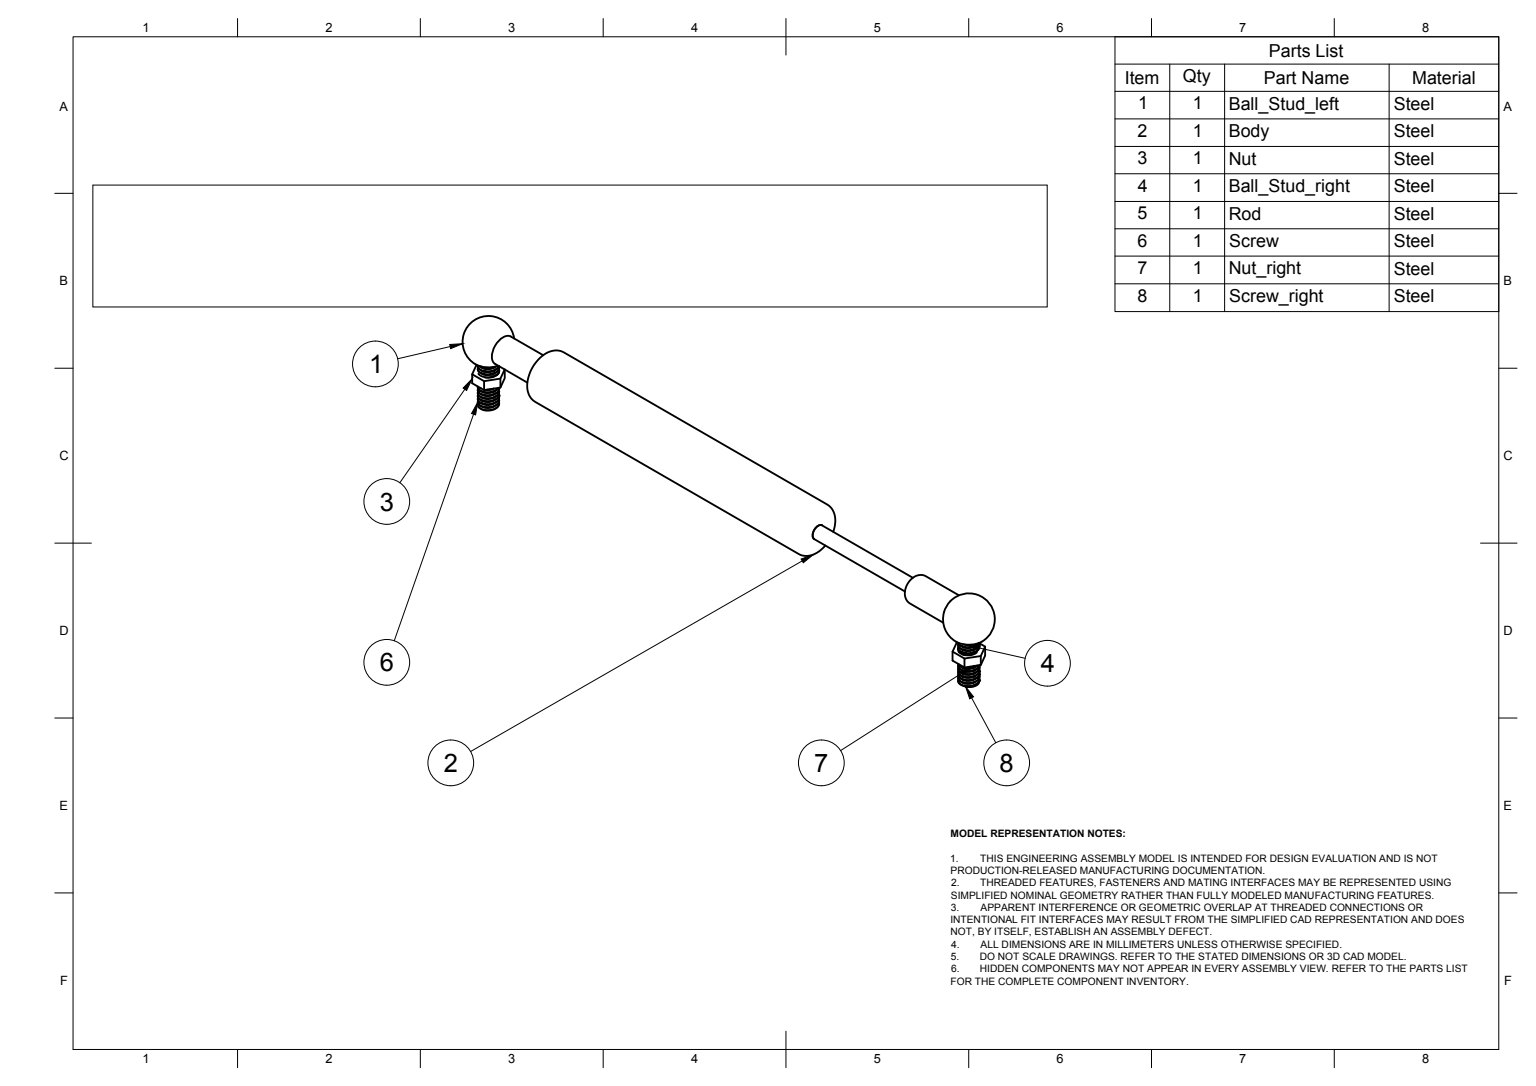
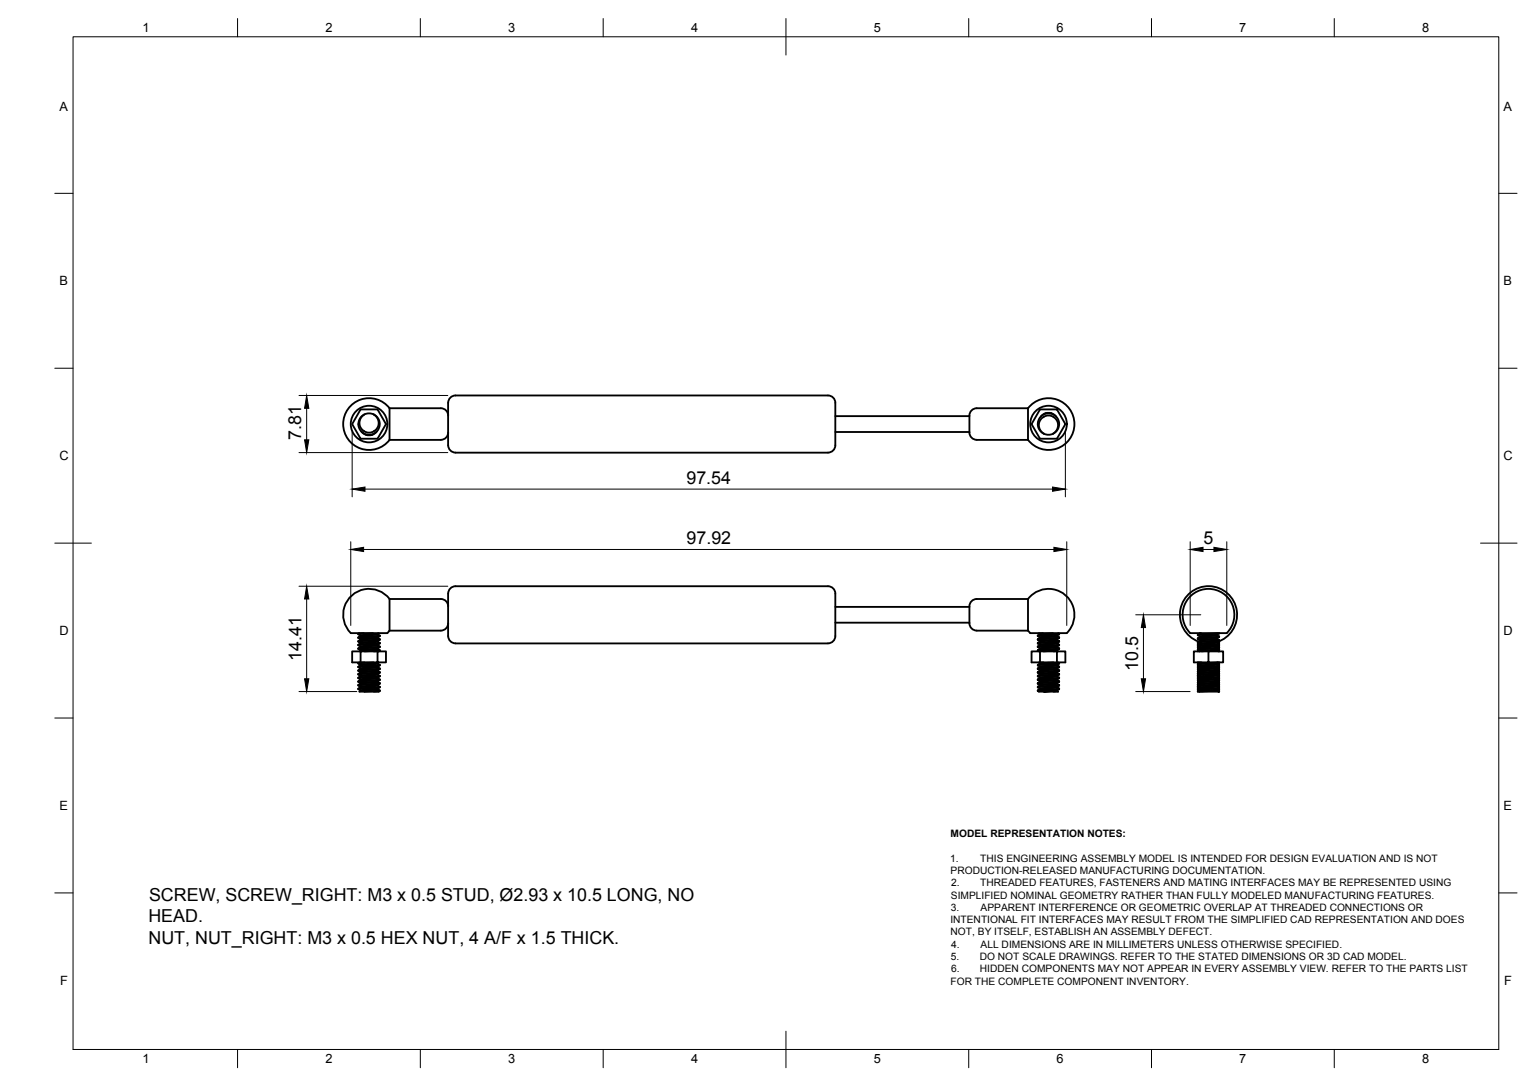
ISO-10303-21;
HEADER;
/* Generated by software containing ST-Developer
 * from STEP Tools, Inc. (www.steptools.com) 
 */

FILE_DESCRIPTION(
/* description */ (''),
/* implementation_level */ '2;1');

FILE_NAME(
/* name */ 'BR-109',
/* time_stamp */ '2026-10-04T22:13:49-07:00',
/* author */ (''),
/* organization */ (''),
/* preprocessor_version */ 'ST-DEVELOPER v20.2',
/* originating_system */ 'Autodesk Translation Framework v15.15.0.0',
/* authorisation */ '');

FILE_SCHEMA (('AUTOMOTIVE_DESIGN { 1 0 10303 214 3 1 1 }'));
ENDSEC;

DATA;
#10=MECHANICAL_DESIGN_GEOMETRIC_PRESENTATION_REPRESENTATION('',(#361,#362,
#363,#364,#365,#366,#367,#368,#369),#40734);
#11=ITEM_DEFINED_TRANSFORMATION($,$,#3265,#3474);
#12=ITEM_DEFINED_TRANSFORMATION($,$,#3284,#3475);
#13=ITEM_DEFINED_TRANSFORMATION($,$,#3299,#3476);
#14=ITEM_DEFINED_TRANSFORMATION($,$,#3320,#3477);
#15=ITEM_DEFINED_TRANSFORMATION($,$,#3340,#3478);
#16=ITEM_DEFINED_TRANSFORMATION($,$,#3351,#3479);
#17=ITEM_DEFINED_TRANSFORMATION($,$,#3402,#3480);
#18=ITEM_DEFINED_TRANSFORMATION($,$,#3423,#3481);
#19=(
REPRESENTATION_RELATIONSHIP($,$,#40766,#40765)
REPRESENTATION_RELATIONSHIP_WITH_TRANSFORMATION(#11)
SHAPE_REPRESENTATION_RELATIONSHIP()
);
#20=(
REPRESENTATION_RELATIONSHIP($,$,#40767,#40765)
REPRESENTATION_RELATIONSHIP_WITH_TRANSFORMATION(#12)
SHAPE_REPRESENTATION_RELATIONSHIP()
);
#21=(
REPRESENTATION_RELATIONSHIP($,$,#40768,#40765)
REPRESENTATION_RELATIONSHIP_WITH_TRANSFORMATION(#13)
SHAPE_REPRESENTATION_RELATIONSHIP()
);
#22=(
REPRESENTATION_RELATIONSHIP($,$,#40769,#40765)
REPRESENTATION_RELATIONSHIP_WITH_TRANSFORMATION(#14)
SHAPE_REPRESENTATION_RELATIONSHIP()
);
#23=(
REPRESENTATION_RELATIONSHIP($,$,#40770,#40765)
REPRESENTATION_RELATIONSHIP_WITH_TRANSFORMATION(#15)
SHAPE_REPRESENTATION_RELATIONSHIP()
);
#24=(
REPRESENTATION_RELATIONSHIP($,$,#40771,#40765)
REPRESENTATION_RELATIONSHIP_WITH_TRANSFORMATION(#16)
SHAPE_REPRESENTATION_RELATIONSHIP()
);
#25=(
REPRESENTATION_RELATIONSHIP($,$,#40772,#40765)
REPRESENTATION_RELATIONSHIP_WITH_TRANSFORMATION(#17)
SHAPE_REPRESENTATION_RELATIONSHIP()
);
#26=(
REPRESENTATION_RELATIONSHIP($,$,#40773,#40765)
REPRESENTATION_RELATIONSHIP_WITH_TRANSFORMATION(#18)
SHAPE_REPRESENTATION_RELATIONSHIP()
);
#27=CONTEXT_DEPENDENT_SHAPE_REPRESENTATION(#19,#40757);
#28=CONTEXT_DEPENDENT_SHAPE_REPRESENTATION(#20,#40758);
#29=CONTEXT_DEPENDENT_SHAPE_REPRESENTATION(#21,#40759);
#30=CONTEXT_DEPENDENT_SHAPE_REPRESENTATION(#22,#40760);
#31=CONTEXT_DEPENDENT_SHAPE_REPRESENTATION(#23,#40761);
#32=CONTEXT_DEPENDENT_SHAPE_REPRESENTATION(#24,#40762);
#33=CONTEXT_DEPENDENT_SHAPE_REPRESENTATION(#25,#40763);
#34=CONTEXT_DEPENDENT_SHAPE_REPRESENTATION(#26,#40764);
#35=NEXT_ASSEMBLY_USAGE_OCCURRENCE('Ball_Stud_left:1',
'Ball_Stud_left:1','Ball_Stud_left:1',#40775,#40776,'Ball_Stud_left:1');
#36=NEXT_ASSEMBLY_USAGE_OCCURRENCE('Body:1','Body:1','Body:1',#40775,#40777,
'Body:1');
#37=NEXT_ASSEMBLY_USAGE_OCCURRENCE('Nut:1','Nut:1','Nut:1',#40775,#40778,
'Nut:1');
#38=NEXT_ASSEMBLY_USAGE_OCCURRENCE('Ball_Stud_right:1',
'Ball_Stud_right:1','Ball_Stud_right:1',#40775,#40779,
'Ball_Stud_right:1');
#39=NEXT_ASSEMBLY_USAGE_OCCURRENCE('Rod:1','Rod:1','Rod:1',#40775,#40780,
'Rod:1');
#40=NEXT_ASSEMBLY_USAGE_OCCURRENCE('Screw:1','Screw:1','Screw:1',#40775,
#40781,'Screw:1');
#41=NEXT_ASSEMBLY_USAGE_OCCURRENCE('Nut_right:1','Nut_right:1',
'Nut_right:1',#40775,#40782,'Nut_right:1');
#42=NEXT_ASSEMBLY_USAGE_OCCURRENCE('Screw_right:1','Screw_right:1',
'Screw_right:1',#40775,#40783,'Screw_right:1');
#43=B_SPLINE_SURFACE_WITH_KNOTS('',3,3,((#5877,#5878,#5879,#5880,#5881,
#5882,#5883,#5884,#5885,#5886,#5887,#5888,#5889,#5890,#5891,#5892,#5893,
#5894,#5895,#5896,#5897,#5898,#5899,#5900),(#5901,#5902,#5903,#5904,#5905,
#5906,#5907,#5908,#5909,#5910,#5911,#5912,#5913,#5914,#5915,#5916,#5917,
#5918,#5919,#5920,#5921,#5922,#5923,#5924),(#5925,#5926,#5927,#5928,#5929,
#5930,#5931,#5932,#5933,#5934,#5935,#5936,#5937,#5938,#5939,#5940,#5941,
#5942,#5943,#5944,#5945,#5946,#5947,#5948),(#5949,#5950,#5951,#5952,#5953,
#5954,#5955,#5956,#5957,#5958,#5959,#5960,#5961,#5962,#5963,#5964,#5965,
#5966,#5967,#5968,#5969,#5970,#5971,#5972)),.UNSPECIFIED.,.F.,.F.,.F.,(4,
4),(4,1,1,1,1,1,1,1,1,1,1,1,1,1,1,1,1,1,1,1,1,4),(-0.000258182183401192,
0.0323763819078579),(11.855103081396,12.8491769023077,13.8429925410361,
14.8368081797645,15.8306238184928,16.8244394572212,17.8182550959496,18.8120707346779,
19.8058863734063,20.7997020121347,21.793517650863,22.7873332895914,23.7811489283198,
24.7749645670481,25.7687802057765,26.7625958445049,27.7564114832332,28.7502271219616,
29.74404276069,30.7378583994183,31.7316740381467,32.725489676875),
 .UNSPECIFIED.);
#44=B_SPLINE_SURFACE_WITH_KNOTS('',3,3,((#6139,#6140,#6141,#6142,#6143,
#6144,#6145,#6146,#6147,#6148,#6149,#6150,#6151,#6152,#6153,#6154,#6155,
#6156,#6157,#6158,#6159,#6160,#6161,#6162),(#6163,#6164,#6165,#6166,#6167,
#6168,#6169,#6170,#6171,#6172,#6173,#6174,#6175,#6176,#6177,#6178,#6179,
#6180,#6181,#6182,#6183,#6184,#6185,#6186),(#6187,#6188,#6189,#6190,#6191,
#6192,#6193,#6194,#6195,#6196,#6197,#6198,#6199,#6200,#6201,#6202,#6203,
#6204,#6205,#6206,#6207,#6208,#6209,#6210),(#6211,#6212,#6213,#6214,#6215,
#6216,#6217,#6218,#6219,#6220,#6221,#6222,#6223,#6224,#6225,#6226,#6227,
#6228,#6229,#6230,#6231,#6232,#6233,#6234)),.UNSPECIFIED.,.F.,.F.,.F.,(4,
4),(4,1,1,1,1,1,1,1,1,1,1,1,1,1,1,1,1,1,1,1,1,4),(-0.000227807970484936,
0.0323629493365531),(14.3984001269719,15.3922157657002,16.3860314044286,
17.379847043157,18.3736626818853,19.3674783206137,20.3612939593421,21.3551095980704,
22.3489252367988,23.3427408755272,24.3365565142555,25.3303721529839,26.3241877917123,
27.3180034304406,28.311819069169,29.3056347078974,30.2994503466257,31.2932659853541,
32.2870816240825,33.2808972628108,34.2747129015392,35.2685285402676),
 .UNSPECIFIED.);
#45=B_SPLINE_SURFACE_WITH_KNOTS('',3,3,((#19059,#19060,#19061,#19062,#19063,
#19064,#19065,#19066,#19067,#19068,#19069,#19070,#19071,#19072,#19073,#19074,
#19075,#19076,#19077,#19078,#19079,#19080,#19081,#19082,#19083,#19084,#19085,
#19086,#19087,#19088,#19089,#19090,#19091,#19092,#19093,#19094,#19095,#19096,
#19097,#19098,#19099,#19100,#19101,#19102,#19103,#19104,#19105,#19106,#19107,
#19108,#19109,#19110,#19111,#19112,#19113,#19114,#19115,#19116,#19117,#19118,
#19119,#19120,#19121,#19122,#19123,#19124,#19125,#19126,#19127,#19128,#19129,
#19130,#19131,#19132,#19133,#19134,#19135,#19136,#19137,#19138,#19139,#19140,
#19141,#19142,#19143,#19144,#19145,#19146,#19147,#19148,#19149,#19150,#19151,
#19152,#19153,#19154,#19155,#19156,#19157,#19158,#19159,#19160,#19161,#19162,
#19163,#19164,#19165,#19166,#19167,#19168,#19169,#19170,#19171,#19172,#19173,
#19174,#19175,#19176,#19177,#19178,#19179,#19180,#19181,#19182,#19183,#19184,
#19185,#19186,#19187,#19188,#19189,#19190,#19191,#19192,#19193,#19194,#19195,
#19196),(#19197,#19198,#19199,#19200,#19201,#19202,#19203,#19204,#19205,
#19206,#19207,#19208,#19209,#19210,#19211,#19212,#19213,#19214,#19215,#19216,
#19217,#19218,#19219,#19220,#19221,#19222,#19223,#19224,#19225,#19226,#19227,
#19228,#19229,#19230,#19231,#19232,#19233,#19234,#19235,#19236,#19237,#19238,
#19239,#19240,#19241,#19242,#19243,#19244,#19245,#19246,#19247,#19248,#19249,
#19250,#19251,#19252,#19253,#19254,#19255,#19256,#19257,#19258,#19259,#19260,
#19261,#19262,#19263,#19264,#19265,#19266,#19267,#19268,#19269,#19270,#19271,
#19272,#19273,#19274,#19275,#19276,#19277,#19278,#19279,#19280,#19281,#19282,
#19283,#19284,#19285,#19286,#19287,#19288,#19289,#19290,#19291,#19292,#19293,
#19294,#19295,#19296,#19297,#19298,#19299,#19300,#19301,#19302,#19303,#19304,
#19305,#19306,#19307,#19308,#19309,#19310,#19311,#19312,#19313,#19314,#19315,
#19316,#19317,#19318,#19319,#19320,#19321,#19322,#19323,#19324,#19325,#19326,
#19327,#19328,#19329,#19330,#19331,#19332,#19333,#19334),(#19335,#19336,
#19337,#19338,#19339,#19340,#19341,#19342,#19343,#19344,#19345,#19346,#19347,
#19348,#19349,#19350,#19351,#19352,#19353,#19354,#19355,#19356,#19357,#19358,
#19359,#19360,#19361,#19362,#19363,#19364,#19365,#19366,#19367,#19368,#19369,
#19370,#19371,#19372,#19373,#19374,#19375,#19376,#19377,#19378,#19379,#19380,
#19381,#19382,#19383,#19384,#19385,#19386,#19387,#19388,#19389,#19390,#19391,
#19392,#19393,#19394,#19395,#19396,#19397,#19398,#19399,#19400,#19401,#19402,
#19403,#19404,#19405,#19406,#19407,#19408,#19409,#19410,#19411,#19412,#19413,
#19414,#19415,#19416,#19417,#19418,#19419,#19420,#19421,#19422,#19423,#19424,
#19425,#19426,#19427,#19428,#19429,#19430,#19431,#19432,#19433,#19434,#19435,
#19436,#19437,#19438,#19439,#19440,#19441,#19442,#19443,#19444,#19445,#19446,
#19447,#19448,#19449,#19450,#19451,#19452,#19453,#19454,#19455,#19456,#19457,
#19458,#19459,#19460,#19461,#19462,#19463,#19464,#19465,#19466,#19467,#19468,
#19469,#19470,#19471,#19472),(#19473,#19474,#19475,#19476,#19477,#19478,
#19479,#19480,#19481,#19482,#19483,#19484,#19485,#19486,#19487,#19488,#19489,
#19490,#19491,#19492,#19493,#19494,#19495,#19496,#19497,#19498,#19499,#19500,
#19501,#19502,#19503,#19504,#19505,#19506,#19507,#19508,#19509,#19510,#19511,
#19512,#19513,#19514,#19515,#19516,#19517,#19518,#19519,#19520,#19521,#19522,
#19523,#19524,#19525,#19526,#19527,#19528,#19529,#19530,#19531,#19532,#19533,
#19534,#19535,#19536,#19537,#19538,#19539,#19540,#19541,#19542,#19543,#19544,
#19545,#19546,#19547,#19548,#19549,#19550,#19551,#19552,#19553,#19554,#19555,
#19556,#19557,#19558,#19559,#19560,#19561,#19562,#19563,#19564,#19565,#19566,
#19567,#19568,#19569,#19570,#19571,#19572,#19573,#19574,#19575,#19576,#19577,
#19578,#19579,#19580,#19581,#19582,#19583,#19584,#19585,#19586,#19587,#19588,
#19589,#19590,#19591,#19592,#19593,#19594,#19595,#19596,#19597,#19598,#19599,
#19600,#19601,#19602,#19603,#19604,#19605,#19606,#19607,#19608,#19609,#19610)),
 .UNSPECIFIED.,.F.,.F.,.F.,(4,4),(4,1,1,1,1,1,1,1,1,1,1,1,1,1,1,1,1,1,1,
1,1,1,1,1,1,1,1,1,1,1,1,1,1,1,1,1,1,1,1,1,1,1,1,1,1,1,1,1,1,1,1,1,1,1,1,
1,1,1,1,1,1,1,1,1,1,1,1,1,1,1,1,1,1,1,1,1,1,1,1,1,1,1,1,1,1,1,1,1,1,1,1,
1,1,1,1,1,1,1,1,1,1,1,1,1,1,1,1,1,1,1,1,1,1,1,1,1,1,1,1,1,1,1,1,1,1,1,1,
1,1,1,1,1,1,1,1,4),(-0.000231142210478152,0.0332102052225793),(8.30203615430837,
9.29477737004237,10.2875185857764,11.2802598015104,12.2730010172444,13.2657422329784,
14.2584834487124,15.2512246644464,16.2439658801804,17.2367070959144,18.2294483116484,
19.2221895273825,20.2149307431165,21.2076719588505,22.2004131745845,23.1931543903185,
24.1858956060525,25.1786368217865,26.1713780375205,27.1641192532545,28.1568604689885,
29.1496016847225,30.1423429004565,31.1350841161905,32.1278253319246,33.1205665476586,
34.1133077633926,35.1060489791266,36.0987901948606,37.0915314105946,38.0842726263286,
39.0770138420626,40.0697550577966,41.0624962735306,42.0552374892646,43.0479787049986,
44.0407199207326,45.0334611364667,46.0262023522007,47.0189435679347,48.0116847836687,
49.0044259994027,49.9971672151367,50.9899084308707,51.9826496466047,52.9753908623387,
53.9681320780727,54.9608732938067,55.9536145095407,56.9463557252747,57.9390969410088,
58.9318381567428,59.9245793724768,60.9173205882108,61.9100618039448,62.9028030196788,
63.8955442354128,64.8882854511468,65.8810266668808,66.8737678826148,67.8665090983488,
68.8592503140828,69.8519915298168,70.8447327455509,71.8374739612849,72.8302151770189,
73.8229563927529,74.8156976084869,75.8084388242209,76.8011800399549,77.7939212556889,
78.7866624714229,79.7794036871569,80.7721449028909,81.7648861186249,82.7576273343589,
83.750368550093,84.743109765827,85.735850981561,86.728592197295,87.721333413029,
88.714074628763,89.706815844497,90.699557060231,91.692298275965,92.685039491699,
93.677780707433,94.670521923167,95.663263138901,96.6560043546351,97.6487455703691,
98.6414867861031,99.6342280018371,100.626969217571,101.619710433305,102.612451649039,
103.605192864773,104.597934080507,105.590675296241,106.583416511975,107.576157727709,
108.568898943443,109.561640159177,110.554381374911,111.547122590645,112.539863806379,
113.532605022113,114.525346237847,115.518087453581,116.510828669315,117.503569885049,
118.496311100783,119.489052316517,120.481793532251,121.474534747985,122.467275963719,
123.460017179453,124.452758395187,125.445499610921,126.438240826655,127.430982042389,
128.423723258123,129.416464473857,130.409205689591,131.401946905325,132.394688121059,
133.387429336793,134.380170552527,135.372911768261,136.365652983995,137.358394199729,
138.351135415463,139.343876631197,140.336617846931,141.329359062665,142.322331420609),
 .UNSPECIFIED.);
#46=B_SPLINE_SURFACE_WITH_KNOTS('',3,3,((#19774,#19775,#19776,#19777,#19778,
#19779,#19780,#19781,#19782,#19783,#19784,#19785,#19786,#19787,#19788,#19789,
#19790,#19791,#19792,#19793,#19794,#19795,#19796,#19797,#19798,#19799,#19800,
#19801,#19802,#19803,#19804,#19805,#19806,#19807,#19808,#19809,#19810,#19811,
#19812,#19813,#19814,#19815,#19816,#19817,#19818,#19819,#19820,#19821,#19822,
#19823,#19824,#19825,#19826,#19827,#19828,#19829,#19830,#19831,#19832,#19833,
#19834,#19835,#19836,#19837,#19838,#19839,#19840,#19841,#19842,#19843,#19844,
#19845,#19846,#19847,#19848,#19849,#19850,#19851,#19852,#19853,#19854,#19855,
#19856,#19857,#19858,#19859,#19860,#19861,#19862,#19863,#19864,#19865,#19866,
#19867,#19868,#19869,#19870,#19871,#19872,#19873,#19874,#19875,#19876,#19877,
#19878,#19879,#19880,#19881,#19882,#19883,#19884,#19885,#19886,#19887,#19888,
#19889,#19890,#19891,#19892,#19893,#19894,#19895,#19896,#19897,#19898,#19899,
#19900,#19901,#19902,#19903,#19904,#19905,#19906,#19907,#19908,#19909,#19910,
#19911),(#19912,#19913,#19914,#19915,#19916,#19917,#19918,#19919,#19920,
#19921,#19922,#19923,#19924,#19925,#19926,#19927,#19928,#19929,#19930,#19931,
#19932,#19933,#19934,#19935,#19936,#19937,#19938,#19939,#19940,#19941,#19942,
#19943,#19944,#19945,#19946,#19947,#19948,#19949,#19950,#19951,#19952,#19953,
#19954,#19955,#19956,#19957,#19958,#19959,#19960,#19961,#19962,#19963,#19964,
#19965,#19966,#19967,#19968,#19969,#19970,#19971,#19972,#19973,#19974,#19975,
#19976,#19977,#19978,#19979,#19980,#19981,#19982,#19983,#19984,#19985,#19986,
#19987,#19988,#19989,#19990,#19991,#19992,#19993,#19994,#19995,#19996,#19997,
#19998,#19999,#20000,#20001,#20002,#20003,#20004,#20005,#20006,#20007,#20008,
#20009,#20010,#20011,#20012,#20013,#20014,#20015,#20016,#20017,#20018,#20019,
#20020,#20021,#20022,#20023,#20024,#20025,#20026,#20027,#20028,#20029,#20030,
#20031,#20032,#20033,#20034,#20035,#20036,#20037,#20038,#20039,#20040,#20041,
#20042,#20043,#20044,#20045,#20046,#20047,#20048,#20049),(#20050,#20051,
#20052,#20053,#20054,#20055,#20056,#20057,#20058,#20059,#20060,#20061,#20062,
#20063,#20064,#20065,#20066,#20067,#20068,#20069,#20070,#20071,#20072,#20073,
#20074,#20075,#20076,#20077,#20078,#20079,#20080,#20081,#20082,#20083,#20084,
#20085,#20086,#20087,#20088,#20089,#20090,#20091,#20092,#20093,#20094,#20095,
#20096,#20097,#20098,#20099,#20100,#20101,#20102,#20103,#20104,#20105,#20106,
#20107,#20108,#20109,#20110,#20111,#20112,#20113,#20114,#20115,#20116,#20117,
#20118,#20119,#20120,#20121,#20122,#20123,#20124,#20125,#20126,#20127,#20128,
#20129,#20130,#20131,#20132,#20133,#20134,#20135,#20136,#20137,#20138,#20139,
#20140,#20141,#20142,#20143,#20144,#20145,#20146,#20147,#20148,#20149,#20150,
#20151,#20152,#20153,#20154,#20155,#20156,#20157,#20158,#20159,#20160,#20161,
#20162,#20163,#20164,#20165,#20166,#20167,#20168,#20169,#20170,#20171,#20172,
#20173,#20174,#20175,#20176,#20177,#20178,#20179,#20180,#20181,#20182,#20183,
#20184,#20185,#20186,#20187),(#20188,#20189,#20190,#20191,#20192,#20193,
#20194,#20195,#20196,#20197,#20198,#20199,#20200,#20201,#20202,#20203,#20204,
#20205,#20206,#20207,#20208,#20209,#20210,#20211,#20212,#20213,#20214,#20215,
#20216,#20217,#20218,#20219,#20220,#20221,#20222,#20223,#20224,#20225,#20226,
#20227,#20228,#20229,#20230,#20231,#20232,#20233,#20234,#20235,#20236,#20237,
#20238,#20239,#20240,#20241,#20242,#20243,#20244,#20245,#20246,#20247,#20248,
#20249,#20250,#20251,#20252,#20253,#20254,#20255,#20256,#20257,#20258,#20259,
#20260,#20261,#20262,#20263,#20264,#20265,#20266,#20267,#20268,#20269,#20270,
#20271,#20272,#20273,#20274,#20275,#20276,#20277,#20278,#20279,#20280,#20281,
#20282,#20283,#20284,#20285,#20286,#20287,#20288,#20289,#20290,#20291,#20292,
#20293,#20294,#20295,#20296,#20297,#20298,#20299,#20300,#20301,#20302,#20303,
#20304,#20305,#20306,#20307,#20308,#20309,#20310,#20311,#20312,#20313,#20314,
#20315,#20316,#20317,#20318,#20319,#20320,#20321,#20322,#20323,#20324,#20325)),
 .UNSPECIFIED.,.F.,.F.,.F.,(4,4),(4,1,1,1,1,1,1,1,1,1,1,1,1,1,1,1,1,1,1,
1,1,1,1,1,1,1,1,1,1,1,1,1,1,1,1,1,1,1,1,1,1,1,1,1,1,1,1,1,1,1,1,1,1,1,1,
1,1,1,1,1,1,1,1,1,1,1,1,1,1,1,1,1,1,1,1,1,1,1,1,1,1,1,1,1,1,1,1,1,1,1,1,
1,1,1,1,1,1,1,1,1,1,1,1,1,1,1,1,1,1,1,1,1,1,1,1,1,1,1,1,1,1,1,1,1,1,1,1,
1,1,1,1,1,1,1,1,4),(-0.000203358763107571,0.0332327300170814),(11.6157025853675,
12.6086809632344,13.6014221789684,14.5941633947024,15.5869046104364,16.5796458261704,
17.5723870419044,18.5651282576385,19.5578694733725,20.5506106891065,21.5433519048405,
22.5360931205745,23.5288343363085,24.5215755520425,25.5143167677765,26.5070579835105,
27.4997991992445,28.4925404149785,29.4852816307125,30.4780228464465,31.4707640621806,
32.4635052779146,33.4562464936486,34.4489877093826,35.4417289251166,36.4344701408506,
37.4272113565846,38.4199525723186,39.4126937880526,40.4054350037866,41.3981762195206,
42.3909174352546,43.3836586509887,44.3763998667227,45.3691410824567,46.3618822981907,
47.3546235139247,48.3473647296587,49.3401059453927,50.3328471611267,51.3255883768607,
52.3183295925947,53.3110708083287,54.3038120240627,55.2965532397967,56.2892944555308,
57.2820356712648,58.2747768869988,59.2675181027328,60.2602593184668,61.2530005342008,
62.2457417499348,63.2384829656688,64.2312241814028,65.2239653971368,66.2167066128708,
67.2094478286048,68.2021890443388,69.1949302600729,70.1876714758069,71.1804126915409,
72.1731539072749,73.1658951230089,74.1586363387429,75.1513775544769,76.1441187702109,
77.1368599859449,78.1296012016789,79.1223424174129,80.1150836331469,81.107824848881,
82.100566064615,83.093307280349,84.086048496083,85.078789711817,86.071530927551,
87.064272143285,88.057013359019,89.049754574753,90.042495790487,91.035237006221,
92.027978221955,93.020719437689,94.0134606534231,95.0062018691571,95.9989430848911,
96.9916843006251,97.9844255163591,98.9771667320931,99.9699079478271,100.962649163561,
101.955390379295,102.948131595029,103.940872810763,104.933614026497,105.926355242231,
106.919096457965,107.911837673699,108.904578889433,109.897320105167,110.890061320901,
111.882802536635,112.875543752369,113.868284968103,114.861026183837,115.853767399571,
116.846508615305,117.839249831039,118.831991046773,119.824732262507,120.817473478241,
121.810214693975,122.802955909709,123.795697125443,124.788438341177,125.781179556911,
126.773920772645,127.766661988379,128.759403204113,129.752144419847,130.744885635581,
131.737626851315,132.730368067049,133.723109282783,134.715850498517,135.708591714251,
136.701332929985,137.694074145719,138.686815361453,139.679556577187,140.672297792921,
141.665039008655,142.657780224389,143.650521440123,144.643262655857,145.636003871591),
 .UNSPECIFIED.);
#47=B_SPLINE_SURFACE_WITH_KNOTS('',3,3,((#22334,#22335,#22336,#22337,#22338,
#22339,#22340,#22341,#22342,#22343,#22344,#22345,#22346,#22347,#22348,#22349,
#22350,#22351,#22352,#22353,#22354,#22355,#22356,#22357),(#22358,#22359,
#22360,#22361,#22362,#22363,#22364,#22365,#22366,#22367,#22368,#22369,#22370,
#22371,#22372,#22373,#22374,#22375,#22376,#22377,#22378,#22379,#22380,#22381),
(#22382,#22383,#22384,#22385,#22386,#22387,#22388,#22389,#22390,#22391,
#22392,#22393,#22394,#22395,#22396,#22397,#22398,#22399,#22400,#22401,#22402,
#22403,#22404,#22405),(#22406,#22407,#22408,#22409,#22410,#22411,#22412,
#22413,#22414,#22415,#22416,#22417,#22418,#22419,#22420,#22421,#22422,#22423,
#22424,#22425,#22426,#22427,#22428,#22429)),.UNSPECIFIED.,.F.,.F.,.F.,(4,
4),(4,1,1,1,1,1,1,1,1,1,1,1,1,1,1,1,1,1,1,1,1,4),(-0.000270002866089487,
0.0323833849707337),(11.8550912607133,12.8491769023077,13.8429925410361,
14.8368081797645,15.8306238184928,16.8244394572212,17.8182550959496,18.8120707346779,
19.8058863734063,20.7997020121347,21.793517650863,22.7873332895914,23.7811489283198,
24.7749645670481,25.7687802057765,26.7625958445049,27.7564114832332,28.7502271219616,
29.74404276069,30.7378583994183,31.7316740381467,32.725489676875),
 .UNSPECIFIED.);
#48=B_SPLINE_SURFACE_WITH_KNOTS('',3,3,((#22596,#22597,#22598,#22599,#22600,
#22601,#22602,#22603,#22604,#22605,#22606,#22607,#22608,#22609,#22610,#22611,
#22612,#22613,#22614,#22615,#22616,#22617,#22618,#22619),(#22620,#22621,
#22622,#22623,#22624,#22625,#22626,#22627,#22628,#22629,#22630,#22631,#22632,
#22633,#22634,#22635,#22636,#22637,#22638,#22639,#22640,#22641,#22642,#22643),
(#22644,#22645,#22646,#22647,#22648,#22649,#22650,#22651,#22652,#22653,
#22654,#22655,#22656,#22657,#22658,#22659,#22660,#22661,#22662,#22663,#22664,
#22665,#22666,#22667),(#22668,#22669,#22670,#22671,#22672,#22673,#22674,
#22675,#22676,#22677,#22678,#22679,#22680,#22681,#22682,#22683,#22684,#22685,
#22686,#22687,#22688,#22689,#22690,#22691)),.UNSPECIFIED.,.F.,.F.,.F.,(4,
4),(4,1,1,1,1,1,1,1,1,1,1,1,1,1,1,1,1,1,1,1,1,4),(-0.000235328167620964,
0.0323617480244609),(14.3982993132237,15.3922157657002,16.3860314044286,
17.379847043157,18.3736626818853,19.3674783206137,20.3612939593421,21.3551095980704,
22.3489252367988,23.3427408755272,24.3365565142555,25.3303721529839,26.3241877917123,
27.3180034304406,28.311819069169,29.3056347078974,30.2994503466257,31.2932659853541,
32.2870816240825,33.2808972628108,34.2747129015392,35.2685285402676),
 .UNSPECIFIED.);
#49=B_SPLINE_SURFACE_WITH_KNOTS('',3,3,((#39281,#39282,#39283,#39284,#39285,
#39286,#39287,#39288,#39289,#39290,#39291,#39292,#39293,#39294,#39295,#39296,
#39297,#39298,#39299,#39300,#39301,#39302,#39303,#39304,#39305,#39306,#39307,
#39308,#39309,#39310,#39311,#39312,#39313,#39314,#39315,#39316,#39317,#39318,
#39319,#39320,#39321,#39322,#39323,#39324,#39325,#39326,#39327,#39328,#39329,
#39330,#39331,#39332,#39333,#39334,#39335,#39336,#39337,#39338,#39339,#39340,
#39341,#39342,#39343,#39344,#39345,#39346,#39347,#39348,#39349,#39350,#39351,
#39352,#39353,#39354,#39355,#39356,#39357,#39358,#39359,#39360,#39361,#39362,
#39363,#39364,#39365,#39366,#39367,#39368,#39369,#39370,#39371,#39372,#39373,
#39374,#39375,#39376,#39377,#39378,#39379,#39380,#39381,#39382,#39383,#39384,
#39385,#39386,#39387,#39388,#39389,#39390,#39391,#39392,#39393,#39394,#39395,
#39396,#39397,#39398,#39399,#39400,#39401,#39402,#39403,#39404,#39405,#39406,
#39407,#39408,#39409,#39410,#39411,#39412,#39413,#39414,#39415,#39416,#39417,
#39418),(#39419,#39420,#39421,#39422,#39423,#39424,#39425,#39426,#39427,
#39428,#39429,#39430,#39431,#39432,#39433,#39434,#39435,#39436,#39437,#39438,
#39439,#39440,#39441,#39442,#39443,#39444,#39445,#39446,#39447,#39448,#39449,
#39450,#39451,#39452,#39453,#39454,#39455,#39456,#39457,#39458,#39459,#39460,
#39461,#39462,#39463,#39464,#39465,#39466,#39467,#39468,#39469,#39470,#39471,
#39472,#39473,#39474,#39475,#39476,#39477,#39478,#39479,#39480,#39481,#39482,
#39483,#39484,#39485,#39486,#39487,#39488,#39489,#39490,#39491,#39492,#39493,
#39494,#39495,#39496,#39497,#39498,#39499,#39500,#39501,#39502,#39503,#39504,
#39505,#39506,#39507,#39508,#39509,#39510,#39511,#39512,#39513,#39514,#39515,
#39516,#39517,#39518,#39519,#39520,#39521,#39522,#39523,#39524,#39525,#39526,
#39527,#39528,#39529,#39530,#39531,#39532,#39533,#39534,#39535,#39536,#39537,
#39538,#39539,#39540,#39541,#39542,#39543,#39544,#39545,#39546,#39547,#39548,
#39549,#39550,#39551,#39552,#39553,#39554,#39555,#39556),(#39557,#39558,
#39559,#39560,#39561,#39562,#39563,#39564,#39565,#39566,#39567,#39568,#39569,
#39570,#39571,#39572,#39573,#39574,#39575,#39576,#39577,#39578,#39579,#39580,
#39581,#39582,#39583,#39584,#39585,#39586,#39587,#39588,#39589,#39590,#39591,
#39592,#39593,#39594,#39595,#39596,#39597,#39598,#39599,#39600,#39601,#39602,
#39603,#39604,#39605,#39606,#39607,#39608,#39609,#39610,#39611,#39612,#39613,
#39614,#39615,#39616,#39617,#39618,#39619,#39620,#39621,#39622,#39623,#39624,
#39625,#39626,#39627,#39628,#39629,#39630,#39631,#39632,#39633,#39634,#39635,
#39636,#39637,#39638,#39639,#39640,#39641,#39642,#39643,#39644,#39645,#39646,
#39647,#39648,#39649,#39650,#39651,#39652,#39653,#39654,#39655,#39656,#39657,
#39658,#39659,#39660,#39661,#39662,#39663,#39664,#39665,#39666,#39667,#39668,
#39669,#39670,#39671,#39672,#39673,#39674,#39675,#39676,#39677,#39678,#39679,
#39680,#39681,#39682,#39683,#39684,#39685,#39686,#39687,#39688,#39689,#39690,
#39691,#39692,#39693,#39694),(#39695,#39696,#39697,#39698,#39699,#39700,
#39701,#39702,#39703,#39704,#39705,#39706,#39707,#39708,#39709,#39710,#39711,
#39712,#39713,#39714,#39715,#39716,#39717,#39718,#39719,#39720,#39721,#39722,
#39723,#39724,#39725,#39726,#39727,#39728,#39729,#39730,#39731,#39732,#39733,
#39734,#39735,#39736,#39737,#39738,#39739,#39740,#39741,#39742,#39743,#39744,
#39745,#39746,#39747,#39748,#39749,#39750,#39751,#39752,#39753,#39754,#39755,
#39756,#39757,#39758,#39759,#39760,#39761,#39762,#39763,#39764,#39765,#39766,
#39767,#39768,#39769,#39770,#39771,#39772,#39773,#39774,#39775,#39776,#39777,
#39778,#39779,#39780,#39781,#39782,#39783,#39784,#39785,#39786,#39787,#39788,
#39789,#39790,#39791,#39792,#39793,#39794,#39795,#39796,#39797,#39798,#39799,
#39800,#39801,#39802,#39803,#39804,#39805,#39806,#39807,#39808,#39809,#39810,
#39811,#39812,#39813,#39814,#39815,#39816,#39817,#39818,#39819,#39820,#39821,
#39822,#39823,#39824,#39825,#39826,#39827,#39828,#39829,#39830,#39831,#39832)),
 .UNSPECIFIED.,.F.,.F.,.F.,(4,4),(4,1,1,1,1,1,1,1,1,1,1,1,1,1,1,1,1,1,1,
1,1,1,1,1,1,1,1,1,1,1,1,1,1,1,1,1,1,1,1,1,1,1,1,1,1,1,1,1,1,1,1,1,1,1,1,
1,1,1,1,1,1,1,1,1,1,1,1,1,1,1,1,1,1,1,1,1,1,1,1,1,1,1,1,1,1,1,1,1,1,1,1,
1,1,1,1,1,1,1,1,1,1,1,1,1,1,1,1,1,1,1,1,1,1,1,1,1,1,1,1,1,1,1,1,1,1,1,1,
1,1,1,1,1,1,1,1,4),(-0.000234148554357844,0.0332108863658552),(8.30203615430837,
9.29477737004237,10.2875185857764,11.2802598015104,12.2730010172444,13.2657422329784,
14.2584834487124,15.2512246644464,16.2439658801804,17.2367070959144,18.2294483116484,
19.2221895273825,20.2149307431165,21.2076719588505,22.2004131745845,23.1931543903185,
24.1858956060525,25.1786368217865,26.1713780375205,27.1641192532545,28.1568604689885,
29.1496016847225,30.1423429004565,31.1350841161905,32.1278253319246,33.1205665476586,
34.1133077633926,35.1060489791266,36.0987901948606,37.0915314105946,38.0842726263286,
39.0770138420626,40.0697550577966,41.0624962735306,42.0552374892646,43.0479787049986,
44.0407199207326,45.0334611364667,46.0262023522007,47.0189435679347,48.0116847836687,
49.0044259994027,49.9971672151367,50.9899084308707,51.9826496466047,52.9753908623387,
53.9681320780727,54.9608732938067,55.9536145095407,56.9463557252747,57.9390969410088,
58.9318381567428,59.9245793724768,60.9173205882108,61.9100618039448,62.9028030196788,
63.8955442354128,64.8882854511468,65.8810266668808,66.8737678826148,67.8665090983488,
68.8592503140828,69.8519915298168,70.8447327455509,71.8374739612849,72.8302151770189,
73.8229563927529,74.8156976084869,75.8084388242209,76.8011800399549,77.7939212556889,
78.7866624714229,79.7794036871569,80.7721449028909,81.7648861186249,82.7576273343589,
83.750368550093,84.743109765827,85.735850981561,86.728592197295,87.721333413029,
88.714074628763,89.706815844497,90.699557060231,91.692298275965,92.685039491699,
93.677780707433,94.670521923167,95.663263138901,96.6560043546351,97.6487455703691,
98.6414867861031,99.6342280018371,100.626969217571,101.619710433305,102.612451649039,
103.605192864773,104.597934080507,105.590675296241,106.583416511975,107.576157727709,
108.568898943443,109.561640159177,110.554381374911,111.547122590645,112.539863806379,
113.532605022113,114.525346237847,115.518087453581,116.510828669315,117.503569885049,
118.496311100783,119.489052316517,120.481793532251,121.474534747985,122.467275963719,
123.460017179453,124.452758395187,125.445499610921,126.438240826655,127.430982042389,
128.423723258123,129.416464473857,130.409205689591,131.401946905325,132.394688121059,
133.387429336793,134.380170552527,135.372911768261,136.365652983995,137.358394199729,
138.351135415463,139.343876631197,140.336617846931,141.329359062665,142.322334426953),
 .UNSPECIFIED.);
#50=B_SPLINE_SURFACE_WITH_KNOTS('',3,3,((#39993,#39994,#39995,#39996,#39997,
#39998,#39999,#40000,#40001,#40002,#40003,#40004,#40005,#40006,#40007,#40008,
#40009,#40010,#40011,#40012,#40013,#40014,#40015,#40016,#40017,#40018,#40019,
#40020,#40021,#40022,#40023,#40024,#40025,#40026,#40027,#40028,#40029,#40030,
#40031,#40032,#40033,#40034,#40035,#40036,#40037,#40038,#40039,#40040,#40041,
#40042,#40043,#40044,#40045,#40046,#40047,#40048,#40049,#40050,#40051,#40052,
#40053,#40054,#40055,#40056,#40057,#40058,#40059,#40060,#40061,#40062,#40063,
#40064,#40065,#40066,#40067,#40068,#40069,#40070,#40071,#40072,#40073,#40074,
#40075,#40076,#40077,#40078,#40079,#40080,#40081,#40082,#40083,#40084,#40085,
#40086,#40087,#40088,#40089,#40090,#40091,#40092,#40093,#40094,#40095,#40096,
#40097,#40098,#40099,#40100,#40101,#40102,#40103,#40104,#40105,#40106,#40107,
#40108,#40109,#40110,#40111,#40112,#40113,#40114,#40115,#40116,#40117,#40118,
#40119,#40120,#40121,#40122,#40123,#40124,#40125,#40126,#40127,#40128,#40129,
#40130),(#40131,#40132,#40133,#40134,#40135,#40136,#40137,#40138,#40139,
#40140,#40141,#40142,#40143,#40144,#40145,#40146,#40147,#40148,#40149,#40150,
#40151,#40152,#40153,#40154,#40155,#40156,#40157,#40158,#40159,#40160,#40161,
#40162,#40163,#40164,#40165,#40166,#40167,#40168,#40169,#40170,#40171,#40172,
#40173,#40174,#40175,#40176,#40177,#40178,#40179,#40180,#40181,#40182,#40183,
#40184,#40185,#40186,#40187,#40188,#40189,#40190,#40191,#40192,#40193,#40194,
#40195,#40196,#40197,#40198,#40199,#40200,#40201,#40202,#40203,#40204,#40205,
#40206,#40207,#40208,#40209,#40210,#40211,#40212,#40213,#40214,#40215,#40216,
#40217,#40218,#40219,#40220,#40221,#40222,#40223,#40224,#40225,#40226,#40227,
#40228,#40229,#40230,#40231,#40232,#40233,#40234,#40235,#40236,#40237,#40238,
#40239,#40240,#40241,#40242,#40243,#40244,#40245,#40246,#40247,#40248,#40249,
#40250,#40251,#40252,#40253,#40254,#40255,#40256,#40257,#40258,#40259,#40260,
#40261,#40262,#40263,#40264,#40265,#40266,#40267,#40268),(#40269,#40270,
#40271,#40272,#40273,#40274,#40275,#40276,#40277,#40278,#40279,#40280,#40281,
#40282,#40283,#40284,#40285,#40286,#40287,#40288,#40289,#40290,#40291,#40292,
#40293,#40294,#40295,#40296,#40297,#40298,#40299,#40300,#40301,#40302,#40303,
#40304,#40305,#40306,#40307,#40308,#40309,#40310,#40311,#40312,#40313,#40314,
#40315,#40316,#40317,#40318,#40319,#40320,#40321,#40322,#40323,#40324,#40325,
#40326,#40327,#40328,#40329,#40330,#40331,#40332,#40333,#40334,#40335,#40336,
#40337,#40338,#40339,#40340,#40341,#40342,#40343,#40344,#40345,#40346,#40347,
#40348,#40349,#40350,#40351,#40352,#40353,#40354,#40355,#40356,#40357,#40358,
#40359,#40360,#40361,#40362,#40363,#40364,#40365,#40366,#40367,#40368,#40369,
#40370,#40371,#40372,#40373,#40374,#40375,#40376,#40377,#40378,#40379,#40380,
#40381,#40382,#40383,#40384,#40385,#40386,#40387,#40388,#40389,#40390,#40391,
#40392,#40393,#40394,#40395,#40396,#40397,#40398,#40399,#40400,#40401,#40402,
#40403,#40404,#40405,#40406),(#40407,#40408,#40409,#40410,#40411,#40412,
#40413,#40414,#40415,#40416,#40417,#40418,#40419,#40420,#40421,#40422,#40423,
#40424,#40425,#40426,#40427,#40428,#40429,#40430,#40431,#40432,#40433,#40434,
#40435,#40436,#40437,#40438,#40439,#40440,#40441,#40442,#40443,#40444,#40445,
#40446,#40447,#40448,#40449,#40450,#40451,#40452,#40453,#40454,#40455,#40456,
#40457,#40458,#40459,#40460,#40461,#40462,#40463,#40464,#40465,#40466,#40467,
#40468,#40469,#40470,#40471,#40472,#40473,#40474,#40475,#40476,#40477,#40478,
#40479,#40480,#40481,#40482,#40483,#40484,#40485,#40486,#40487,#40488,#40489,
#40490,#40491,#40492,#40493,#40494,#40495,#40496,#40497,#40498,#40499,#40500,
#40501,#40502,#40503,#40504,#40505,#40506,#40507,#40508,#40509,#40510,#40511,
#40512,#40513,#40514,#40515,#40516,#40517,#40518,#40519,#40520,#40521,#40522,
#40523,#40524,#40525,#40526,#40527,#40528,#40529,#40530,#40531,#40532,#40533,
#40534,#40535,#40536,#40537,#40538,#40539,#40540,#40541,#40542,#40543,#40544)),
 .UNSPECIFIED.,.F.,.F.,.F.,(4,4),(4,1,1,1,1,1,1,1,1,1,1,1,1,1,1,1,1,1,1,
1,1,1,1,1,1,1,1,1,1,1,1,1,1,1,1,1,1,1,1,1,1,1,1,1,1,1,1,1,1,1,1,1,1,1,1,
1,1,1,1,1,1,1,1,1,1,1,1,1,1,1,1,1,1,1,1,1,1,1,1,1,1,1,1,1,1,1,1,1,1,1,1,
1,1,1,1,1,1,1,1,1,1,1,1,1,1,1,1,1,1,1,1,1,1,1,1,1,1,1,1,1,1,1,1,1,1,1,1,
1,1,1,1,1,1,1,1,4),(-0.000206153515366958,0.0332359307550877),(11.6156993846295,
12.6086809632344,13.6014221789684,14.5941633947024,15.5869046104364,16.5796458261704,
17.5723870419044,18.5651282576385,19.5578694733725,20.5506106891065,21.5433519048405,
22.5360931205745,23.5288343363085,24.5215755520425,25.5143167677765,26.5070579835105,
27.4997991992445,28.4925404149785,29.4852816307125,30.4780228464465,31.4707640621806,
32.4635052779146,33.4562464936486,34.4489877093826,35.4417289251166,36.4344701408506,
37.4272113565846,38.4199525723186,39.4126937880526,40.4054350037866,41.3981762195206,
42.3909174352546,43.3836586509887,44.3763998667227,45.3691410824567,46.3618822981907,
47.3546235139247,48.3473647296587,49.3401059453927,50.3328471611267,51.3255883768607,
52.3183295925947,53.3110708083287,54.3038120240627,55.2965532397967,56.2892944555308,
57.2820356712648,58.2747768869988,59.2675181027328,60.2602593184668,61.2530005342008,
62.2457417499348,63.2384829656688,64.2312241814028,65.2239653971368,66.2167066128708,
67.2094478286048,68.2021890443388,69.1949302600729,70.1876714758069,71.1804126915409,
72.1731539072749,73.1658951230089,74.1586363387429,75.1513775544769,76.1441187702109,
77.1368599859449,78.1296012016789,79.1223424174129,80.1150836331469,81.107824848881,
82.100566064615,83.093307280349,84.086048496083,85.078789711817,86.071530927551,
87.064272143285,88.057013359019,89.049754574753,90.042495790487,91.035237006221,
92.027978221955,93.020719437689,94.0134606534231,95.0062018691571,95.9989430848911,
96.9916843006251,97.9844255163591,98.9771667320931,99.9699079478271,100.962649163561,
101.955390379295,102.948131595029,103.940872810763,104.933614026497,105.926355242231,
106.919096457965,107.911837673699,108.904578889433,109.897320105167,110.890061320901,
111.882802536635,112.875543752369,113.868284968103,114.861026183837,115.853767399571,
116.846508615305,117.839249831039,118.831991046773,119.824732262507,120.817473478241,
121.810214693975,122.802955909709,123.795697125443,124.788438341177,125.781179556911,
126.773920772645,127.766661988379,128.759403204113,129.752144419847,130.744885635581,
131.737626851315,132.730368067049,133.723109282783,134.715850498517,135.708591714251,
136.701332929985,137.694074145719,138.686815361453,139.679556577187,140.672297792921,
141.665039008655,142.657780224389,143.650521440123,144.643262655857,145.636003871591),
 .UNSPECIFIED.);
#51=B_SPLINE_CURVE_WITH_KNOTS('',3,(#4121,#4122,#4123,#4124,#4125,#4126),
 .UNSPECIFIED.,.F.,.F.,(4,1,1,4),(30.4992669120821,30.7378583994183,31.7316740381467,
32.725489676875),.UNSPECIFIED.);
#52=B_SPLINE_CURVE_WITH_KNOTS('',3,(#4129,#4130,#4131,#4132,#4133,#4134,
#4135,#4136,#4137,#4138,#4139,#4140,#4141,#4142,#4143,#4144,#4145,#4146,
#4147,#4148,#4149,#4150,#4151,#4152,#4153,#4154,#4155,#4156,#4157,#4158,
#4159,#4160,#4161,#4162,#4163,#4164,#4165,#4166,#4167,#4168,#4169,#4170,
#4171,#4172,#4173,#4174,#4175,#4176,#4177,#4178,#4179,#4180,#4181,#4182,
#4183,#4184,#4185,#4186,#4187,#4188,#4189,#4190,#4191,#4192,#4193,#4194,
#4195,#4196,#4197,#4198,#4199,#4200,#4201,#4202,#4203,#4204),
 .UNSPECIFIED.,.F.,.F.,(4,3,3,3,3,3,3,3,3,3,3,3,3,3,3,3,3,3,3,3,3,3,3,3,
3,4),(30.5007322636873,30.6122727264591,30.7237376230315,30.8351702081999,
30.9496941524884,31.0612649927854,31.1772654890698,31.2932659853541,31.405444381662,
31.5174234643071,31.629291154361,31.7410902071455,31.8528632800448,31.9647326752084,
32.0766471573347,32.1887699843063,32.2870816240825,32.398548943329,32.5098233581226,
32.6209912335388,32.7320964774763,32.8431829042999,32.9543713853473,33.0656134824414,
33.1770570913779,33.2478062575977),.UNSPECIFIED.);
#53=B_SPLINE_CURVE_WITH_KNOTS('',3,(#4210,#4211,#4212,#4213,#4214,#4215,
#4216,#4217,#4218,#4219,#4220,#4221,#4222,#4223,#4224,#4225,#4226,#4227,
#4228,#4229,#4230,#4231,#4232,#4233,#4234,#4235,#4236,#4237,#4238,#4239,
#4240,#4241,#4242,#4243,#4244,#4245,#4246,#4247,#4248,#4249,#4250,#4251,
#4252,#4253,#4254,#4255,#4256,#4257,#4258,#4259,#4260,#4261,#4262,#4263,
#4264,#4265,#4266,#4267,#4268,#4269,#4270,#4271,#4272,#4273,#4274,#4275,
#4276,#4277,#4278,#4279,#4280,#4281,#4282,#4283,#4284,#4285,#4286,#4287,
#4288,#4289,#4290,#4291,#4292,#4293,#4294,#4295,#4296,#4297,#4298,#4299,
#4300,#4301,#4302,#4303,#4304,#4305,#4306,#4307,#4308,#4309,#4310,#4311,
#4312,#4313,#4314,#4315,#4316,#4317,#4318,#4319,#4320,#4321),
 .UNSPECIFIED.,.F.,.F.,(4,3,3,3,3,3,3,3,3,3,3,3,3,3,3,3,3,3,3,3,3,3,3,3,
3,3,3,3,3,3,3,3,3,3,3,3,3,4),(24.2171494664266,24.3287289861615,24.4404061429661,
24.5521266745184,24.6640652186713,24.7749645670481,24.8869176317094,24.9986729372709,
25.1103179593314,25.2218958291666,25.3334495814181,25.4451043023639,25.5568063273599,
25.668723124984,25.7687802057765,25.8807765547188,25.9925749208264,26.104262837802,
26.2158833658169,26.3274794682339,26.4391757243447,26.550918903972,26.6628756909807,
26.7625958445049,26.8745949120742,26.9863967358013,27.0980885559922,27.2097134207251,
27.3213142818085,27.4330159084715,27.5447648029427,27.6567278002384,27.7564114832332,
27.8729397438563,27.9891469003203,28.1051613568161,28.2209618754298,28.2743338823081),
 .UNSPECIFIED.);
#54=B_SPLINE_CURVE_WITH_KNOTS('',3,(#4322,#4323,#4324,#4325,#4326,#4327),
 .UNSPECIFIED.,.F.,.F.,(4,1,1,4),(28.2743354175824,28.7502271219616,29.74404276069,
30.4992669120821),.UNSPECIFIED.);
#55=B_SPLINE_CURVE_WITH_KNOTS('',3,(#4329,#4330,#4331,#4332,#4333,#4334,
#4335,#4336,#4337,#4338,#4339,#4340,#4341,#4342,#4343,#4344,#4345,#4346,
#4347,#4348,#4349,#4350,#4351,#4352,#4353,#4354,#4355,#4356,#4357,#4358,
#4359,#4360,#4361,#4362,#4363,#4364,#4365,#4366,#4367,#4368,#4369,#4370,
#4371,#4372,#4373,#4374,#4375,#4376,#4377,#4378,#4379,#4380,#4381,#4382,
#4383,#4384,#4385,#4386,#4387,#4388,#4389,#4390,#4391,#4392),
 .UNSPECIFIED.,.F.,.F.,(4,3,3,3,3,3,3,3,3,3,3,3,3,3,3,3,3,3,3,3,3,4),(28.2743338823081,
28.311819069169,28.4238155021246,28.5356139507129,28.6473019491837,28.7589225575854,
28.8705187391566,28.9822150718989,29.0939583268957,29.2059151862192,29.3056347078974,
29.4176340985753,29.5294362480819,29.6411283954428,29.7527535881624,29.8643547774776,
29.9760567301189,30.0878059498508,30.1997692670012,30.2994503466257,30.4112462518584,
30.5007322636873),.UNSPECIFIED.);
#56=B_SPLINE_CURVE_WITH_KNOTS('',3,(#4393,#4394,#4395,#4396,#4397,#4398,
#4399,#4400,#4401,#4402,#4403,#4404,#4405,#4406,#4407,#4408,#4409,#4410,
#4411,#4412,#4413,#4414,#4415,#4416,#4417,#4418,#4419,#4420,#4421,#4422,
#4423,#4424,#4425,#4426,#4427,#4428,#4429,#4430,#4431,#4432,#4433,#4434,
#4435,#4436,#4437,#4438,#4439,#4440,#4441,#4442,#4443,#4444,#4445,#4446,
#4447,#4448,#4449,#4450,#4451,#4452,#4453,#4454,#4455,#4456,#4457,#4458,
#4459,#4460,#4461,#4462,#4463,#4464,#4465,#4466,#4467,#4468,#4469,#4470,
#4471,#4472,#4473,#4474,#4475,#4476,#4477,#4478,#4479,#4480,#4481,#4482,
#4483,#4484,#4485,#4486,#4487,#4488,#4489,#4490,#4491,#4492,#4493,#4494,
#4495,#4496,#4497,#4498,#4499,#4500,#4501,#4502,#4503,#4504,#4505,#4506,
#4507),.UNSPECIFIED.,.F.,.F.,(4,3,3,3,3,3,3,3,3,3,3,3,3,3,3,3,3,3,3,3,3,
3,3,3,3,3,3,3,3,3,3,3,3,3,3,3,3,3,4),(24.2164788938612,24.3284578108245,
24.3365565142555,24.4485244285209,24.560294535519,24.6719543195167,24.7835468869861,
24.8951152477273,25.0067843218568,25.1185005830992,25.2304312375024,25.3303721529839,
25.4423485822127,25.5541272382699,25.6657955861649,25.7773967178561,25.8889736286533,
26.0006511630903,26.1123758489851,26.2243147601803,26.3241877917123,26.4361661670213,
26.5479468651215,26.6596173118309,26.7712205948806,26.8827997054225,26.9944794966149,
27.1062064741593,27.2181477050763,27.3180034304406,27.4292887012154,27.5403774827401,
27.651357678686,27.7622734955792,27.8731690428523,27.9841643917093,28.095212635599,
28.2064596772962,28.2743338817915),.UNSPECIFIED.);
#57=B_SPLINE_CURVE_WITH_KNOTS('',3,(#4513,#4514,#4515,#4516,#4517,#4518,
#4519,#4520,#4521,#4522,#4523,#4524,#4525,#4526,#4527,#4528,#4529,#4530,
#4531,#4532,#4533,#4534,#4535,#4536,#4537,#4538,#4539,#4540,#4541,#4542,
#4543,#4544,#4545,#4546,#4547,#4548,#4549,#4550,#4551,#4552,#4553,#4554,
#4555,#4556,#4557,#4558,#4559,#4560,#4561,#4562,#4563,#4564,#4565,#4566,
#4567,#4568,#4569,#4570,#4571,#4572,#4573),.UNSPECIFIED.,.F.,.F.,(4,3,3,
3,3,3,3,3,3,3,3,3,3,3,3,3,3,3,3,3,4),(15.707963267949,15.818355090934,15.9287111247549,
16.0430411946733,16.1535358156933,16.2697836100609,16.3860314044286,16.4981421037095,
16.6100544113457,16.7218559281154,16.8335894986427,16.9452978703484,17.0571042296374,
17.1689564942254,17.2810192004281,17.379847043157,17.4919974773912,17.6039638386448,
17.7158203932178,17.8276366370513,17.9335665904152),.UNSPECIFIED.);
#58=B_SPLINE_CURVE_WITH_KNOTS('',3,(#4575,#4576,#4577,#4578,#4579),
 .UNSPECIFIED.,.F.,.F.,(4,1,4),(14.3984001269719,15.3922157657002,15.7079548812379),
 .UNSPECIFIED.);
#59=B_SPLINE_CURVE_WITH_KNOTS('',3,(#4583,#4584,#4585,#4586,#4587,#4588,
#4589,#4590,#4591,#4592,#4593,#4594,#4595,#4596,#4597,#4598,#4599,#4600,
#4601,#4602,#4603,#4604,#4605,#4606,#4607,#4608,#4609,#4610,#4611,#4612,
#4613,#4614,#4615,#4616,#4617,#4618,#4619,#4620,#4621,#4622,#4623,#4624,
#4625,#4626,#4627,#4628,#4629,#4630,#4631,#4632,#4633,#4634),
 .UNSPECIFIED.,.F.,.F.,(4,3,3,3,3,3,3,3,3,3,3,3,3,3,3,3,3,4),(13.8759340267632,
13.9874055240017,14.0986819048936,14.2098503830277,14.3209548725418,14.4320391923179,
14.5432235672466,14.6544603986013,14.7658970889775,14.8368081797645,14.9473475531393,
15.0577376284281,15.1680237022244,15.2782509068263,15.3885311804989,15.4988322555113,
15.6093107358845,15.707963267949),.UNSPECIFIED.);
#60=B_SPLINE_CURVE_WITH_KNOTS('',3,(#4635,#4636,#4637,#4638,#4639,#4640,
#4641),.UNSPECIFIED.,.F.,.F.,(4,1,1,1,4),(15.707963267949,15.8306238184928,
16.8244394572212,17.8182550959496,17.9344079850994),.UNSPECIFIED.);
#61=B_SPLINE_CURVE_WITH_KNOTS('',3,(#4647,#4648,#4649,#4650,#4651,#4652,
#4653,#4654,#4655,#4656,#4657,#4658,#4659,#4660,#4661,#4662,#4663,#4664,
#4665,#4666,#4667,#4668,#4669,#4670,#4671,#4672,#4673,#4674,#4675,#4676,
#4677,#4678,#4679,#4680,#4681,#4682,#4683,#4684,#4685,#4686,#4687,#4688,
#4689,#4690,#4691,#4692,#4693,#4694,#4695,#4696,#4697,#4698),
 .UNSPECIFIED.,.F.,.F.,(4,3,3,3,3,3,3,3,3,3,3,3,3,3,3,3,3,4),(18.2326852175056,
18.3501141129404,18.4675228039056,18.5850446472557,18.7026282574228,18.8204305181141,
18.8824971358389,18.9989861703458,19.1152627236631,19.2314232752781,19.3475198007835,
19.4636041624104,19.5798208788147,19.6961099863659,19.8126414543351,19.8763127745673,
20.0320230471778,20.1591088879388),.UNSPECIFIED.);
#62=B_SPLINE_CURVE_WITH_KNOTS('',3,(#4700,#4701,#4702,#4703,#4704,#4705,
#4706,#4707,#4708,#4709,#4710,#4711,#4712,#4713),.UNSPECIFIED.,.F.,.F.,
(4,2,2,2,2,2,4),(-0.0902879860330804,-0.0695195013464431,-0.0576139772363393,
-0.0451609786697689,-0.0307684913612755,-0.00741601523602112,0.),
 .UNSPECIFIED.);
#63=B_SPLINE_CURVE_WITH_KNOTS('',3,(#4716,#4717,#4718,#4719,#4720,#4721,
#4722,#4723,#4724,#4725,#4726,#4727,#4728,#4729,#4730,#4731,#4732,#4733,
#4734,#4735,#4736,#4737,#4738,#4739,#4740,#4741,#4742,#4743,#4744,#4745,
#4746,#4747,#4748,#4749,#4750,#4751,#4752,#4753,#4754,#4755,#4756,#4757,
#4758,#4759,#4760,#4761,#4762,#4763,#4764,#4765,#4766,#4767,#4768,#4769,
#4770,#4771,#4772,#4773,#4774,#4775,#4776,#4777,#4778,#4779,#4780,#4781,
#4782,#4783,#4784,#4785,#4786,#4787,#4788,#4789,#4790,#4791,#4792,#4793,
#4794,#4795,#4796,#4797),.UNSPECIFIED.,.F.,.F.,(4,2,2,2,2,2,2,2,2,2,2,2,
2,2,2,2,2,2,2,2,2,2,2,2,2,2,2,2,2,2,2,2,2,2,2,2,2,2,2,2,4),(-1.10310963530152,
-1.09840428209197,-1.07722214007663,-1.06150851698653,-1.04868281780305,
-1.03819235320156,-1.02138418259208,-0.999282379625926,-0.990602595865436,
-0.983495936132868,-0.976570972649354,-0.961692691255592,-0.940952466821429,
-0.926313970937883,-0.916002211406824,-0.902436796120762,-0.870391217176744,
-0.860477072002617,-0.854465023776041,-0.845070439673182,-0.819245833374607,
-0.806702496780286,-0.79543475800065,-0.784817093076859,-0.762133674934839,
-0.745228751131369,-0.734731689538218,-0.728719271759347,-0.719808072857297,
-0.694096875566972,-0.681109182806924,-0.669588324732776,-0.658941721449021,
-0.638880453131988,-0.614447417440931,-0.606635107300723,-0.600344143431757,
-0.588300966408003,-0.564446554319691,-0.552834380572,-0.552725405623167),
 .UNSPECIFIED.);
#64=B_SPLINE_CURVE_WITH_KNOTS('',3,(#4803,#4804,#4805,#4806,#4807,#4808,
#4809,#4810,#4811,#4812,#4813,#4814,#4815,#4816,#4817,#4818,#4819,#4820,
#4821,#4822,#4823,#4824,#4825,#4826,#4827,#4828,#4829,#4830,#4831,#4832,
#4833,#4834,#4835,#4836,#4837,#4838,#4839,#4840,#4841,#4842,#4843,#4844,
#4845,#4846,#4847,#4848,#4849,#4850,#4851,#4852,#4853,#4854,#4855,#4856,
#4857),.UNSPECIFIED.,.F.,.F.,(4,3,3,3,3,3,3,3,3,3,3,3,3,3,3,3,3,3,4),(11.9491877790605,
12.0704897196116,12.1879350799606,12.3052738059049,12.4225558808697,12.539831191545,
12.6572286481437,12.7747004780911,12.892380281892,12.9196033034688,13.0391446098747,
13.1558912766851,13.2725228710644,13.3890907032798,13.5108014661389,13.6274735002162,
13.7442192750413,13.8611645569831,13.8759337547162),.UNSPECIFIED.);
#65=B_SPLINE_CURVE_WITH_KNOTS('',3,(#4858,#4859,#4860,#4861,#4862,#4863,
#4864,#4865,#4866,#4867,#4868,#4869,#4870,#4871,#4872,#4873,#4874,#4875,
#4876,#4877,#4878,#4879,#4880,#4881,#4882,#4883,#4884,#4885,#4886,#4887,
#4888,#4889,#4890,#4891,#4892,#4893,#4894,#4895,#4896,#4897,#4898,#4899,
#4900,#4901,#4902,#4903,#4904,#4905,#4906,#4907,#4908,#4909,#4910,#4911,
#4912,#4913,#4914,#4915,#4916,#4917,#4918,#4919,#4920,#4921,#4922,#4923,
#4924,#4925,#4926,#4927,#4928,#4929,#4930,#4931,#4932,#4933,#4934,#4935,
#4936,#4937,#4938,#4939,#4940,#4941,#4942,#4943,#4944,#4945,#4946,#4947,
#4948,#4949,#4950,#4951,#4952,#4953,#4954,#4955,#4956,#4957,#4958,#4959,
#4960,#4961,#4962,#4963,#4964,#4965,#4966,#4967,#4968,#4969,#4970,#4971,
#4972,#4973,#4974,#4975,#4976,#4977,#4978),.UNSPECIFIED.,.F.,.F.,(4,3,3,
3,3,3,3,3,3,3,3,3,3,3,3,3,3,3,3,3,3,3,3,3,3,3,3,3,3,3,3,3,3,3,3,3,3,3,3,
3,4),(13.8759337553363,13.9134189421971,14.0311296480262,14.1486252389434,
14.2660024664715,14.383311313252,14.5006016500783,14.6180056712398,14.735473475376,
14.8531565546079,14.9072345809255,15.0249483953848,15.1424479004606,15.2598295359287,
15.377143269917,15.4944389593616,15.6118489804661,15.7293231625642,15.8470131172698,
15.9010502196539,16.0185862160695,16.1359071716103,16.2531099559165,16.3702448724762,
16.4873621130608,16.604595636191,16.7218941812094,16.8394118468141,16.8948658583822,
17.0127678116824,17.1304532100569,17.2480191781504,17.365515344718,17.4829912252123,
17.6005766740717,17.7182237949846,17.8360809197351,17.8886814971106,18.006475161737,
18.1240829762214,18.2326852175056),.UNSPECIFIED.);
#66=B_SPLINE_CURVE_WITH_KNOTS('',3,(#4980,#4981,#4982,#4983,#4984,#4985,
#4986,#4987,#4988,#4989,#4990,#4991,#4992,#4993,#4994,#4995,#4996,#4997,
#4998,#4999,#5000,#5001,#5002,#5003,#5004,#5005,#5006,#5007,#5008,#5009,
#5010,#5011,#5012,#5013,#5014,#5015,#5016,#5017,#5018,#5019,#5020,#5021,
#5022,#5023,#5024,#5025,#5026,#5027,#5028,#5029,#5030,#5031,#5032,#5033,
#5034,#5035,#5036,#5037,#5038,#5039,#5040,#5041,#5042,#5043,#5044,#5045,
#5046,#5047,#5048,#5049,#5050,#5051,#5052,#5053,#5054,#5055,#5056,#5057,
#5058,#5059),.UNSPECIFIED.,.F.,.F.,(4,2,2,2,2,2,2,2,2,2,2,2,2,2,2,2,2,2,
2,2,2,2,2,2,2,2,2,2,2,2,2,2,2,2,2,2,2,2,2,4),(-0.552725405623167,-0.541977170966905,
-0.53084957666005,-0.51866977594079,-0.490571100145663,-0.481793473449696,
-0.475745498289177,-0.464874554957004,-0.446785851085663,-0.425816502562416,
-0.415167087894251,-0.403760289275286,-0.390983977795993,-0.365216310304077,
-0.356082527804832,-0.35005340954438,-0.33973200687133,-0.323398146844299,
-0.299824069413248,-0.289158384786419,-0.277737870662131,-0.264943180238732,
-0.233016973059306,-0.226580840545827,-0.219169303547567,-0.209851774465103,
-0.182807487580695,-0.169162145546328,-0.158906935173509,-0.144586539612125,
-0.124772548138701,-0.107597516249468,-0.10099011512184,-0.0938729126324881,
-0.0851219325742436,-0.0624426869455938,-0.0456861069530859,-0.0353317986472908,
-0.0229676387407706,-0.00036925595930691),.UNSPECIFIED.);
#67=B_SPLINE_CURVE_WITH_KNOTS('',3,(#5060,#5061,#5062,#5063,#5064,#5065,
#5066,#5067,#5068,#5069,#5070,#5071,#5072,#5073,#5074,#5075,#5076,#5077,
#5078,#5079,#5080,#5081,#5082,#5083,#5084,#5085,#5086,#5087,#5088,#5089,
#5090,#5091,#5092,#5093,#5094,#5095,#5096,#5097,#5098,#5099,#5100,#5101,
#5102,#5103,#5104,#5105,#5106,#5107,#5108,#5109,#5110,#5111,#5112,#5113,
#5114),.UNSPECIFIED.,.F.,.F.,(4,3,3,3,3,3,3,3,3,3,3,3,3,3,3,3,3,3,4),(-10.1357873115492,
-9.96754509954774,-9.93815638728366,-9.82046673168105,-9.70299196205392,
-9.58563539619237,-9.46834701434813,-9.35107690841475,-9.23369261088505,
-9.11624426811025,-8.99858002714185,-8.94434074855529,-8.82667899846583,
-8.7091951599211,-8.59183899812951,-8.47453671765872,-8.35726362182951,
-8.23992726492522,-8.20946475857041),.UNSPECIFIED.);
#68=B_SPLINE_CURVE_WITH_KNOTS('',3,(#5120,#5121,#5122,#5123,#5124,#5125,
#5126,#5127,#5128,#5129,#5130,#5131,#5132,#5133,#5134,#5135,#5136,#5137,
#5138,#5139,#5140,#5141,#5142,#5143,#5144,#5145,#5146,#5147,#5148,#5149,
#5150,#5151,#5152,#5153,#5154,#5155,#5156,#5157,#5158,#5159,#5160,#5161,
#5162,#5163,#5164,#5165,#5166,#5167,#5168,#5169,#5170,#5171),
 .UNSPECIFIED.,.F.,.F.,(4,3,3,3,3,3,3,3,3,3,3,3,3,3,3,3,3,4),(-1.9253726413955,
-1.80892801606211,-1.69271607294993,-1.57659231075127,-1.46050482883161,
-1.3438325313058,-1.22757869284794,-1.11069716578816,-0.993815638728368,
-0.869588683887322,-0.748964684319401,-0.628496931294659,-0.508144556691677,
-0.387866877787889,-0.267588204475049,-0.147310085942533,-0.0269467534811709,
0.),.UNSPECIFIED.);
#69=B_SPLINE_CURVE_WITH_KNOTS('',3,(#5174,#5175,#5176,#5177,#5178,#5179,
#5180,#5181,#5182,#5183,#5184,#5185,#5186,#5187,#5188,#5189,#5190,#5191,
#5192,#5193,#5194,#5195,#5196,#5197,#5198,#5199,#5200,#5201,#5202,#5203,
#5204,#5205,#5206,#5207,#5208,#5209,#5210,#5211,#5212,#5213,#5214,#5215,
#5216,#5217,#5218,#5219,#5220,#5221,#5222,#5223,#5224,#5225,#5226,#5227,
#5228,#5229,#5230,#5231,#5232,#5233,#5234,#5235,#5236,#5237,#5238,#5239,
#5240,#5241,#5242,#5243,#5244,#5245,#5246,#5247,#5248,#5249,#5250,#5251,
#5252,#5253,#5254,#5255,#5256,#5257,#5258,#5259,#5260,#5261,#5262,#5263,
#5264,#5265,#5266,#5267,#5268,#5269,#5270,#5271,#5272,#5273),
 .UNSPECIFIED.,.F.,.F.,(4,3,3,3,3,3,3,3,3,3,3,3,3,3,3,3,3,3,3,3,3,3,3,3,
3,3,3,3,3,3,3,3,3,4),(2.02058586035984,2.140693492338,2.25763871850387,
2.37446977250673,2.49123762200474,2.61378994554983,2.73066277291718,2.84760915246737,
2.96475566751446,2.9814469161851,3.09932762598598,3.21699987894726,3.33455773188,
3.45205079961854,3.56952859030924,3.68712343907614,3.8047842612984,3.9226614896851,
3.97526255491346,4.09280623566134,4.21013195125936,4.32733768164007,4.44447373540583,
4.56159030700783,4.67882045378987,4.79611407133702,4.91362448723962,4.96907819364183,
5.08676714789316,5.20427682387841,5.32166915676348,5.43898696672328,5.55634477834659,
5.66535571352405),.UNSPECIFIED.);
#70=B_SPLINE_CURVE_WITH_KNOTS('',3,(#5276,#5277,#5278,#5279,#5280,#5281,
#5282,#5283,#5284,#5285,#5286,#5287,#5288,#5289,#5290,#5291,#5292,#5293,
#5294,#5295,#5296,#5297,#5298,#5299,#5300,#5301,#5302,#5303,#5304,#5305,
#5306,#5307,#5308,#5309,#5310,#5311,#5312,#5313,#5314,#5315,#5316,#5317,
#5318,#5319,#5320,#5321,#5322,#5323,#5324,#5325,#5326,#5327,#5328,#5329,
#5330),.UNSPECIFIED.,.F.,.F.,(4,3,3,3,3,3,3,3,3,3,3,3,3,3,3,3,3,3,4),(5.66535571352405,
5.78282313787065,5.90050854996624,5.9628938323702,6.08060184387462,6.19809576663304,
6.31547196297819,6.43278041377381,6.55007098888068,6.66747619791458,6.78494573459987,
6.90263135953802,6.95670947109856,7.07492583639565,7.19294503118885,7.31080723912486,
7.42857851003219,7.54632867482091,7.59274844815668),.UNSPECIFIED.);
#71=B_SPLINE_CURVE_WITH_KNOTS('',3,(#5331,#5332,#5333,#5334,#5335,#5336,
#5337,#5338,#5339,#5340,#5341,#5342,#5343,#5344,#5345,#5346,#5347,#5348,
#5349,#5350,#5351,#5352,#5353,#5354,#5355,#5356,#5357,#5358,#5359,#5360,
#5361,#5362,#5363,#5364,#5365,#5366,#5367,#5368,#5369,#5370,#5371,#5372,
#5373,#5374,#5375,#5376,#5377,#5378,#5379,#5380,#5381,#5382,#5383,#5384,
#5385,#5386,#5387,#5388,#5389,#5390,#5391,#5392,#5393,#5394,#5395,#5396,
#5397,#5398,#5399,#5400,#5401,#5402,#5403,#5404,#5405,#5406,#5407,#5408,
#5409,#5410,#5411,#5412,#5413,#5414,#5415,#5416,#5417,#5418,#5419,#5420,
#5421,#5422,#5423,#5424,#5425,#5426,#5427,#5428,#5429,#5430,#5431,#5432,
#5433,#5434,#5435,#5436,#5437,#5438,#5439,#5440,#5441,#5442,#5443,#5444,
#5445,#5446,#5447,#5448,#5449,#5450,#5451),.UNSPECIFIED.,.F.,.F.,(4,3,3,
3,3,3,3,3,3,3,3,3,3,3,3,3,3,3,3,3,3,3,3,3,3,3,3,3,3,3,3,3,3,3,3,3,3,3,3,
3,4),(7.59274844890258,7.72609722425204,7.86061502881771,7.95052510982693,
8.06821691258659,8.18569390433419,8.30305273661296,8.42034342427409,8.53761587058653,
8.65500254100594,8.77245327853699,8.89011991932543,8.94434074855529,9.06203010323196,
9.17950469623869,9.29686116261319,9.41414952184228,9.53141968187335,9.64880414817428,
9.76625272552297,9.88391729904848,9.93815638728366,10.0558371193437,10.1733029282768,
10.2906505181704,10.4079299255747,10.5251910753747,10.6425665139707,10.760006040877,
10.8776616330052,10.931972026012,11.0496617074852,11.1671365028361,11.2844930943089,
11.4017815016062,11.5190516327888,11.636435955069,11.7538843223442,11.8715485871527,
11.9257876647404,11.9491877790605),.UNSPECIFIED.);
#72=B_SPLINE_CURVE_WITH_KNOTS('',3,(#5453,#5454,#5455,#5456,#5457,#5458,
#5459,#5460,#5461,#5462,#5463,#5464,#5465,#5466,#5467,#5468,#5469,#5470,
#5471,#5472,#5473,#5474,#5475,#5476,#5477,#5478,#5479,#5480,#5481,#5482,
#5483,#5484,#5485,#5486,#5487,#5488,#5489,#5490,#5491,#5492,#5493,#5494,
#5495,#5496,#5497,#5498,#5499,#5500,#5501,#5502,#5503,#5504,#5505,#5506,
#5507,#5508,#5509,#5510,#5511,#5512,#5513,#5514,#5515,#5516,#5517,#5518,
#5519,#5520,#5521,#5522,#5523,#5524,#5525,#5526,#5527,#5528,#5529,#5530,
#5531,#5532,#5533,#5534,#5535,#5536,#5537,#5538,#5539,#5540,#5541,#5542,
#5543,#5544,#5545,#5546,#5547,#5548,#5549,#5550,#5551,#5552,#5553,#5554,
#5555,#5556,#5557,#5558,#5559,#5560,#5561,#5562,#5563,#5564,#5565,#5566,
#5567,#5568,#5569,#5570,#5571,#5572,#5573),.UNSPECIFIED.,.F.,.F.,(4,3,3,
3,3,3,3,3,3,3,3,3,3,3,3,3,3,3,3,3,3,3,3,3,3,3,3,3,3,3,3,3,3,3,3,3,3,3,3,
3,4),(-8.20946475857041,-8.09199014784659,-7.97430853604256,-7.95052510982693,
-7.8328599850263,-7.7154097312376,-7.59807765075524,-7.48081367822952,-7.36356785992191,
-7.24620747770174,-7.12878287120506,-7.01114181960341,-6.95670947109856,
-6.83899885356979,-6.7215033492923,-6.60412620730503,-6.48681744482345,
-6.36952719090972,-6.25212324996335,-6.13465552461373,-6.01697252110421,
-5.9628938323702,-5.84518035750499,-5.7276811949198,-5.61029990342987,-5.49298651424117,
-5.37569116975381,-5.25828149111712,-5.1408076505398,-5.02311803196177,
-4.96907819364183,-4.85154138746856,-4.73421962199873,-4.6170160282861,
-4.49988030427019,-4.38276225960712,-4.26552794359781,-4.14822861091272,
-4.0307101746435,-3.97526255491346,-3.85260200436959),.UNSPECIFIED.);
#73=B_SPLINE_CURVE_WITH_KNOTS('',3,(#5574,#5575,#5576,#5577,#5578,#5579,
#5580,#5581,#5582,#5583,#5584,#5585,#5586,#5587,#5588,#5589,#5590,#5591,
#5592,#5593,#5594,#5595,#5596,#5597,#5598,#5599,#5600,#5601,#5602,#5603,
#5604,#5605,#5606,#5607,#5608,#5609,#5610,#5611,#5612,#5613,#5614,#5615,
#5616,#5617,#5618,#5619,#5620,#5621,#5622,#5623,#5624,#5625,#5626,#5627,
#5628),.UNSPECIFIED.,.F.,.F.,(4,3,3,3,3,3,3,3,3,3,3,3,3,3,3,3,3,3,4),(-3.85260200386407,
-3.73648747745417,-3.62051638895482,-3.50463624099859,-3.38879469763866,
-3.27286091253272,-3.15687669525244,-3.04068630600158,-2.9814469161851,
-2.86363061157218,-2.74602508039629,-2.62853533549447,-2.51111164876292,
-2.39370440056642,-2.27618134800846,-2.15859314055966,-2.04078899997219,
-1.98763127745673,-1.9253726413955),.UNSPECIFIED.);
#74=B_SPLINE_CURVE_WITH_KNOTS('',3,(#5631,#5632,#5633,#5634,#5635,#5636,
#5637,#5638),.UNSPECIFIED.,.F.,.F.,(4,1,1,1,1,4),(17.9344079850994,18.8120707346779,
19.8058863734063,20.7997020121347,21.793517650863,21.9911485751285),
 .UNSPECIFIED.);
#75=B_SPLINE_CURVE_WITH_KNOTS('',3,(#5639,#5640,#5641,#5642,#5643,#5644,
#5645,#5646,#5647,#5648,#5649,#5650,#5651,#5652,#5653,#5654,#5655,#5656,
#5657,#5658,#5659,#5660,#5661,#5662,#5663,#5664,#5665,#5666,#5667,#5668,
#5669,#5670,#5671,#5672,#5673,#5674,#5675,#5676,#5677,#5678,#5679,#5680,
#5681,#5682,#5683,#5684,#5685,#5686,#5687,#5688,#5689,#5690,#5691,#5692,
#5693,#5694,#5695,#5696,#5697,#5698,#5699,#5700,#5701,#5702),
 .UNSPECIFIED.,.F.,.F.,(4,3,3,3,3,3,3,3,3,3,3,3,3,3,3,3,3,3,3,3,3,4),(21.9911485751285,
22.1012980243391,22.2113482880773,22.321344734747,22.4313326401807,22.5414276972775,
22.6515882903729,22.7619346601458,22.7873332895914,22.8993096942055,23.0110883257836,
23.1227566492983,23.2343577567475,23.3459346434801,23.4576121543163,23.5693368168269,
23.6812757052973,23.7811489283198,23.8930884987303,24.0048748237804,24.1165488904639,
24.2171494664266),.UNSPECIFIED.);
#76=B_SPLINE_CURVE_WITH_KNOTS('',3,(#5704,#5705,#5706,#5707,#5708,#5709,
#5710,#5711,#5712,#5713,#5714,#5715,#5716,#5717,#5718,#5719,#5720,#5721,
#5722,#5723,#5724,#5725,#5726,#5727,#5728,#5729,#5730,#5731,#5732,#5733,
#5734,#5735,#5736,#5737,#5738,#5739,#5740,#5741,#5742,#5743,#5744,#5745,
#5746,#5747,#5748,#5749,#5750,#5751,#5752,#5753,#5754,#5755,#5756,#5757,
#5758,#5759,#5760,#5761,#5762,#5763,#5764),.UNSPECIFIED.,.F.,.F.,(4,3,3,
3,3,3,3,3,3,3,3,3,3,3,3,3,3,3,3,3,4),(21.9911485755794,22.1180239270845,
22.2459913725795,22.3489252367988,22.4609036843361,22.5726844279904,22.684354904006,
22.7959582001587,22.9075373076252,23.0192170705217,23.1309440058854,23.2428851718823,
23.3427408755272,23.4546781603108,23.5664579396098,23.6781234690952,23.7897178493381,
23.9013376620179,24.0129645371053,24.1247338172087,24.2164788938612),
 .UNSPECIFIED.);
#77=B_SPLINE_CURVE_WITH_KNOTS('',3,(#5765,#5766,#5767,#5768,#5769,#5770,
#5771,#5772,#5773,#5774,#5775,#5776,#5777,#5778,#5779,#5780,#5781,#5782,
#5783,#5784,#5785,#5786,#5787,#5788,#5789,#5790,#5791,#5792,#5793,#5794,
#5795,#5796,#5797,#5798,#5799,#5800,#5801,#5802,#5803,#5804,#5805,#5806,
#5807,#5808,#5809,#5810,#5811,#5812,#5813,#5814,#5815,#5816,#5817,#5818,
#5819,#5820,#5821,#5822,#5823,#5824,#5825,#5826,#5827,#5828,#5829,#5830,
#5831,#5832,#5833,#5834,#5835,#5836,#5837,#5838,#5839,#5840,#5841,#5842,
#5843,#5844,#5845,#5846,#5847,#5848,#5849,#5850,#5851,#5852,#5853,#5854,
#5855,#5856,#5857,#5858,#5859,#5860,#5861,#5862,#5863,#5864,#5865,#5866,
#5867,#5868,#5869,#5870,#5871,#5872,#5873,#5874,#5875,#5876),
 .UNSPECIFIED.,.F.,.F.,(4,3,3,3,3,3,3,3,3,3,3,3,3,3,3,3,3,3,3,3,3,3,3,3,
3,3,3,3,3,3,3,3,3,3,3,3,3,4),(17.9335665904152,18.0454424339238,18.1573652595226,
18.2695047672841,18.3736626818853,18.4855001980023,18.5971371009513,18.708662064031,
18.8201184282184,18.9315494357043,19.0430804470575,19.1546580302906,19.2664507586058,
19.3674783206137,19.4794788083052,19.5912816496511,19.7029742420256,19.8145996336116,
19.9262007760276,20.0379022986976,20.1496508775319,20.2616132084707,20.3612939593421,
20.4732878287697,20.5850846606291,20.6967716191335,20.8083917627454,20.9199880538123,
21.0316853912131,21.143430143744,21.2553893075683,21.3551095980704,21.467587143227,
21.5798851258176,21.6920363292369,21.8041004131203,21.9161448818857,21.9911485751285),
 .UNSPECIFIED.);
#78=B_SPLINE_CURVE_WITH_KNOTS('',3,(#5974,#5975,#5976,#5977,#5978,#5979,
#5980,#5981,#5982,#5983,#5984,#5985,#5986,#5987,#5988,#5989,#5990,#5991,
#5992,#5993,#5994,#5995,#5996,#5997,#5998,#5999,#6000,#6001,#6002,#6003,
#6004,#6005,#6006,#6007,#6008,#6009,#6010,#6011,#6012,#6013,#6014,#6015,
#6016,#6017,#6018,#6019,#6020,#6021,#6022,#6023,#6024,#6025,#6026,#6027,
#6028,#6029,#6030,#6031,#6032,#6033,#6034,#6035,#6036,#6037,#6038,#6039,
#6040,#6041,#6042,#6043,#6044,#6045,#6046,#6047,#6048,#6049,#6050,#6051,
#6052),.UNSPECIFIED.,.F.,.F.,(4,3,3,3,3,3,3,3,3,3,3,3,3,3,3,3,3,3,3,3,3,
3,3,3,3,3,4),(0.,0.0179048422970877,0.0361024915626215,0.0542404355784353,
0.0580134783300132,0.0611348681368874,0.0788899039747601,0.0963378629766525,
0.10916026369559,0.115724976061314,0.119100678912912,0.13593778804363,0.147800793130485,
0.16459229773457,0.169382843385744,0.173083715163794,0.189811925251359,
0.206538015292767,0.216907909431901,0.222250091057922,0.226942734525874,
0.243039503413473,0.25318826724009,0.25808162694784,0.273544260851943,0.28213282996317,
0.286347380332243),.UNSPECIFIED.);
#79=B_SPLINE_CURVE_WITH_KNOTS('',3,(#6053,#6054,#6055,#6056,#6057,#6058,
#6059,#6060,#6061,#6062,#6063,#6064,#6065,#6066,#6067,#6068,#6069,#6070,
#6071,#6072,#6073,#6074,#6075,#6076,#6077,#6078,#6079,#6080,#6081,#6082,
#6083,#6084,#6085,#6086,#6087,#6088,#6089,#6090,#6091,#6092,#6093,#6094,
#6095,#6096,#6097,#6098,#6099,#6100,#6101,#6102,#6103,#6104,#6105,#6106,
#6107,#6108,#6109,#6110,#6111,#6112,#6113,#6114,#6115,#6116,#6117,#6118,
#6119,#6120,#6121,#6122,#6123,#6124,#6125,#6126,#6127,#6128,#6129,#6130,
#6131,#6132,#6133,#6134),.UNSPECIFIED.,.F.,.F.,(4,3,3,3,3,3,3,3,3,3,3,3,
3,3,3,3,3,3,3,3,3,3,3,3,3,3,3,4),(1.07126707893266E-15,0.0152281422359197,
0.0310358564807719,0.0437698821708955,0.0495880457978997,0.0523050824654196,
0.0686461535426187,0.0852625440655788,0.0972830200437303,0.101409276797269,
0.104348930321076,0.121427316920974,0.133459759972985,0.150098458592417,
0.154673008198034,0.158573193033796,0.175469189003421,0.192923999237044,
0.203913467919425,0.209199575070649,0.212499609675233,0.215890121723282,
0.233888353561583,0.246488524940927,0.251400213167848,0.269588946346959,
0.280063647041007,0.285111243506067),.UNSPECIFIED.);
#80=B_SPLINE_CURVE_WITH_KNOTS('',3,(#6135,#6136,#6137,#6138),
 .UNSPECIFIED.,.F.,.F.,(4,4),(-0.0155829349012829,0.),.UNSPECIFIED.);
#81=B_SPLINE_CURVE_WITH_KNOTS('',3,(#6235,#6236,#6237,#6238,#6239,#6240,
#6241,#6242,#6243,#6244,#6245,#6246,#6247,#6248,#6249,#6250,#6251,#6252,
#6253,#6254,#6255,#6256,#6257,#6258,#6259,#6260,#6261,#6262,#6263,#6264,
#6265,#6266,#6267,#6268,#6269,#6270,#6271,#6272,#6273,#6274,#6275,#6276,
#6277,#6278,#6279,#6280,#6281,#6282,#6283,#6284,#6285,#6286,#6287,#6288,
#6289,#6290,#6291,#6292,#6293,#6294,#6295,#6296,#6297,#6298,#6299,#6300,
#6301,#6302,#6303,#6304,#6305,#6306,#6307,#6308,#6309,#6310,#6311,#6312,
#6313,#6314,#6315,#6316),.UNSPECIFIED.,.F.,.F.,(4,3,3,3,3,3,3,3,3,3,3,3,
3,3,3,3,3,3,3,3,3,3,3,3,3,3,3,4),(0.,0.0152282227773072,0.0310359955541488,
0.043770002841855,0.0495884887043898,0.053412115752948,0.0697756354439873,
0.0863907647498071,0.0972836205062952,0.101414423606461,0.104352797521847,
0.121431164597359,0.133459759972988,0.15009841762802,0.154672953836668,
0.158573187410825,0.175469130012791,0.192923920449733,0.203913403642419,
0.209199537217335,0.212499486961885,0.219647292536604,0.237645810922074,
0.246488478012031,0.251400187912865,0.269588921026693,0.280063647041022,
0.285128810487037),.UNSPECIFIED.);
#82=B_SPLINE_CURVE_WITH_KNOTS('',3,(#6317,#6318,#6319,#6320,#6321,#6322,
#6323,#6324,#6325,#6326,#6327,#6328,#6329,#6330,#6331,#6332,#6333,#6334,
#6335,#6336,#6337,#6338,#6339,#6340,#6341,#6342,#6343,#6344,#6345,#6346,
#6347,#6348,#6349,#6350,#6351,#6352,#6353,#6354,#6355,#6356,#6357,#6358,
#6359,#6360,#6361,#6362,#6363,#6364,#6365,#6366,#6367,#6368,#6369,#6370,
#6371,#6372,#6373,#6374,#6375,#6376,#6377,#6378,#6379,#6380,#6381,#6382,
#6383,#6384,#6385,#6386,#6387,#6388,#6389,#6390,#6391,#6392,#6393,#6394,
#6395),.UNSPECIFIED.,.F.,.F.,(4,3,3,3,3,3,3,3,3,3,3,3,3,3,3,3,3,3,3,3,3,
3,3,3,3,3,4),(0.,0.017904897346114,0.0361025664030719,0.0542404915517878,
0.0580134882355451,0.0611348756782414,0.0788871339356662,0.0973060528525341,
0.114370955860744,0.115724971769402,0.119100681284986,0.135937768656981,
0.147800793130486,0.164592297734572,0.169382837867022,0.173083711575593,
0.189811921998653,0.206538004930166,0.216907939748199,0.222250091872117,
0.226243992006493,0.242350705801912,0.25318821167206,0.258081617490871,
0.273544209260892,0.282132829963172,0.286347380332245),.UNSPECIFIED.);
#83=B_SPLINE_CURVE_WITH_KNOTS('',3,(#6490,#6491,#6492,#6493,#6494,#6495,
#6496,#6497,#6498,#6499,#6500,#6501,#6502,#6503,#6504,#6505,#6506,#6507,
#6508,#6509,#6510,#6511,#6512,#6513,#6514,#6515,#6516,#6517,#6518,#6519,
#6520,#6521,#6522,#6523,#6524,#6525,#6526,#6527,#6528,#6529,#6530,#6531,
#6532,#6533,#6534,#6535,#6536,#6537,#6538,#6539,#6540,#6541,#6542,#6543,
#6544,#6545,#6546,#6547,#6548,#6549,#6550,#6551,#6552,#6553,#6554,#6555,
#6556,#6557,#6558,#6559,#6560,#6561,#6562,#6563,#6564,#6565,#6566,#6567,
#6568,#6569,#6570,#6571,#6572,#6573,#6574,#6575,#6576,#6577,#6578,#6579,
#6580,#6581,#6582,#6583,#6584,#6585,#6586,#6587,#6588,#6589,#6590,#6591,
#6592,#6593),.UNSPECIFIED.,.F.,.F.,(4,2,2,2,2,2,2,2,2,2,2,2,2,2,2,2,2,2,
2,2,2,2,2,2,2,2,2,2,2,2,2,2,2,2,2,2,2,2,2,2,2,2,2,2,2,2,2,2,2,2,2,4),(-0.388514427190929,
-0.368221310937293,-0.346791783756936,-0.343842853532956,-0.342674543962951,
-0.341819510444399,-0.340868810709443,-0.339445697276287,-0.335398541529993,
-0.32895292619097,-0.314550516013459,-0.291050761397792,-0.286392135096329,
-0.284273066173644,-0.282636675189563,-0.28086450600946,-0.278021181417783,
-0.267979780725477,-0.234896592289182,-0.227511697807702,-0.225702799566772,
-0.22465610901148,-0.223829575858867,-0.222664975514512,-0.22025973306123,
-0.217050085148467,-0.208937459508696,-0.185148325978312,-0.171212712264527,
-0.167979267254765,-0.166089040079341,-0.164449928003969,-0.162431611861429,
-0.158497993283455,-0.136834284450073,-0.112966254746684,-0.109341869582915,
-0.107941242202741,-0.106991115318562,-0.106014115977095,-0.104509334881813,
-0.100096609042361,-0.0928656015424145,-0.0773124844305157,-0.0560252071051106,
-0.0528876958272259,-0.0508429216859864,-0.0491823720855215,-0.0472669220909674,
-0.0438997461789251,-0.0262185413838201,-0.00172224983852417),
 .UNSPECIFIED.);
#84=B_SPLINE_CURVE_WITH_KNOTS('',3,(#6596,#6597,#6598,#6599,#6600,#6601,
#6602,#6603,#6604,#6605,#6606,#6607,#6608,#6609,#6610,#6611,#6612,#6613,
#6614,#6615,#6616,#6617,#6618,#6619,#6620,#6621,#6622,#6623,#6624,#6625,
#6626,#6627,#6628,#6629,#6630,#6631,#6632,#6633,#6634,#6635,#6636,#6637,
#6638,#6639,#6640,#6641,#6642,#6643,#6644,#6645,#6646,#6647,#6648,#6649,
#6650),.UNSPECIFIED.,.F.,.F.,(4,3,3,3,3,3,3,3,3,3,3,3,3,3,3,3,3,3,4),(11.6159397475004,
11.7400323994672,11.862567028973,11.985074843802,12.1075982462362,12.2328689254857,
12.3556466736646,12.4821638184495,12.6086809632344,12.7327736152012,12.8511026178218,
12.9692968137257,13.0874111577251,13.2055004593513,13.323702607504,13.4419711806477,
13.560458265704,13.6014221789684,13.6623817597106),.UNSPECIFIED.);
#85=B_SPLINE_CURVE_WITH_KNOTS('',3,(#6655,#6656,#6657,#6658,#6659,#6660,
#6661,#6662,#6663,#6664,#6665,#6666,#6667,#6668,#6669,#6670,#6671,#6672,
#6673,#6674,#6675,#6676,#6677,#6678,#6679,#6680,#6681,#6682,#6683,#6684,
#6685,#6686,#6687,#6688,#6689,#6690,#6691,#6692,#6693,#6694,#6695,#6696,
#6697,#6698,#6699,#6700,#6701,#6702,#6703,#6704,#6705,#6706,#6707,#6708,
#6709,#6710,#6711,#6712,#6713,#6714,#6715,#6716,#6717,#6718,#6719,#6720,
#6721,#6722,#6723,#6724,#6725,#6726,#6727,#6728,#6729,#6730,#6731,#6732,
#6733,#6734,#6735,#6736,#6737,#6738,#6739,#6740,#6741,#6742,#6743,#6744,
#6745,#6746,#6747,#6748,#6749,#6750,#6751,#6752,#6753,#6754,#6755,#6756,
#6757,#6758,#6759,#6760,#6761,#6762,#6763,#6764,#6765,#6766,#6767,#6768,
#6769,#6770,#6771,#6772,#6773,#6774,#6775,#6776,#6777,#6778,#6779,#6780,
#6781,#6782,#6783,#6784,#6785,#6786,#6787,#6788,#6789,#6790,#6791,#6792,
#6793,#6794,#6795,#6796,#6797,#6798,#6799,#6800,#6801,#6802,#6803,#6804,
#6805,#6806,#6807,#6808,#6809,#6810,#6811,#6812,#6813,#6814,#6815,#6816,
#6817,#6818,#6819,#6820,#6821,#6822,#6823,#6824,#6825,#6826,#6827,#6828,
#6829,#6830,#6831,#6832,#6833,#6834,#6835,#6836,#6837,#6838,#6839,#6840,
#6841,#6842,#6843,#6844,#6845,#6846,#6847,#6848,#6849,#6850,#6851,#6852,
#6853,#6854,#6855,#6856,#6857,#6858,#6859,#6860,#6861,#6862,#6863,#6864,
#6865,#6866,#6867,#6868,#6869,#6870,#6871,#6872,#6873,#6874),
 .UNSPECIFIED.,.F.,.F.,(4,2,2,2,2,2,2,2,2,2,2,2,2,2,2,2,2,2,2,2,2,2,2,2,
2,2,2,2,2,2,2,2,2,2,2,2,2,2,2,2,2,2,2,2,2,2,2,2,2,2,2,2,2,2,2,2,2,2,2,2,
2,2,2,2,2,2,2,2,2,2,2,2,2,2,2,2,2,2,2,2,2,2,2,2,2,2,2,2,2,2,2,2,2,2,2,2,
2,2,2,2,2,2,2,2,2,2,2,2,2,4),(-1.13034213650894,-1.11820041556272,-1.11177497333452,
-1.10702526459189,-1.10485747823376,-1.10320963951788,-1.10142274079296,
-1.09855015211907,-1.08933196811893,-1.05797328810593,-1.05142615478228,
-1.04732838922035,-1.04589136802156,-1.0449329513895,-1.04407836063236,
-1.04291101850557,-1.03996504071417,-1.01856767427725,-1.00089023061501,
-0.99451631738985,-0.989795890656017,-0.987633536452375,-0.985986620994032,
-0.98419760350581,-0.981314703344727,-0.971997099803371,-0.947031836916508,
-0.931352399734769,-0.929260956228999,-0.92816043504425,-0.92724610555965,
-0.926096197724991,-0.9242738535319,-0.913860420219523,-0.905378302347292,
-0.890964824454125,-0.874929853182554,-0.871673834827296,-0.869803389415422,
-0.868171797855497,-0.86615043382999,-0.863027939613639,-0.840359212284697,
-0.823002803884699,-0.816814311731417,-0.812878535714292,-0.811463204754879,
-0.810509129265617,-0.809649936427881,-0.808466211197927,-0.805458770482397,
-0.786547298096331,-0.76780885711994,-0.757118941048501,-0.754204369043874,
-0.752407656370931,-0.750761548758316,-0.748647663602783,-0.744071461326168,
-0.718193708769564,-0.703313973227802,-0.69863965860383,-0.695437100124942,
-0.694131129064522,-0.693198150743625,-0.692315151393086,-0.690773485775082,
-0.686249583783698,-0.678509337501351,-0.662821909200767,-0.640915208090116,
-0.637783632906045,-0.63576056827369,-0.634130361513526,-0.632264549260561,
-0.629024566980841,-0.613288092327909,-0.590011639141079,-0.5796148181095,
-0.577793949130371,-0.576644953121554,-0.575731081854003,-0.57463079288496,
-0.572540081175855,-0.556898177806101,-0.532038487071388,-0.52257177098094,
-0.519669399877649,-0.517875386921876,-0.516228573833571,-0.5140731795945,
-0.509395587447883,-0.503096525912975,-0.485779367623905,-0.463858351648118,
-0.460944071181973,-0.459775085167193,-0.458918891001253,-0.457955454832381,
-0.456509464126,-0.452374802532125,-0.445751668633164,-0.412950832225143,
-0.405181758156097,-0.402475709624456,-0.400721473034683,-0.399053286009071,
-0.396780642755917,-0.391448996417024,-0.388514427190929),.UNSPECIFIED.);
#86=B_SPLINE_CURVE_WITH_KNOTS('',3,(#6876,#6877,#6878,#6879,#6880,#6881,
#6882,#6883,#6884,#6885,#6886,#6887,#6888,#6889,#6890,#6891,#6892,#6893,
#6894,#6895,#6896,#6897,#6898,#6899,#6900,#6901,#6902,#6903,#6904,#6905,
#6906,#6907,#6908,#6909,#6910,#6911,#6912,#6913,#6914,#6915,#6916,#6917,
#6918,#6919,#6920,#6921,#6922,#6923,#6924,#6925,#6926,#6927,#6928,#6929,
#6930),.UNSPECIFIED.,.F.,.F.,(4,3,3,3,3,3,3,3,3,3,3,3,3,3,3,3,3,3,4),(13.6623817597106,
13.7822439330251,13.9019593887874,14.0215805270642,14.141159596228,14.2608366137815,
14.380560216883,14.5005136928787,14.5941633947024,14.7182560466692,14.838053126636,
14.9577353493353,15.0773549872691,15.1969642038554,15.3166972037048,15.4365049949453,
15.5565283172486,15.5869046104364,15.7079632679489),.UNSPECIFIED.);
#87=B_SPLINE_CURVE_WITH_KNOTS('',3,(#6931,#6932,#6933,#6934,#6935,#6936,
#6937,#6938,#6939,#6940,#6941,#6942,#6943,#6944,#6945,#6946,#6947,#6948,
#6949,#6950,#6951,#6952,#6953,#6954,#6955,#6956,#6957,#6958,#6959,#6960,
#6961,#6962,#6963,#6964,#6965,#6966,#6967,#6968,#6969,#6970,#6971,#6972,
#6973,#6974,#6975,#6976,#6977,#6978,#6979,#6980,#6981,#6982,#6983,#6984,
#6985,#6986,#6987,#6988,#6989,#6990,#6991,#6992,#6993,#6994,#6995,#6996,
#6997,#6998,#6999,#7000,#7001,#7002,#7003,#7004,#7005,#7006,#7007,#7008,
#7009,#7010,#7011,#7012,#7013,#7014,#7015,#7016,#7017,#7018,#7019,#7020,
#7021,#7022,#7023,#7024,#7025,#7026,#7027,#7028,#7029,#7030,#7031,#7032,
#7033,#7034,#7035,#7036,#7037,#7038,#7039,#7040,#7041,#7042,#7043,#7044,
#7045,#7046,#7047,#7048,#7049,#7050,#7051,#7052,#7053,#7054,#7055,#7056,
#7057,#7058,#7059,#7060,#7061,#7062,#7063,#7064,#7065,#7066,#7067,#7068,
#7069,#7070,#7071,#7072,#7073,#7074,#7075,#7076,#7077,#7078),
 .UNSPECIFIED.,.F.,.F.,(4,2,2,2,2,2,2,2,2,2,2,2,2,2,2,2,2,2,2,2,2,2,2,2,
2,2,2,2,2,2,2,2,2,2,2,2,2,2,2,2,2,2,2,2,2,2,2,2,2,2,2,2,2,2,2,2,2,2,2,2,
2,2,2,2,2,2,2,2,2,2,2,2,2,4),(-1.4842126102915,-1.45130207338096,-1.44653130870228,
-1.44276869942762,-1.44080057054265,-1.43934051164438,-1.43751243817818,
-1.4344104257189,-1.42265854661368,-1.39703504888428,-1.38855781433865,
-1.38526210078702,-1.38285473389067,-1.38168740855745,-1.38078564426567,
-1.37972798915731,-1.37788809376559,-1.37017195385148,-1.36675056177856,
-1.3445160894195,-1.32824044125102,-1.32496817415823,-1.32309142791469,
-1.3214560273151,-1.31943202057342,-1.31630906073201,-1.29380089136102,
-1.27658693263777,-1.27035072447172,-1.26639114431749,-1.26496911456164,
-1.26401104340175,-1.26315131940477,-1.26196698062992,-1.2589596710476,
-1.24090131187391,-1.22086735295395,-1.21057179383267,-1.2076926130244,
-1.20590414969959,-1.20425655965863,-1.20212813564549,-1.19746864097054,
-1.17384809453591,-1.16461532130469,-1.15161192875772,-1.14877183895778,
-1.14752773246244,-1.14660501956323,-1.14556920533366,-1.14377563658134,
-1.1369004973678,-1.13034372480405,-1.12505514274365,-1.1113946695191,-1.0999270589011,
-1.09505136269905,-1.09121913384257,-1.08922918810993,-1.0877587552546,
-1.08592503317702,-1.08283083981542,-1.0712707980281,-1.04563535180211,
-1.03715357075267,-1.03224704240593,-1.03071241032682,-1.02973378947652,
-1.02879532618135,-1.02763142312175,-1.024737534062,-1.00239397536905,-0.985353888275223,
-0.983952824113294),.UNSPECIFIED.);
#88=B_SPLINE_CURVE_WITH_KNOTS('',3,(#7084,#7085,#7086,#7087,#7088,#7089,
#7090,#7091,#7092,#7093,#7094,#7095,#7096,#7097,#7098,#7099,#7100,#7101,
#7102,#7103,#7104,#7105,#7106,#7107,#7108,#7109,#7110,#7111,#7112,#7113,
#7114,#7115,#7116,#7117,#7118,#7119,#7120,#7121,#7122,#7123,#7124,#7125,
#7126,#7127,#7128,#7129,#7130,#7131,#7132,#7133,#7134,#7135,#7136,#7137,
#7138,#7139,#7140,#7141,#7142,#7143,#7144,#7145,#7146,#7147,#7148,#7149,
#7150,#7151,#7152,#7153,#7154,#7155,#7156,#7157,#7158,#7159,#7160,#7161,
#7162,#7163,#7164,#7165,#7166,#7167,#7168,#7169,#7170,#7171,#7172,#7173,
#7174,#7175,#7176,#7177,#7178,#7179,#7180,#7181,#7182,#7183,#7184,#7185,
#7186,#7187,#7188,#7189,#7190,#7191,#7192,#7193,#7194,#7195,#7196,#7197,
#7198,#7199,#7200,#7201,#7202,#7203,#7204,#7205,#7206,#7207,#7208,#7209,
#7210,#7211,#7212,#7213,#7214,#7215,#7216,#7217,#7218,#7219,#7220,#7221,
#7222,#7223,#7224,#7225,#7226,#7227,#7228,#7229,#7230,#7231,#7232,#7233,
#7234,#7235,#7236,#7237,#7238,#7239,#7240,#7241),.UNSPECIFIED.,.F.,.F.,
(4,2,2,2,2,2,2,2,2,2,2,2,2,2,2,2,2,2,2,2,2,2,2,2,2,2,2,2,2,2,2,2,2,2,2,
2,2,2,2,2,2,2,2,2,2,2,2,2,2,2,2,2,2,2,2,2,2,2,2,2,2,2,2,2,2,2,2,2,2,2,2,
2,2,2,2,2,2,2,4),(-0.50063650275462,-0.497024637327494,-0.495221469099781,
-0.494172101298276,-0.493343476842378,-0.492172717878405,-0.489733842655887,
-0.48646488791054,-0.478116602320491,-0.453224652532998,-0.440866015760715,
-0.437708521725177,-0.43585911919942,-0.434388009039503,-0.432412512068425,
-0.428660542059646,-0.423915850114574,-0.412918930263119,-0.390000903402408,
-0.380088751451523,-0.378118092411696,-0.377030712610813,-0.37611507727911,
-0.374947899808193,-0.372527524358872,-0.369290559832854,-0.361065820328322,
-0.336791511166343,-0.323720090478632,-0.320552077568326,-0.318682313840578,
-0.317050171360907,-0.315026639774005,-0.311037965859611,-0.305908604171269,
-0.293519775473539,-0.275504200391794,-0.263046350866745,-0.261149301146257,
-0.259976754628464,-0.259060776951206,-0.257977550615054,-0.255969559166934,
-0.243626994095386,-0.218649328115914,-0.20638912865002,-0.203238106878432,
-0.201390134617007,-0.199918875936053,-0.197941519525203,-0.194180385200166,
-0.189420928527075,-0.178372117169142,-0.15215115604119,-0.145266667814842,
-0.143470367067601,-0.142432885763339,-0.141508973714647,-0.14030975903304,
-0.137650977813546,-0.133944521184283,-0.123810489935291,-0.09795895259853,
-0.0886339571623371,-0.0857493870782382,-0.0839594152448264,-0.0823116697759282,
-0.080148292349025,-0.0757326145299565,-0.0592212029193365,-0.0449233210994165,
-0.0286365008532833,-0.0267014876391612,-0.0255176528208188,-0.0246007846056997,
-0.0235257826118716,-0.0223781926196326,-0.0205714060941184,-0.000340550666543722),
 .UNSPECIFIED.);
#89=B_SPLINE_CURVE_WITH_KNOTS('',3,(#7242,#7243,#7244,#7245,#7246,#7247,
#7248,#7249,#7250,#7251,#7252,#7253,#7254,#7255,#7256,#7257,#7258,#7259,
#7260,#7261,#7262,#7263,#7264,#7265,#7266,#7267,#7268,#7269,#7270,#7271,
#7272,#7273,#7274,#7275,#7276,#7277,#7278,#7279,#7280,#7281,#7282,#7283,
#7284,#7285,#7286,#7287,#7288,#7289,#7290,#7291,#7292,#7293,#7294,#7295,
#7296,#7297,#7298,#7299,#7300,#7301,#7302,#7303,#7304,#7305,#7306,#7307,
#7308,#7309,#7310,#7311,#7312,#7313),.UNSPECIFIED.,.F.,.F.,(4,2,2,2,2,2,
2,2,2,2,2,2,2,2,2,2,2,2,2,2,2,2,2,2,2,2,2,2,2,2,2,2,2,2,2,4),(-1.37194901085214,
-1.34536824511777,-1.34239661910496,-1.34044614178634,-1.33857827078369,
-1.33694682595166,-1.33492292119506,-1.33179126924952,-1.31125702746167,
-1.29365158861557,-1.28627394289529,-1.28185440494781,-1.28040102360935,
-1.279419129298,-1.27848200570107,-1.27732337203004,-1.27446076747013,-1.25172253860903,
-1.23493567505875,-1.22564933688806,-1.22293752234361,-1.22114898911913,
-1.21950187176284,-1.21737481149489,-1.21272137552847,-1.18903102983852,
-1.17492030217937,-1.16853475121453,-1.16450967889086,-1.16308248541461,
-1.16212619743274,-1.1612698733031,-1.16009582551167,-1.15714334193878,
-1.13613143610354,-1.13034213650894),.UNSPECIFIED.);
#90=B_SPLINE_CURVE_WITH_KNOTS('',3,(#7314,#7315,#7316,#7317,#7318,#7319,
#7320,#7321,#7322,#7323,#7324,#7325,#7326,#7327,#7328,#7329,#7330,#7331,
#7332,#7333,#7334,#7335,#7336,#7337,#7338,#7339,#7340,#7341,#7342,#7343,
#7344,#7345,#7346,#7347,#7348,#7349,#7350,#7351,#7352,#7353,#7354,#7355,
#7356,#7357,#7358,#7359,#7360,#7361,#7362,#7363,#7364,#7365,#7366,#7367,
#7368,#7369,#7370,#7371,#7372,#7373,#7374,#7375,#7376,#7377,#7378,#7379,
#7380,#7381,#7382,#7383,#7384,#7385,#7386,#7387,#7388,#7389,#7390,#7391,
#7392,#7393,#7394,#7395,#7396,#7397,#7398,#7399,#7400,#7401,#7402,#7403,
#7404,#7405,#7406,#7407,#7408,#7409,#7410,#7411,#7412,#7413,#7414,#7415,
#7416,#7417,#7418,#7419,#7420,#7421,#7422,#7423,#7424,#7425,#7426,#7427,
#7428,#7429,#7430,#7431,#7432,#7433,#7434,#7435,#7436,#7437,#7438,#7439,
#7440,#7441,#7442,#7443,#7444,#7445,#7446,#7447,#7448,#7449,#7450,#7451,
#7452,#7453,#7454,#7455,#7456,#7457,#7458,#7459,#7460,#7461,#7462,#7463,
#7464,#7465,#7466,#7467,#7468,#7469,#7470,#7471,#7472,#7473,#7474,#7475,
#7476,#7477,#7478,#7479,#7480,#7481,#7482,#7483,#7484,#7485,#7486,#7487,
#7488,#7489,#7490,#7491,#7492,#7493,#7494,#7495,#7496,#7497,#7498,#7499,
#7500,#7501,#7502,#7503,#7504,#7505,#7506,#7507,#7508,#7509,#7510,#7511,
#7512,#7513,#7514,#7515,#7516,#7517,#7518,#7519,#7520,#7521,#7522,#7523,
#7524,#7525),.UNSPECIFIED.,.F.,.F.,(4,2,2,2,2,2,2,2,2,2,2,2,2,2,2,2,2,2,
2,2,2,2,2,2,2,2,2,2,2,2,2,2,2,2,2,2,2,2,2,2,2,2,2,2,2,2,2,2,2,2,2,2,2,2,
2,2,2,2,2,2,2,2,2,2,2,2,2,2,2,2,2,2,2,2,2,2,2,2,2,2,2,2,2,2,2,2,2,2,2,2,
2,2,2,2,2,2,2,2,2,2,2,2,2,2,2,4),(-0.983952824113294,-0.979112457342209,
-0.974467210153396,-0.972318108599363,-0.970672559708975,-0.968876428169694,
-0.965962748639736,-0.956367956378335,-0.925454067561909,-0.918936148615411,
-0.914851190701928,-0.9134154210932,-0.912456926202318,-0.911601816724087,
-0.910432824749628,-0.907510684142617,-0.885735684430236,-0.868321864233186,
-0.86200269440527,-0.857313497744151,-0.855156830607735,-0.85351072917423,
-0.851719152654242,-0.848824455782848,-0.839402772390256,-0.814521718062078,
-0.798874004326344,-0.796783280196324,-0.79568299312694,-0.794768810212375,
-0.793619032069579,-0.79179674190767,-0.781378236929632,-0.772879384216026,
-0.758416439463654,-0.742455947614859,-0.739242432341524,-0.737362976429339,
-0.735732756192979,-0.733724939901887,-0.729811076664254,-0.710344793261954,
-0.690555130412554,-0.681441642654773,-0.679514134972561,-0.678436812333014,
-0.677520688410213,-0.676341400787479,-0.673856830254932,-0.657571990761665,
-0.629363875052377,-0.6235329308949,-0.621118517170292,-0.619596915814238,
-0.617917721693957,-0.615563096914216,-0.609697241792277,-0.576305668323957,
-0.56441144503393,-0.562535875829102,-0.561369872435618,-0.560454549203759,
-0.559366831544476,-0.557336714035062,-0.544267051131203,-0.514184662095057,
-0.506800394592969,-0.504150088099636,-0.502584971541169,-0.500936077963987,
-0.498760679712532,-0.493968522749452,-0.487467358485707,-0.456539253956947,
-0.446978560843,-0.445026777089898,-0.443943845995054,-0.443028155468029,
-0.441856051730323,-0.439409069944889,-0.419040355454601,-0.392865542696693,
-0.388307656442141,-0.386197810391775,-0.38455302103317,-0.382755916582182,
-0.379836636757588,-0.369081443983243,-0.350140703300661,-0.346589037711122,
-0.330038268487219,-0.328103777119719,-0.326920315779717,-0.326003760019795,
-0.324929152495716,-0.322960633236989,-0.311703117048912,-0.295885020599676,
-0.2739338284628,-0.270791465048754,-0.268764127147645,-0.26713218555787,
-0.265266227696324,-0.26203065701868,-0.246426662707309,-0.242036404917214),
 .UNSPECIFIED.);
#91=B_SPLINE_CURVE_WITH_KNOTS('',3,(#7530,#7531,#7532,#7533,#7534,#7535,
#7536,#7537,#7538,#7539,#7540,#7541,#7542,#7543,#7544,#7545,#7546,#7547,
#7548,#7549,#7550,#7551,#7552,#7553,#7554,#7555,#7556,#7557,#7558,#7559,
#7560,#7561,#7562,#7563,#7564,#7565,#7566,#7567,#7568,#7569,#7570,#7571,
#7572,#7573,#7574,#7575,#7576,#7577,#7578,#7579,#7580,#7581,#7582,#7583,
#7584,#7585,#7586,#7587,#7588,#7589,#7590,#7591,#7592,#7593,#7594,#7595,
#7596,#7597,#7598,#7599,#7600,#7601,#7602,#7603,#7604,#7605,#7606,#7607,
#7608,#7609,#7610,#7611,#7612,#7613,#7614,#7615,#7616,#7617,#7618,#7619,
#7620,#7621,#7622,#7623,#7624,#7625,#7626,#7627,#7628,#7629,#7630,#7631,
#7632,#7633,#7634,#7635,#7636,#7637,#7638,#7639,#7640,#7641,#7642,#7643,
#7644,#7645,#7646,#7647,#7648,#7649,#7650,#7651,#7652,#7653,#7654,#7655,
#7656,#7657,#7658,#7659,#7660,#7661,#7662,#7663,#7664,#7665,#7666,#7667,
#7668,#7669,#7670,#7671,#7672,#7673,#7674,#7675,#7676,#7677,#7678,#7679,
#7680,#7681,#7682,#7683,#7684,#7685,#7686,#7687,#7688,#7689,#7690,#7691,
#7692,#7693,#7694,#7695,#7696,#7697,#7698,#7699,#7700,#7701,#7702,#7703,
#7704,#7705,#7706,#7707,#7708,#7709,#7710,#7711,#7712,#7713,#7714,#7715,
#7716,#7717,#7718,#7719,#7720,#7721,#7722,#7723,#7724,#7725,#7726,#7727,
#7728,#7729,#7730,#7731,#7732,#7733,#7734,#7735,#7736,#7737,#7738,#7739,
#7740,#7741,#7742,#7743,#7744,#7745,#7746,#7747),.UNSPECIFIED.,.F.,.F.,
(4,2,2,2,2,2,2,2,2,2,2,2,2,2,2,2,2,2,2,2,2,2,2,2,2,2,2,2,2,2,2,2,2,2,2,
2,2,2,2,2,2,2,2,2,2,2,2,2,2,2,2,2,2,2,2,2,2,2,2,2,2,2,2,2,2,2,2,2,2,2,2,
2,2,2,2,2,2,2,2,2,2,2,2,2,2,2,2,2,2,2,2,2,2,2,2,2,2,2,2,2,2,2,2,2,2,2,2,
2,4),(-1.24264336813119,-1.22712387526997,-1.20979043909343,-1.20357483124483,
-1.19962660535392,-1.19820958233988,-1.1972552015808,-1.19639682159987,
-1.19521511959944,-1.19221789981971,-1.17284850970692,-1.15440534164446,
-1.14380788165375,-1.14090173994353,-1.13910723124616,-1.13746117927735,
-1.13534465337651,-1.13075179952556,-1.10523906071215,-1.09828730208679,
-1.08489208712552,-1.082010351588,-1.08075827738038,-1.07983359958038,-1.07879956122474,
-1.07701855233006,-1.07030705950698,-1.06487313487277,-1.05809892239603,
-1.03713163172408,-1.0301386978465,-1.02507180193962,-1.0228476100675,-1.0211908289725,
-1.01963932991833,-1.01706257980809,-1.0102055054726,-0.979647202704972,
-0.970596590982185,-0.967150237728209,-0.964609930994401,-0.963419792553165,
-0.962502395743958,-0.961431833346224,-0.959535718783307,-0.950962199086458,
-0.919101737246764,-0.912525607385185,-0.907690497674577,-0.905507030483104,
-0.90385655098092,-0.902075736918723,-0.899232529315944,-0.890304074065052,
-0.864995358738982,-0.849182001509665,-0.847087495813602,-0.845986080348796,
-0.845071433052295,-0.843921636805775,-0.842100360838026,-0.831724092395496,
-0.829243987775399,-0.823742451505518,-0.809999637397287,-0.798595745451111,
-0.793735794587718,-0.789912071538546,-0.787921891398305,-0.786291819411394,
-0.784396573813481,-0.781116074382432,-0.766029631183796,-0.742162358302822,
-0.731835197619737,-0.730015707904923,-0.72886641777491,-0.727951734275185,
-0.726849742074642,-0.724752694641456,-0.708790487399557,-0.683089422239272,
-0.674617375026131,-0.671828296225942,-0.670059129977536,-0.668404071696104,
-0.666191366279745,-0.661191239826731,-0.654318641261029,-0.634045211892259,
-0.631755811411363,-0.614811879826588,-0.612876358682872,-0.611692393317409,
-0.610775533046097,-0.609700661792849,-0.607731841359522,-0.596477892339598,
-0.580653748784753,-0.558696996926903,-0.555554343478411,-0.553526596051362,
-0.551894177024496,-0.550027508688503,-0.546790271736406,-0.531166267807641,
-0.508897535085186,-0.504245027562709,-0.50063650275462),.UNSPECIFIED.);
#92=B_SPLINE_CURVE_WITH_KNOTS('',3,(#7749,#7750,#7751,#7752,#7753,#7754,
#7755,#7756,#7757,#7758,#7759,#7760,#7761,#7762,#7763,#7764,#7765,#7766,
#7767,#7768,#7769,#7770,#7771,#7772,#7773,#7774,#7775,#7776,#7777,#7778,
#7779,#7780,#7781,#7782,#7783,#7784,#7785,#7786,#7787,#7788,#7789,#7790,
#7791,#7792,#7793,#7794,#7795,#7796,#7797,#7798,#7799,#7800,#7801,#7802,
#7803,#7804,#7805,#7806,#7807,#7808,#7809,#7810,#7811,#7812,#7813,#7814,
#7815,#7816,#7817,#7818,#7819,#7820),.UNSPECIFIED.,.F.,.F.,(4,2,2,2,2,2,
2,2,2,2,2,2,2,2,2,2,2,2,2,2,2,2,2,2,2,2,2,2,2,2,2,2,2,2,2,4),(-0.242036404917214,
-0.224304689154436,-0.219081814344386,-0.212217338264901,-0.210423145404613,
-0.209386338842877,-0.208462666703193,-0.207216708244654,-0.204369011382599,
-0.191299921640434,-0.173017733276505,-0.156535286804907,-0.153193752754875,
-0.151285062299865,-0.149671724073372,-0.147705565778639,-0.144195939889097,
-0.139707951364804,-0.129590328758661,-0.10074616488669,-0.0948246251316918,
-0.0931187066129743,-0.0921012994788982,-0.0911712853451696,-0.0902432979436676,
-0.0880087333420003,-0.0730617412361167,-0.0581265465350124,-0.0394301049462768,
-0.0363181880100623,-0.0342999386601178,-0.0326684507778004,-0.0307954762365262,
-0.0288378594984424,-0.0258493948732865,-0.000340914984294712),
 .UNSPECIFIED.);
#93=B_SPLINE_CURVE_WITH_KNOTS('',3,(#7821,#7822,#7823,#7824,#7825,#7826,
#7827,#7828,#7829,#7830,#7831,#7832,#7833,#7834,#7835,#7836,#7837,#7838,
#7839,#7840,#7841,#7842,#7843,#7844,#7845,#7846,#7847,#7848,#7849,#7850,
#7851,#7852,#7853,#7854,#7855,#7856,#7857,#7858,#7859,#7860,#7861,#7862,
#7863,#7864,#7865,#7866,#7867,#7868,#7869,#7870,#7871,#7872,#7873,#7874,
#7875,#7876,#7877,#7878,#7879,#7880,#7881,#7882,#7883,#7884,#7885,#7886,
#7887,#7888,#7889,#7890,#7891,#7892,#7893,#7894,#7895,#7896,#7897,#7898,
#7899,#7900,#7901,#7902,#7903,#7904,#7905,#7906,#7907,#7908,#7909,#7910,
#7911,#7912,#7913,#7914,#7915,#7916,#7917,#7918,#7919,#7920,#7921,#7922,
#7923,#7924,#7925,#7926,#7927,#7928,#7929,#7930,#7931,#7932,#7933,#7934,
#7935,#7936,#7937,#7938,#7939,#7940,#7941,#7942,#7943,#7944,#7945,#7946,
#7947,#7948,#7949,#7950,#7951,#7952,#7953,#7954,#7955,#7956,#7957,#7958,
#7959,#7960,#7961,#7962,#7963,#7964,#7965,#7966,#7967,#7968,#7969,#7970,
#7971,#7972),.UNSPECIFIED.,.F.,.F.,(4,2,2,2,2,2,2,2,2,2,2,2,2,2,2,2,2,2,
2,2,2,2,2,2,2,2,2,2,2,2,2,2,2,2,2,2,2,2,2,2,2,2,2,2,2,2,2,2,2,2,2,2,2,2,
2,2,2,2,2,2,2,2,2,2,2,2,2,2,2,2,2,2,2,2,2,4),(-1.48452552344657,-1.46324998878013,
-1.46143255545788,-1.46028067119404,-1.45920273036994,-1.45828632138,-1.4571069253181,
-1.45518665640661,-1.43747892874884,-1.4195484851468,-1.40579231336392,
-1.40277758422884,-1.40090018600885,-1.39926894611929,-1.39725627461905,
-1.39416297392096,-1.37632827098489,-1.35346024078587,-1.34764165979955,
-1.34389961524338,-1.34254176559955,-1.34158318422872,-1.34072820483503,
-1.33956018512919,-1.33661235638184,-1.31524838903706,-1.29753439872821,
-1.291151877532,-1.28642611251312,-1.284262256449,-1.28261457971463,-1.28082510845336,
-1.27794230562532,-1.26863301093611,-1.24364684020745,-1.22795675751151,
-1.22586436687754,-1.22476337146837,-1.22384867599427,-1.22269833317034,
-1.22087531287728,-1.2104578294475,-1.20197289382995,-1.18755111677402,
-1.17151975238591,-1.16826324412659,-1.16639238783583,-1.16476036438029,
-1.16273837365398,-1.15961475105383,-1.13692504794917,-1.1195456143468,
-1.11336704461743,-1.10943558579736,-1.10802075636541,-1.10706674800836,
-1.10620784428835,-1.10502434185619,-1.10201679037227,-1.08363569870297,
-1.06722778238116,-1.05398717427103,-1.05088339342619,-1.04904563885963,
-1.04740919216897,-1.04533716553315,-1.04110214661615,-1.01139413227062,
-0.998975792054699,-0.994771046868928,-0.991813620582064,-0.990548338519137,
-0.989621606801628,-0.988593758881314,-0.986841354122029,-0.984153281563999),
 .UNSPECIFIED.);
#94=B_SPLINE_CURVE_WITH_KNOTS('',3,(#7978,#7979,#7980,#7981,#7982,#7983,
#7984,#7985,#7986,#7987,#7988,#7989,#7990,#7991,#7992,#7993,#7994,#7995,
#7996,#7997,#7998,#7999,#8000,#8001,#8002,#8003,#8004,#8005,#8006,#8007,
#8008,#8009,#8010,#8011,#8012,#8013,#8014,#8015,#8016,#8017,#8018,#8019,
#8020,#8021,#8022,#8023,#8024,#8025,#8026,#8027,#8028,#8029,#8030,#8031,
#8032,#8033,#8034,#8035,#8036,#8037,#8038,#8039,#8040,#8041,#8042,#8043,
#8044,#8045,#8046,#8047,#8048,#8049,#8050,#8051,#8052,#8053,#8054,#8055,
#8056,#8057,#8058,#8059,#8060,#8061,#8062,#8063,#8064,#8065,#8066,#8067,
#8068,#8069,#8070,#8071,#8072,#8073,#8074,#8075,#8076,#8077,#8078,#8079,
#8080,#8081,#8082,#8083,#8084,#8085,#8086,#8087,#8088,#8089,#8090,#8091,
#8092,#8093,#8094,#8095,#8096,#8097,#8098,#8099,#8100,#8101,#8102,#8103,
#8104,#8105,#8106,#8107,#8108,#8109,#8110,#8111,#8112,#8113,#8114,#8115,
#8116,#8117,#8118,#8119,#8120,#8121,#8122,#8123,#8124,#8125,#8126,#8127,
#8128,#8129),.UNSPECIFIED.,.F.,.F.,(4,2,2,2,2,2,2,2,2,2,2,2,2,2,2,2,2,2,
2,2,2,2,2,2,2,2,2,2,2,2,2,2,2,2,2,2,2,2,2,2,2,2,2,2,2,2,2,2,2,2,2,2,2,2,
2,2,2,2,2,2,2,2,2,2,2,2,2,2,2,2,2,2,2,2,2,4),(-0.500930905015856,-0.489414795378476,
-0.480595938752729,-0.477758763458719,-0.47597915635434,-0.474328044687318,
-0.472141138444648,-0.467287443190145,-0.460677618302062,-0.428398008132838,
-0.420227150845221,-0.418356128387158,-0.41729118119917,-0.416381572424069,
-0.415187698266216,-0.412628080405464,-0.393583200777573,-0.366105453164573,
-0.362080450391464,-0.360024535264082,-0.358496781341437,-0.356822075232639,
-0.354494845907435,-0.348807714003998,-0.340652043927438,-0.310642109202778,
-0.302892970599045,-0.301050213958518,-0.299991670589847,-0.299164427617486,
-0.298006775734322,-0.295635711675723,-0.292483681190909,-0.284583105366693,
-0.261147446158963,-0.246876973565852,-0.243636361419123,-0.241749920146631,
-0.240118931306484,-0.238116888669093,-0.234235985029833,-0.229283045541622,
-0.217545063671744,-0.195864794956641,-0.185881639625283,-0.184077288804618,
-0.182932472356574,-0.18201780299577,-0.180911543136154,-0.178794560374685,
-0.161526427743071,-0.132184626026053,-0.127403791955138,-0.125395489751191,
-0.123727408204824,-0.122047612538427,-0.119598017667965,-0.116786128127286,
-0.11165441678592,-0.0992575921436533,-0.0811582678166073,-0.0687842506521004,
-0.0668904483073508,-0.0657187973444854,-0.0648027827936573,-0.063718642147186,
-0.0617067190957231,-0.0492496180350549,-0.0183593721448643,-0.0110826221428734,
-0.00844911783150569,-0.00688674173760558,-0.00531457785453973,-0.0037118314827622,
-0.00203881054937059,-0.000340422350922375),.UNSPECIFIED.);
#95=B_SPLINE_CURVE_WITH_KNOTS('',3,(#8130,#8131,#8132,#8133,#8134,#8135,
#8136,#8137,#8138,#8139,#8140,#8141,#8142,#8143,#8144,#8145,#8146,#8147,
#8148,#8149,#8150,#8151,#8152,#8153,#8154,#8155,#8156,#8157,#8158,#8159,
#8160,#8161,#8162,#8163,#8164,#8165,#8166,#8167,#8168,#8169,#8170,#8171,
#8172,#8173,#8174,#8175,#8176,#8177,#8178,#8179,#8180,#8181,#8182,#8183,
#8184,#8185,#8186,#8187,#8188,#8189,#8190,#8191,#8192,#8193,#8194,#8195,
#8196,#8197,#8198,#8199,#8200,#8201,#8202,#8203,#8204,#8205,#8206,#8207),
 .UNSPECIFIED.,.F.,.F.,(4,2,2,2,2,2,2,2,2,2,2,2,2,2,2,2,2,2,2,2,2,2,2,2,
2,2,2,2,2,2,2,2,2,2,2,2,2,2,4),(-1.48418639400976,-1.48017874309778,-1.44813213191569,
-1.43936492498694,-1.43434588509554,-1.43279727926195,-1.43181461792903,
-1.43087752427373,-1.42971972877046,-1.42686314038833,-1.40400822573636,
-1.38250883373378,-1.37870546308272,-1.3764143956616,-1.37442443659962,
-1.3743926974679,-1.37435948447998,-1.37432460331821,-1.37275532211427,
-1.37096702527161,-1.36808897032653,-1.35882224098135,-1.33380902979447,
-1.3181100726536,-1.31601778901592,-1.31491689621603,-1.31400230905884,
-1.31285211772264,-1.311029356812,-1.3006132149743,-1.29213604341452,-1.27772466985114,
-1.2616891893659,-1.25843285733839,-1.25656218084475,-1.25493035618873,
-1.25290866190645,-1.2497855829382,-1.24264336813119),.UNSPECIFIED.);
#96=B_SPLINE_CURVE_WITH_KNOTS('',3,(#8208,#8209,#8210,#8211,#8212,#8213,
#8214,#8215,#8216,#8217,#8218,#8219,#8220,#8221,#8222,#8223,#8224,#8225,
#8226,#8227,#8228,#8229,#8230,#8231,#8232,#8233,#8234,#8235,#8236,#8237,
#8238,#8239,#8240,#8241,#8242,#8243,#8244,#8245,#8246,#8247,#8248,#8249,
#8250,#8251,#8252,#8253,#8254,#8255,#8256,#8257,#8258,#8259,#8260,#8261,
#8262,#8263,#8264,#8265,#8266,#8267,#8268,#8269,#8270,#8271,#8272,#8273,
#8274,#8275,#8276,#8277,#8278,#8279,#8280,#8281,#8282,#8283,#8284,#8285,
#8286,#8287,#8288,#8289,#8290,#8291,#8292,#8293,#8294,#8295,#8296,#8297,
#8298,#8299,#8300,#8301,#8302,#8303,#8304,#8305,#8306,#8307,#8308,#8309,
#8310,#8311,#8312,#8313,#8314,#8315,#8316,#8317,#8318,#8319,#8320,#8321,
#8322,#8323,#8324,#8325,#8326,#8327,#8328,#8329,#8330,#8331,#8332,#8333,
#8334,#8335,#8336,#8337,#8338,#8339,#8340,#8341,#8342,#8343,#8344,#8345,
#8346,#8347,#8348,#8349,#8350,#8351,#8352,#8353,#8354,#8355,#8356,#8357,
#8358,#8359,#8360,#8361,#8362,#8363,#8364,#8365,#8366,#8367,#8368,#8369,
#8370,#8371,#8372,#8373,#8374,#8375,#8376,#8377,#8378,#8379,#8380,#8381,
#8382,#8383,#8384,#8385,#8386,#8387,#8388,#8389,#8390,#8391,#8392,#8393,
#8394,#8395,#8396,#8397,#8398,#8399,#8400,#8401,#8402,#8403,#8404,#8405,
#8406,#8407,#8408,#8409,#8410,#8411,#8412,#8413,#8414,#8415,#8416,#8417),
 .UNSPECIFIED.,.F.,.F.,(4,2,2,2,2,2,2,2,2,2,2,2,2,2,2,2,2,2,2,2,2,2,2,2,
2,2,2,2,2,2,2,2,2,2,2,2,2,2,2,2,2,2,2,2,2,2,2,2,2,2,2,2,2,2,2,2,2,2,2,2,
2,2,2,2,2,2,2,2,2,2,2,2,2,2,2,2,2,2,2,2,2,2,2,2,2,2,2,2,2,2,2,2,2,2,2,2,
2,2,2,2,2,2,2,2,4),(-0.984153281563999,-0.980446617635857,-0.949083063846512,
-0.936591368536691,-0.933537702523708,-0.931710902589926,-0.930072520691694,
-0.927982019546928,-0.923650764903865,-0.894761695085295,-0.881852713101108,
-0.877549109366779,-0.874539290610191,-0.873265118657313,-0.872337057184719,
-0.871313400710301,-0.869579882426399,-0.863383163621796,-0.837874039499182,
-0.821409270227159,-0.817122453290162,-0.815040464802325,-0.81340300398146,
-0.811571257252587,-0.808494949596129,-0.797217304573491,-0.771318938491924,
-0.762792088943186,-0.7594773133826,-0.757012183290362,-0.755836340574079,
-0.754920092276665,-0.753839269750242,-0.751897874311517,-0.742542281486401,
-0.728504517050363,-0.704707562090513,-0.700054589302537,-0.697927004308375,
-0.696279176879146,-0.694489573228853,-0.691606626505655,-0.681277053976863,
-0.661140117196513,-0.643143298927895,-0.640120276386359,-0.638934177437661,
-0.638074599347353,-0.637121288783701,-0.635709964603215,-0.631804037019758,
-0.625681908418129,-0.60818730993821,-0.585548075802756,-0.582424636816855,
-0.580402655879584,-0.578770581989299,-0.576899603585641,-0.57364272427195,
-0.557608573605474,-0.54317306108342,-0.534678952657553,-0.524257815881781,
-0.522434485016907,-0.521284032655635,-0.520369300741631,-0.519268317035172,
-0.51717611250087,-0.501489747364672,-0.476508929189119,-0.467211192134723,
-0.464329542869904,-0.462540255681777,-0.460892390730031,-0.458727765152341,
-0.45399821087008,-0.447608380182307,-0.429860312323292,-0.408515568527029,
-0.405575784391122,-0.404403626315586,-0.403547572696955,-0.402590166129962,
-0.401159011280747,-0.397107348330107,-0.390664890546024,-0.373598181545457,
-0.351047533758038,-0.347921737886868,-0.345899064831565,-0.344266973291212,
-0.342396567963362,-0.339142225044656,-0.323161567880343,-0.308687691348596,
-0.300177412819621,-0.289754124345347,-0.287930737351276,-0.28678028110471,
-0.285865567874966,-0.28476463283225,-0.28267259205122,-0.266993032297975,
-0.242029482469724,-0.241988514754038),.UNSPECIFIED.);
#97=B_SPLINE_CURVE_WITH_KNOTS('',3,(#8422,#8423,#8424,#8425,#8426,#8427,
#8428,#8429,#8430,#8431,#8432,#8433,#8434,#8435,#8436,#8437,#8438,#8439,
#8440,#8441,#8442,#8443,#8444,#8445,#8446,#8447,#8448,#8449,#8450,#8451,
#8452,#8453,#8454,#8455,#8456,#8457,#8458,#8459,#8460,#8461,#8462,#8463,
#8464,#8465,#8466,#8467,#8468,#8469,#8470,#8471,#8472,#8473,#8474,#8475,
#8476,#8477,#8478,#8479,#8480,#8481,#8482,#8483,#8484,#8485,#8486,#8487,
#8488,#8489,#8490,#8491,#8492,#8493,#8494,#8495,#8496,#8497,#8498,#8499,
#8500,#8501,#8502,#8503,#8504,#8505,#8506,#8507,#8508,#8509,#8510,#8511,
#8512,#8513,#8514,#8515,#8516,#8517,#8518,#8519,#8520,#8521,#8522,#8523,
#8524,#8525,#8526,#8527,#8528,#8529,#8530,#8531,#8532,#8533,#8534,#8535,
#8536,#8537,#8538,#8539,#8540,#8541,#8542,#8543,#8544,#8545,#8546,#8547,
#8548,#8549,#8550,#8551,#8552,#8553,#8554,#8555,#8556,#8557,#8558,#8559,
#8560,#8561,#8562,#8563,#8564,#8565,#8566,#8567,#8568,#8569,#8570,#8571,
#8572,#8573,#8574,#8575,#8576,#8577,#8578,#8579,#8580,#8581,#8582,#8583,
#8584,#8585,#8586,#8587,#8588,#8589,#8590,#8591,#8592,#8593,#8594,#8595,
#8596,#8597,#8598,#8599,#8600,#8601,#8602,#8603,#8604,#8605,#8606,#8607,
#8608,#8609,#8610,#8611,#8612,#8613,#8614,#8615,#8616,#8617,#8618,#8619,
#8620,#8621,#8622,#8623,#8624,#8625,#8626,#8627,#8628,#8629,#8630,#8631,
#8632,#8633,#8634,#8635,#8636,#8637,#8638,#8639,#8640,#8641),
 .UNSPECIFIED.,.F.,.F.,(4,2,2,2,2,2,2,2,2,2,2,2,2,2,2,2,2,2,2,2,2,2,2,2,
2,2,2,2,2,2,2,2,2,2,2,2,2,2,2,2,2,2,2,2,2,2,2,2,2,2,2,2,2,2,2,2,2,2,2,2,
2,2,2,2,2,2,2,2,2,2,2,2,2,2,2,2,2,2,2,2,2,2,2,2,2,2,2,2,2,2,2,2,2,2,2,2,
2,2,2,2,2,2,2,2,2,2,2,2,2,4),(-1.24309113755231,-1.24126632442143,-1.23926693276646,
-1.23818551144056,-1.23726931749502,-1.23609426338528,-1.23418889070891,
-1.22070590490734,-1.20365940695935,-1.19133512542798,-1.18622278579794,
-1.18224411471887,-1.18022252406742,-1.17859044478126,-1.17671910482104,
-1.17354442737101,-1.16041497062373,-1.13617349906431,-1.12795365152909,
-1.12471798954741,-1.12229851255801,-1.12113146376042,-1.12030323585615,
-1.1192512898428,-1.11743710707711,-1.11007707877698,-1.07700856402774,
-1.07034271672478,-1.06545718590742,-1.06326463847935,-1.06161268595253,
-1.06005198049401,-1.05742696370277,-1.05023108217569,-1.01996261489869,
-1.011014805984,-1.00759389292042,-1.00506801745253,-1.00388055851729,-1.00296334148134,
-1.00189079039497,-0.999986105325724,-0.991285744971732,-0.962219334169995,
-0.950029067899264,-0.946996787179803,-0.94517463843108,-0.943535289520301,
-0.941436438524951,-0.937061427575507,-0.908584851671165,-0.895426743947146,
-0.891074050475468,-0.888038379096605,-0.886759841993951,-0.88583109090128,
-0.884809376542716,-0.883084673218698,-0.876978109408967,-0.851427419565153,
-0.834915369678608,-0.830622566689491,-0.828539422348956,-0.826901825757826,
-0.825070727683588,-0.8219974302899,-0.810758391755525,-0.781563306750961,
-0.775161278486433,-0.771128184394633,-0.769699464254831,-0.768742529345625,
-0.767885987986307,-0.766712021933907,-0.763761749195055,-0.74268854491404,
-0.71816638474444,-0.713534668857383,-0.711410893274628,-0.709763583211138,
-0.707972100616846,-0.705080685803936,-0.694656025852426,-0.67416984738979,
-0.666168391592487,-0.662640378933236,-0.654752555190516,-0.652900405974989,
-0.651839801655332,-0.651012996072326,-0.649858599354989,-0.647503607729981,
-0.644378949607415,-0.636580779371404,-0.613342325985203,-0.598757587071977,
-0.595500471328468,-0.593610442358724,-0.591979933870467,-0.589983012305076,
-0.586126567446377,-0.563670628477222,-0.538968082207945,-0.536170996631755,
-0.534946939717794,-0.534023014778787,-0.532985361727387,-0.531188471005012,
-0.523278635959589,-0.500930905015856),.UNSPECIFIED.);
#98=B_SPLINE_CURVE_WITH_KNOTS('',3,(#8643,#8644,#8645,#8646,#8647,#8648,
#8649,#8650,#8651,#8652,#8653,#8654,#8655,#8656,#8657,#8658,#8659,#8660,
#8661,#8662,#8663,#8664,#8665,#8666,#8667,#8668,#8669,#8670,#8671,#8672,
#8673,#8674,#8675,#8676,#8677,#8678,#8679,#8680,#8681,#8682,#8683,#8684,
#8685,#8686,#8687,#8688,#8689,#8690,#8691,#8692,#8693,#8694,#8695,#8696,
#8697,#8698,#8699,#8700,#8701,#8702,#8703,#8704,#8705,#8706,#8707,#8708,
#8709,#8710,#8711,#8712,#8713,#8714,#8715,#8716),.UNSPECIFIED.,.F.,.F.,
(4,2,2,2,2,2,2,2,2,2,2,2,2,2,2,2,2,2,2,2,2,2,2,2,2,2,2,2,2,2,2,2,2,2,2,
2,4),(-0.241988514754038,-0.232712639227085,-0.229829016152512,-0.228039324207548,
-0.226391634885176,-0.224228041812203,-0.219504030892733,-0.213123918449792,
-0.195422977376067,-0.17401126592963,-0.17106329479951,-0.16989529214844,
-0.169040282082338,-0.168081604915298,-0.166644328235717,-0.162546644592089,
-0.156001480166582,-0.124671258454934,-0.115424722653325,-0.112548598795624,
-0.110760591377874,-0.109185782200507,-0.109157460453551,-0.109130732410267,
-0.10712992737639,-0.104851867839005,-0.101080791656546,-0.0809630231652105,
-0.0564594984009954,-0.053641854435739,-0.0524142889581039,-0.0514899538839555,
-0.0504544029297609,-0.0486667149753297,-0.0408919222111806,-0.00875195972409242,
-0.000340782874575415),.UNSPECIFIED.);
#99=B_SPLINE_CURVE_WITH_KNOTS('',3,(#8717,#8718,#8719,#8720,#8721,#8722,
#8723,#8724,#8725,#8726,#8727,#8728,#8729,#8730,#8731,#8732,#8733,#8734,
#8735,#8736,#8737,#8738,#8739,#8740,#8741,#8742,#8743,#8744,#8745,#8746,
#8747,#8748,#8749,#8750,#8751,#8752,#8753,#8754,#8755,#8756,#8757,#8758,
#8759,#8760,#8761,#8762,#8763,#8764,#8765,#8766,#8767,#8768,#8769,#8770,
#8771,#8772,#8773,#8774,#8775,#8776,#8777,#8778,#8779,#8780,#8781,#8782,
#8783,#8784,#8785,#8786,#8787,#8788,#8789,#8790,#8791,#8792,#8793,#8794,
#8795,#8796,#8797,#8798,#8799,#8800,#8801,#8802,#8803,#8804,#8805,#8806,
#8807,#8808,#8809,#8810,#8811,#8812,#8813,#8814,#8815,#8816,#8817,#8818,
#8819,#8820,#8821,#8822,#8823,#8824,#8825,#8826,#8827,#8828,#8829,#8830,
#8831,#8832,#8833,#8834,#8835,#8836,#8837,#8838,#8839,#8840,#8841,#8842,
#8843,#8844,#8845,#8846,#8847,#8848,#8849,#8850,#8851,#8852,#8853,#8854,
#8855,#8856,#8857,#8858,#8859,#8860,#8861,#8862,#8863,#8864,#8865,#8866),
 .UNSPECIFIED.,.F.,.F.,(4,2,2,2,2,2,2,2,2,2,2,2,2,2,2,2,2,2,2,2,2,2,2,2,
2,2,2,2,2,2,2,2,2,2,2,2,2,2,2,2,2,2,2,2,2,2,2,2,2,2,2,2,2,2,2,2,2,2,2,2,
2,2,2,2,2,2,2,2,2,2,2,2,2,2,4),(-1.48412001715137,-1.48190965603259,-1.47983659088756,
-1.47821563782734,-1.47666047664527,-1.47491530913237,-1.47223351354066,
-1.46458778411192,-1.434944769811,-1.42176781561533,-1.41973510949454,-1.41864711061999,
-1.41773226021195,-1.41656776312692,-1.41469626621342,-1.40289891138794,
-1.36951389790073,-1.36549205973259,-1.36311358723029,-1.36097061927544,
-1.35935005515891,-1.35758157780193,-1.3547914425417,-1.3462989039611,-1.31205232442885,
-1.30411659550579,-1.30231887845869,-1.30128152637233,-1.30035841499434,
-1.29913618082103,-1.29634635071621,-1.27162529681923,-1.25609533368068,
-1.2501881548139,-1.24573650734627,-1.24362399052763,-1.24198390753885,
-1.24017105395127,-1.23717796753591,-1.22680454173612,-1.1967129446604,
-1.19024934602209,-1.18618921672579,-1.184757430969,-1.18380027507081,-1.18294496095465,
-1.18177447330326,-1.17884223239724,-1.1573354928398,-1.139736836888,-1.13337936496933,
-1.12866837701041,-1.12650784113347,-1.12486129200661,-1.12307167744254,
-1.12018560251057,-1.11083640832922,-1.07962041459186,-1.07308229491254,
-1.06898866688826,-1.06755232586779,-1.06659414786319,-1.06573948144598,
-1.06457183281278,-1.06162488567421,-1.0402706189335,-1.02256290960806,
-1.01618274884087,-1.01145875357087,-1.00929572808906,-1.0076486919997,
-1.00585992449612,-1.0029782730818,-0.99367286509119,-0.983793564935614),
 .UNSPECIFIED.);
#100=B_SPLINE_CURVE_WITH_KNOTS('',3,(#8872,#8873,#8874,#8875,#8876,#8877,
#8878,#8879,#8880,#8881,#8882,#8883,#8884,#8885,#8886,#8887,#8888,#8889,
#8890,#8891,#8892,#8893,#8894,#8895,#8896,#8897,#8898,#8899,#8900,#8901,
#8902,#8903,#8904,#8905,#8906,#8907,#8908,#8909,#8910,#8911,#8912,#8913,
#8914,#8915,#8916,#8917,#8918,#8919,#8920,#8921,#8922,#8923,#8924,#8925,
#8926,#8927,#8928,#8929,#8930,#8931,#8932,#8933,#8934,#8935,#8936,#8937,
#8938,#8939,#8940,#8941,#8942,#8943,#8944,#8945,#8946,#8947,#8948,#8949,
#8950,#8951,#8952,#8953,#8954,#8955,#8956,#8957,#8958,#8959,#8960,#8961,
#8962,#8963,#8964,#8965,#8966,#8967,#8968,#8969,#8970,#8971,#8972,#8973,
#8974,#8975,#8976,#8977,#8978,#8979,#8980,#8981,#8982,#8983,#8984,#8985,
#8986,#8987,#8988,#8989,#8990,#8991,#8992,#8993,#8994,#8995,#8996,#8997,
#8998,#8999,#9000,#9001,#9002,#9003,#9004,#9005,#9006,#9007,#9008,#9009,
#9010,#9011,#9012,#9013,#9014,#9015),.UNSPECIFIED.,.F.,.F.,(4,2,2,2,2,2,
2,2,2,2,2,2,2,2,2,2,2,2,2,2,2,2,2,2,2,2,2,2,2,2,2,2,2,2,2,2,2,2,2,2,2,2,
2,2,2,2,2,2,2,2,2,2,2,2,2,2,2,2,2,2,2,2,2,2,2,2,2,2,2,2,2,4),(-0.500819173945887,
-0.493777206906728,-0.479351861776628,-0.470865801088027,-0.46044512596012,
-0.458621959504854,-0.457471604552115,-0.456556942202042,-0.45545601971394,
-0.45336385714678,-0.437669222525489,-0.412663201038334,-0.403404091249994,
-0.400526694865227,-0.398738425051046,-0.39709040679574,-0.394923978418504,
-0.3901838706952,-0.383775228035058,-0.365932818995212,-0.344738336504506,
-0.341783031791153,-0.340613829838816,-0.339758555185984,-0.338800324047081,
-0.337364989287407,-0.333281494086993,-0.32676777916111,-0.29591966733786,
-0.286246301329913,-0.283324121186216,-0.281526137556155,-0.279881133613596,
-0.277735991188525,-0.27311239074608,-0.266907954555483,-0.25004233161852,
-0.227383301044488,-0.22451310642436,-0.223352907767055,-0.222415134207218,
-0.221433302782806,-0.219888710254711,-0.214906469089431,-0.206235806671276,
-0.17915184505782,-0.169099215949359,-0.166134623139714,-0.164327402676302,
-0.162684900855216,-0.160558631331137,-0.156036957893393,-0.150009388874568,
-0.133951888692588,-0.110018687787216,-0.107175144709924,-0.106053229930523,
-0.105125192411495,-0.104146874338745,-0.102648556808029,-0.100813822341213,
-0.0972150595024378,-0.0875372674535842,-0.0783689936404857,-0.054706126379121,
-0.0500515005800035,-0.0479237987091279,-0.0462761366731087,-0.0444869649045571,
-0.0416052648876107,-0.0312863423734425,-0.000340942165246433),
 .UNSPECIFIED.);
#101=B_SPLINE_CURVE_WITH_KNOTS('',3,(#9016,#9017,#9018,#9019,#9020,#9021,
#9022,#9023,#9024,#9025,#9026,#9027,#9028,#9029,#9030,#9031,#9032,#9033,
#9034,#9035,#9036,#9037,#9038,#9039,#9040,#9041,#9042,#9043,#9044,#9045,
#9046,#9047,#9048,#9049,#9050,#9051,#9052,#9053,#9054,#9055,#9056,#9057,
#9058,#9059,#9060,#9061,#9062,#9063,#9064,#9065,#9066,#9067,#9068,#9069,
#9070,#9071,#9072,#9073,#9074,#9075,#9076,#9077,#9078,#9079,#9080,#9081,
#9082,#9083,#9084,#9085,#9086,#9087,#9088,#9089,#9090,#9091),
 .UNSPECIFIED.,.F.,.F.,(4,2,2,2,2,2,2,2,2,2,2,2,2,2,2,2,2,2,2,2,2,2,2,2,
2,2,2,2,2,2,2,2,2,2,2,2,2,4),(-1.48462944420424,-1.47854706264515,-1.47522746968644,
-1.47396875633596,-1.47304062285797,-1.47216955552764,-1.4711705878605,
-1.46954819973224,-1.46438832786397,-1.45664645350163,-1.44275484241869,
-1.42063070257591,-1.41669766923023,-1.41468548338647,-1.41305434599212,
-1.41117673959019,-1.40797348414356,-1.39435211355748,-1.3618191261588,
-1.35889281860234,-1.35730422023743,-1.35594276665795,-1.35500797741246,
-1.35414906110552,-1.35296547144243,-1.34995731772499,-1.33148899974201,
-1.31239607042987,-1.30523902346609,-1.30008214116386,-1.29784236701082,
-1.2961829427663,-1.29442385838963,-1.29168153576673,-1.28359941082173,
-1.27740114420268,-1.25334811321103,-1.24309113755231),.UNSPECIFIED.);
#102=B_SPLINE_CURVE_WITH_KNOTS('',3,(#9092,#9093,#9094,#9095,#9096,#9097,
#9098,#9099,#9100,#9101,#9102,#9103,#9104,#9105,#9106,#9107,#9108,#9109,
#9110,#9111,#9112,#9113,#9114,#9115,#9116,#9117,#9118,#9119,#9120,#9121,
#9122,#9123,#9124,#9125,#9126,#9127,#9128,#9129,#9130,#9131,#9132,#9133,
#9134,#9135,#9136,#9137,#9138,#9139,#9140,#9141,#9142,#9143,#9144,#9145,
#9146,#9147,#9148,#9149,#9150,#9151,#9152,#9153,#9154,#9155,#9156,#9157,
#9158,#9159,#9160,#9161,#9162,#9163,#9164,#9165,#9166,#9167,#9168,#9169,
#9170,#9171,#9172,#9173,#9174,#9175,#9176,#9177,#9178,#9179,#9180,#9181,
#9182,#9183,#9184,#9185,#9186,#9187,#9188,#9189,#9190,#9191,#9192,#9193,
#9194,#9195,#9196,#9197,#9198,#9199,#9200,#9201,#9202,#9203,#9204,#9205,
#9206,#9207,#9208,#9209,#9210,#9211,#9212,#9213,#9214,#9215,#9216,#9217,
#9218,#9219,#9220,#9221,#9222,#9223,#9224,#9225,#9226,#9227,#9228,#9229,
#9230,#9231,#9232,#9233,#9234,#9235,#9236,#9237,#9238,#9239,#9240,#9241,
#9242,#9243,#9244,#9245,#9246,#9247,#9248,#9249,#9250,#9251,#9252,#9253,
#9254,#9255,#9256,#9257,#9258,#9259,#9260,#9261,#9262,#9263,#9264,#9265,
#9266,#9267,#9268,#9269,#9270,#9271,#9272,#9273,#9274,#9275,#9276,#9277,
#9278,#9279,#9280,#9281,#9282,#9283,#9284,#9285,#9286,#9287,#9288,#9289,
#9290,#9291,#9292,#9293,#9294,#9295,#9296,#9297,#9298,#9299,#9300,#9301,
#9302,#9303,#9304,#9305,#9306,#9307),.UNSPECIFIED.,.F.,.F.,(4,2,2,2,2,2,
2,2,2,2,2,2,2,2,2,2,2,2,2,2,2,2,2,2,2,2,2,2,2,2,2,2,2,2,2,2,2,2,2,2,2,2,
2,2,2,2,2,2,2,2,2,2,2,2,2,2,2,2,2,2,2,2,2,2,2,2,2,2,2,2,2,2,2,2,2,2,2,2,
2,2,2,2,2,2,2,2,2,2,2,2,2,2,2,2,2,2,2,2,2,2,2,2,2,2,2,2,2,4),(-0.983793564935614,
-0.968696261868599,-0.953012236160266,-0.950920660055713,-0.949820093400412,
-0.948905754416435,-0.947755860133233,-0.94593355059917,-0.935520123495261,
-0.927038511042748,-0.912622359712589,-0.896597264859473,-0.893342027870717,
-0.891471901615443,-0.889840514812668,-0.887819312617179,-0.884696907671688,
-0.862006562726232,-0.84461534549455,-0.838456713890232,-0.83453482699478,
-0.833121656489663,-0.832168248187483,-0.831309478421971,-0.83012564474862,
-0.827114483444018,-0.80896740956612,-0.788966357616482,-0.778676332009486,
-0.775797756300876,-0.774009570297988,-0.772362179491771,-0.770233937309615,
-0.76557450857,-0.742147073738758,-0.719937075314893,-0.717037065860415,
-0.715871903558975,-0.714932951359228,-0.713953374336011,-0.712418376972951,
-0.707519867930903,-0.699062837519007,-0.673570092699887,-0.661895314942863,
-0.658784935592021,-0.656946187079544,-0.655474223034174,-0.653485438433571,
-0.649666558844556,-0.628488494720904,-0.605952493049906,-0.600576136686598,
-0.598928918820536,-0.597924571068326,-0.596989138598303,-0.595669372942323,
-0.592379584239752,-0.587534244208183,-0.571664837309244,-0.547185012169975,
-0.542553243950537,-0.540429926712259,-0.538783175839867,-0.536992509009948,
-0.53410288231899,-0.523690579447275,-0.503245278973118,-0.49561067002373,
-0.490805137257805,-0.483680188068646,-0.481864029236699,-0.480822423448885,
-0.479900000765593,-0.478663191227497,-0.475867189104592,-0.463284699551626,
-0.441127668571468,-0.427682290649862,-0.42449054103066,-0.422615744908427,
-0.420984667879787,-0.418969499525952,-0.415020622489202,-0.391301557665565,
-0.368192272870674,-0.365345349402046,-0.364189279578466,-0.363252698628978,
-0.362269478355352,-0.360718098347127,-0.355672958115622,-0.346838923238608,
-0.317118075265111,-0.309394102414707,-0.306698136847339,-0.304949386529126,
-0.303285762257949,-0.30101843144945,-0.295695787017629,-0.269354114211768,
-0.251184887950499,-0.24817287021915,-0.24698881359996,-0.246129927382777,
-0.245176433937095,-0.243763221929403,-0.241871924735937),.UNSPECIFIED.);
#103=B_SPLINE_CURVE_WITH_KNOTS('',3,(#9312,#9313,#9314,#9315,#9316,#9317,
#9318,#9319,#9320,#9321,#9322,#9323,#9324,#9325,#9326,#9327,#9328,#9329,
#9330,#9331,#9332,#9333,#9334,#9335,#9336,#9337,#9338,#9339,#9340,#9341,
#9342,#9343,#9344,#9345,#9346,#9347,#9348,#9349,#9350,#9351,#9352,#9353,
#9354,#9355,#9356,#9357,#9358,#9359,#9360,#9361,#9362,#9363,#9364,#9365,
#9366,#9367,#9368,#9369,#9370,#9371,#9372,#9373,#9374,#9375,#9376,#9377,
#9378,#9379,#9380,#9381,#9382,#9383,#9384,#9385,#9386,#9387,#9388,#9389,
#9390,#9391,#9392,#9393,#9394,#9395,#9396,#9397,#9398,#9399,#9400,#9401,
#9402,#9403,#9404,#9405,#9406,#9407,#9408,#9409,#9410,#9411,#9412,#9413,
#9414,#9415,#9416,#9417,#9418,#9419,#9420,#9421,#9422,#9423,#9424,#9425,
#9426,#9427,#9428,#9429,#9430,#9431,#9432,#9433,#9434,#9435,#9436,#9437,
#9438,#9439,#9440,#9441,#9442,#9443,#9444,#9445,#9446,#9447,#9448,#9449,
#9450,#9451,#9452,#9453,#9454,#9455,#9456,#9457,#9458,#9459,#9460,#9461,
#9462,#9463,#9464,#9465,#9466,#9467,#9468,#9469,#9470,#9471,#9472,#9473,
#9474,#9475,#9476,#9477,#9478,#9479,#9480,#9481,#9482,#9483,#9484,#9485,
#9486,#9487,#9488,#9489,#9490,#9491,#9492,#9493,#9494,#9495,#9496,#9497,
#9498,#9499,#9500,#9501,#9502,#9503,#9504,#9505,#9506,#9507,#9508,#9509,
#9510,#9511,#9512,#9513,#9514,#9515,#9516,#9517,#9518,#9519,#9520,#9521,
#9522,#9523,#9524,#9525,#9526,#9527,#9528,#9529,#9530,#9531,#9532,#9533),
 .UNSPECIFIED.,.F.,.F.,(4,2,2,2,2,2,2,2,2,2,2,2,2,2,2,2,2,2,2,2,2,2,2,2,
2,2,2,2,2,2,2,2,2,2,2,2,2,2,2,2,2,2,2,2,2,2,2,2,2,2,2,2,2,2,2,2,2,2,2,2,
2,2,2,2,2,2,2,2,2,2,2,2,2,2,2,2,2,2,2,2,2,2,2,2,2,2,2,2,2,2,2,2,2,2,2,2,
2,2,2,2,2,2,2,2,2,2,2,2,2,2,4),(-1.2428172115265,-1.24249234473694,-1.23078262926944,
-1.22583767315457,-1.22196155341259,-1.21996074205993,-1.21833014567714,
-1.21644347476855,-1.21320076899999,-1.19888499679281,-1.17546559847501,
-1.16757628439986,-1.16442755563331,-1.1620586984377,-1.16090161783892,
-1.1600745816541,-1.15901600819455,-1.15717257801453,-1.14940924389079,
-1.11943961512502,-1.11129047521323,-1.10560639889848,-1.10327989549632,
-1.10160552361073,-1.10007794037801,-1.09802205322527,-1.09399646262687,
-1.0665154066557,-1.05272569646497,-1.04825145863456,-1.04515223747807,
-1.04386315972315,-1.04293278083638,-1.04191580163504,-1.04021226373077,
-1.03431527911758,-1.00862299086621,-0.992024560629506,-0.987720938971641,
-0.985635831704979,-0.983998149664809,-0.982168469399791,-0.979101195136434,
-0.967936794679667,-0.944515512125686,-0.93420287263835,-0.928615632696912,
-0.927007549208844,-0.926011699898189,-0.925082284623874,-0.923954855652924,
-0.92107657660576,-0.897310699738304,-0.881187617793249,-0.875145220086792,
-0.870614478764588,-0.868486417478237,-0.866843569632226,-0.865037008816023,
-0.862075896748497,-0.852060176738265,-0.827694828606197,-0.81224622831273,
-0.810158395254423,-0.809058347262913,-0.808143592794,-0.806992095849127,
-0.805165263453635,-0.794652144959133,-0.767275694831161,-0.755350953423724,
-0.752338216961626,-0.750520388425605,-0.748880210691996,-0.746773728485989,
-0.742358109158383,-0.724862609446661,-0.706516547946201,-0.70154835440642,
-0.694523523075217,-0.69271538809805,-0.69167536361139,-0.690752218469142,
-0.689511555996434,-0.686694981166887,-0.67392358609147,-0.666933433456118,
-0.640706684604885,-0.636150813889163,-0.634040978294949,-0.632395805915498,
-0.630597882793247,-0.627676358967061,-0.616901059222625,-0.597898551376377,
-0.57928969230207,-0.576276161915608,-0.57509169726426,-0.574232578310295,
-0.573278894949353,-0.571865504691222,-0.5679441006064,-0.561788004791788,
-0.544404412671272,-0.521721132984155,-0.518598128564709,-0.516576365329992,
-0.514944421395287,-0.513073538066115,-0.509816672449976,-0.500819173945887),
 .UNSPECIFIED.);
#104=B_SPLINE_CURVE_WITH_KNOTS('',3,(#9535,#9536,#9537,#9538,#9539,#9540,
#9541,#9542,#9543,#9544,#9545,#9546,#9547,#9548,#9549,#9550,#9551,#9552,
#9553,#9554,#9555,#9556,#9557,#9558,#9559,#9560,#9561,#9562,#9563,#9564,
#9565,#9566,#9567,#9568,#9569,#9570,#9571,#9572,#9573,#9574,#9575,#9576,
#9577,#9578,#9579,#9580,#9581,#9582,#9583,#9584,#9585,#9586,#9587,#9588,
#9589,#9590,#9591,#9592,#9593,#9594,#9595,#9596,#9597,#9598,#9599,#9600,
#9601,#9602,#9603,#9604,#9605,#9606,#9607,#9608,#9609,#9610),
 .UNSPECIFIED.,.F.,.F.,(4,2,2,2,2,2,2,2,2,2,2,2,2,2,2,2,2,2,2,2,2,2,2,2,
2,2,2,2,2,2,2,2,2,2,2,2,2,4),(-0.241871924735937,-0.239841673385435,-0.233684822665038,
-0.216303692719354,-0.193622004876805,-0.190499538363504,-0.18847818442888,
-0.186846614987625,-0.184976213068143,-0.181720332570845,-0.165690973487894,
-0.140556038965802,-0.132138525183534,-0.130251016583305,-0.129182537690494,
-0.128282805778212,-0.127132854326775,-0.125848452014372,-0.123703968120966,
-0.119203879859423,-0.105275452917386,-0.0780319460560208,-0.0735452913502586,
-0.0714484189340119,-0.0698052957158563,-0.0680013910808192,-0.0650514232092265,
-0.0539293515464517,-0.0259234861970813,-0.0183744785915654,-0.0141211811940812,
-0.0126154182771393,-0.0117388268599531,-0.0108674173226553,-0.00993989921184121,
-0.00868279022866366,-0.00563249670091923,-0.000340252375207522),
 .UNSPECIFIED.);
#105=B_SPLINE_CURVE_WITH_KNOTS('',3,(#9611,#9612,#9613,#9614,#9615,#9616,
#9617,#9618,#9619,#9620,#9621,#9622,#9623,#9624,#9625,#9626,#9627,#9628,
#9629,#9630,#9631,#9632,#9633,#9634,#9635,#9636,#9637,#9638,#9639,#9640,
#9641,#9642,#9643,#9644,#9645,#9646,#9647,#9648,#9649,#9650,#9651,#9652,
#9653,#9654,#9655,#9656,#9657,#9658,#9659,#9660,#9661,#9662,#9663,#9664,
#9665,#9666,#9667,#9668,#9669,#9670,#9671,#9672,#9673,#9674,#9675,#9676,
#9677,#9678,#9679,#9680,#9681,#9682,#9683,#9684,#9685,#9686,#9687,#9688,
#9689,#9690,#9691,#9692,#9693,#9694,#9695,#9696,#9697,#9698,#9699,#9700,
#9701,#9702,#9703,#9704,#9705,#9706,#9707,#9708,#9709,#9710,#9711,#9712,
#9713,#9714,#9715,#9716,#9717,#9718,#9719,#9720,#9721,#9722,#9723,#9724,
#9725,#9726,#9727,#9728,#9729,#9730,#9731,#9732,#9733,#9734,#9735,#9736,
#9737,#9738,#9739,#9740,#9741,#9742,#9743,#9744,#9745,#9746,#9747,#9748,
#9749,#9750,#9751,#9752,#9753,#9754),.UNSPECIFIED.,.F.,.F.,(4,2,2,2,2,2,
2,2,2,2,2,2,2,2,2,2,2,2,2,2,2,2,2,2,2,2,2,2,2,2,2,2,2,2,2,2,2,2,2,2,2,2,
2,2,2,2,2,2,2,2,2,2,2,2,2,2,2,2,2,2,2,2,2,2,2,2,2,2,2,2,2,4),(-1.48448022972756,
-1.45253145118343,-1.44218218330809,-1.43929849412675,-1.43750929736548,
-1.43586242197044,-1.43373687449237,-1.42909174084597,-1.40503566329731,
-1.39117708996751,-1.384849204403,-1.38213576934346,-1.38062823722837,-1.3793554103156,
-1.37842741728136,-1.37756250831909,-1.37635473994927,-1.37386053420512,
-1.34906907763824,-1.33355666097405,-1.32765311333543,-1.32320341324644,
-1.32109104869219,-1.31945075265988,-1.31763732764823,-1.31464251382629,
-1.30425463192307,-1.27417162459092,-1.26770788105642,-1.26364749278658,
-1.26221552349324,-1.2612582190253,-1.26040275212933,-1.25923203030285,
-1.25629907348894,-1.2347941477793,-1.21718886179115,-1.2108295659136,-1.20611735705056,
-1.20395638083128,-1.20230954473904,-1.20051966578124,-1.19763327014716,
-1.18828405633806,-1.15706112532489,-1.15052180244857,-1.14642744035259,
-1.14499085223529,-1.14403251230689,-1.14317770370543,-1.14200986362902,
-1.13906243745354,-1.11770396783046,-1.09999372397697,-1.09361258272429,
-1.0888878461881,-1.08672446734085,-1.08507715652161,-1.0832880851261,-1.08040593189491,
-1.07109878533898,-1.0461181513722,-1.03043155715585,-1.02833963162282,
-1.02723888075393,-1.02632438852579,-1.02517430126548,-1.02335168544546,
-1.01293649113938,-1.0044532045271,-0.990034106714849,-0.98405823001278),
 .UNSPECIFIED.);
#106=B_SPLINE_CURVE_WITH_KNOTS('',3,(#9760,#9761,#9762,#9763,#9764,#9765,
#9766,#9767,#9768,#9769,#9770,#9771,#9772,#9773,#9774,#9775,#9776,#9777,
#9778,#9779,#9780,#9781,#9782,#9783,#9784,#9785,#9786,#9787,#9788,#9789,
#9790,#9791,#9792,#9793,#9794,#9795,#9796,#9797,#9798,#9799,#9800,#9801,
#9802,#9803,#9804,#9805,#9806,#9807,#9808,#9809,#9810,#9811,#9812,#9813,
#9814,#9815,#9816,#9817,#9818,#9819,#9820,#9821,#9822,#9823,#9824,#9825,
#9826,#9827,#9828,#9829,#9830,#9831,#9832,#9833,#9834,#9835,#9836,#9837,
#9838,#9839,#9840,#9841,#9842,#9843,#9844,#9845,#9846,#9847,#9848,#9849,
#9850,#9851,#9852,#9853,#9854,#9855,#9856,#9857,#9858,#9859,#9860,#9861,
#9862,#9863,#9864,#9865,#9866,#9867,#9868,#9869,#9870,#9871,#9872,#9873,
#9874,#9875,#9876,#9877,#9878,#9879,#9880,#9881,#9882,#9883,#9884,#9885,
#9886,#9887,#9888,#9889,#9890,#9891,#9892,#9893,#9894,#9895,#9896,#9897,
#9898,#9899,#9900,#9901,#9902,#9903,#9904,#9905,#9906,#9907,#9908,#9909,
#9910,#9911),.UNSPECIFIED.,.F.,.F.,(4,2,2,2,2,2,2,2,2,2,2,2,2,2,2,2,2,2,
2,2,2,2,2,2,2,2,2,2,2,2,2,2,2,2,2,2,2,2,2,2,2,2,2,2,2,2,2,2,2,2,2,2,2,2,
2,2,2,2,2,2,2,2,2,2,2,2,2,2,2,2,2,2,2,2,2,4),(-0.500712197120109,-0.499886588927617,
-0.498155634717826,-0.497132550335824,-0.496204286833124,-0.494928847679332,
-0.49191148215954,-0.487594006162487,-0.474614145976675,-0.445876781470393,
-0.441532128751737,-0.43943907733086,-0.437800407536301,-0.435975047452157,
-0.432927988268123,-0.420531219258952,-0.389962238813033,-0.38277887871243,
-0.380978607154051,-0.379929844830267,-0.379101012200458,-0.377929061452973,
-0.375484354622653,-0.372205387236876,-0.363818660474139,-0.338725789014427,
-0.326592632820325,-0.323449679782123,-0.321603330348852,-0.32013166466181,
-0.318151563245263,-0.314377722233372,-0.309597958210389,-0.298478375150139,
-0.27580250107145,-0.265844271387734,-0.26404297498217,-0.262899131515969,
-0.261984564462171,-0.260877612020439,-0.258757038578453,-0.241186104621821,
-0.211088678604902,-0.206906604019289,-0.204844851656629,-0.203209403655764,
-0.201365249478619,-0.198232142414803,-0.184522712491843,-0.168436853651836,
-0.15024396269488,-0.14723214677337,-0.146047909429669,-0.145188801950515,
-0.144234946323207,-0.142879572072936,-0.13924028239031,-0.133634208548949,
-0.113594284681153,-0.092707884315093,-0.089566733559867,-0.0875393766573888,
-0.0859068978359904,-0.0840397526215277,-0.0810718295493039,-0.0680879069889224,
-0.0504342275555722,-0.0419858476100865,-0.0314035321927687,-0.0295737764242259,
-0.0284213811036784,-0.0275065538783484,-0.026407182221728,-0.0252248357174609,
-0.0233328873464089,-0.00034061238379718),.UNSPECIFIED.);
#107=B_SPLINE_CURVE_WITH_KNOTS('',3,(#9912,#9913,#9914,#9915,#9916,#9917,
#9918,#9919,#9920,#9921,#9922,#9923,#9924,#9925,#9926,#9927,#9928,#9929,
#9930,#9931,#9932,#9933,#9934,#9935,#9936,#9937,#9938,#9939,#9940,#9941,
#9942,#9943,#9944,#9945,#9946,#9947,#9948,#9949,#9950,#9951,#9952,#9953,
#9954,#9955,#9956,#9957,#9958,#9959,#9960,#9961,#9962,#9963,#9964,#9965,
#9966,#9967,#9968,#9969,#9970,#9971,#9972,#9973,#9974,#9975,#9976,#9977,
#9978,#9979,#9980,#9981,#9982,#9983,#9984,#9985),.UNSPECIFIED.,.F.,.F.,
(4,2,2,2,2,2,2,2,2,2,2,2,2,2,2,2,2,2,2,2,2,2,2,2,2,2,2,2,2,2,2,2,2,2,2,
2,4),(-1.48451373067849,-1.46116924777296,-1.45808400850521,-1.45608651279479,
-1.45418536159507,-1.45271924820267,-1.45080623437103,-1.44744613437415,
-1.43053270847733,-1.41672089915974,-1.40406921364431,-1.40030111634928,
-1.39700628022729,-1.39597319077417,-1.39497744950135,-1.3940481350744,
-1.39292082845391,-1.39004286185665,-1.3665419218,-1.35023558159827,-1.34415285491573,
-1.339636031179,-1.33749038448044,-1.33584536069051,-1.33404771752278,-1.33112691416296,
-1.32146605515252,-1.28852098913718,-1.28327249887088,-1.27978201788845,
-1.27843091628103,-1.27748955484114,-1.27649574954126,-1.27489698996495,
-1.26993474313087,-1.26411590652247,-1.2428172115265),.UNSPECIFIED.);
#108=B_SPLINE_CURVE_WITH_KNOTS('',3,(#9986,#9987,#9988,#9989,#9990,#9991,
#9992,#9993,#9994,#9995,#9996,#9997,#9998,#9999,#10000,#10001,#10002,#10003,
#10004,#10005,#10006,#10007,#10008,#10009,#10010,#10011,#10012,#10013,#10014,
#10015,#10016,#10017,#10018,#10019,#10020,#10021,#10022,#10023,#10024,#10025,
#10026,#10027,#10028,#10029,#10030,#10031,#10032,#10033,#10034,#10035,#10036,
#10037,#10038,#10039,#10040,#10041,#10042,#10043,#10044,#10045,#10046,#10047,
#10048,#10049,#10050,#10051,#10052,#10053,#10054,#10055,#10056,#10057,#10058,
#10059,#10060,#10061,#10062,#10063,#10064,#10065,#10066,#10067,#10068,#10069,
#10070,#10071,#10072,#10073,#10074,#10075,#10076,#10077,#10078,#10079,#10080,
#10081,#10082,#10083,#10084,#10085,#10086,#10087,#10088,#10089,#10090,#10091,
#10092,#10093,#10094,#10095,#10096,#10097,#10098,#10099,#10100,#10101,#10102,
#10103,#10104,#10105,#10106,#10107,#10108,#10109,#10110,#10111,#10112,#10113,
#10114,#10115,#10116,#10117,#10118,#10119,#10120,#10121,#10122,#10123,#10124,
#10125,#10126,#10127,#10128,#10129,#10130,#10131,#10132,#10133,#10134,#10135,
#10136,#10137,#10138,#10139,#10140,#10141,#10142,#10143,#10144,#10145,#10146,
#10147,#10148,#10149,#10150,#10151,#10152,#10153,#10154,#10155,#10156,#10157,
#10158,#10159,#10160,#10161,#10162,#10163,#10164,#10165,#10166,#10167,#10168,
#10169,#10170,#10171,#10172,#10173,#10174,#10175,#10176,#10177,#10178,#10179,
#10180,#10181,#10182,#10183,#10184,#10185,#10186,#10187,#10188,#10189,#10190,
#10191,#10192,#10193,#10194,#10195,#10196,#10197,#10198,#10199,#10200,#10201,
#10202,#10203,#10204,#10205),.UNSPECIFIED.,.F.,.F.,(4,2,2,2,2,2,2,2,2,2,
2,2,2,2,2,2,2,2,2,2,2,2,2,2,2,2,2,2,2,2,2,2,2,2,2,2,2,2,2,2,2,2,2,2,2,2,
2,2,2,2,2,2,2,2,2,2,2,2,2,2,2,2,2,2,2,2,2,2,2,2,2,2,2,2,2,2,2,2,2,2,2,2,
2,2,2,2,2,2,2,2,2,2,2,2,2,2,2,2,2,2,2,2,2,2,2,2,2,2,2,4),(-0.98405823001278,
-0.97400707104787,-0.970751322952857,-0.968880890719665,-0.967249229774399,
-0.965227678577384,-0.962104716522352,-0.939450532390953,-0.921932922739935,
-0.915825427897057,-0.911926867132361,-0.910516773785427,-0.909563886051716,
-0.908704363146824,-0.907517937650744,-0.904492041117516,-0.886581067929002,
-0.866411828836706,-0.856074473085999,-0.853191341938306,-0.851401969544046,
-0.849754583930772,-0.847627889181588,-0.842978227434208,-0.819043668860734,
-0.80509198424679,-0.798741802913096,-0.794732412670994,-0.793307140818024,
-0.79235111324414,-0.791494301057696,-0.790318609442775,-0.787356942735387,
-0.766542008679358,-0.742504085515605,-0.737493007348105,-0.735445218903251,
-0.733919759220508,-0.732243893297746,-0.729908190212917,-0.724164738818813,
-0.715899240907171,-0.684546126543545,-0.678130409343872,-0.676376224410512,
-0.675348101217621,-0.674421673710567,-0.673157589418741,-0.670206343020052,
-0.666013420097018,-0.65365123238517,-0.623883897872317,-0.619660189745749,
-0.617590579403002,-0.615954629787558,-0.61411595003376,-0.611006985416679,
-0.597680316716895,-0.581319613680652,-0.562970119972712,-0.559962101353089,
-0.558778623782255,-0.557919816092369,-0.556965997793481,-0.555551602359039,
-0.551622239650024,-0.545448648603113,-0.528082323631822,-0.505406498411675,
-0.502283657914997,-0.500262058696316,-0.498630289203212,-0.496759655680116,
-0.493503366136088,-0.477471835743734,-0.463039274916872,-0.454546891360892,
-0.444127690341879,-0.442304698911643,-0.441154460790533,-0.44023989927412,
-0.43913912072516,-0.437047306200743,-0.421363876621889,-0.396387746483833,
-0.387091702409179,-0.384210585859698,-0.382421631112915,-0.380774073440092,
-0.378609853130598,-0.373881191013549,-0.367492570217147,-0.349747903971835,
-0.328406998548195,-0.325467766644331,-0.32429582771276,-0.323439933769897,
-0.322482705334922,-0.321051815983408,-0.31700089942774,-0.310559623129661,
-0.293496097450313,-0.270949680337322,-0.267824464950883,-0.265802168162892,
-0.264170380648203,-0.262300324195541,-0.259046589473324,-0.243068950388722,
-0.242040300785714),.UNSPECIFIED.);
#109=B_SPLINE_CURVE_WITH_KNOTS('',3,(#10210,#10211,#10212,#10213,#10214,
#10215,#10216,#10217,#10218,#10219,#10220,#10221,#10222,#10223,#10224,#10225,
#10226,#10227,#10228,#10229,#10230,#10231,#10232,#10233,#10234,#10235,#10236,
#10237,#10238,#10239,#10240,#10241,#10242,#10243,#10244,#10245,#10246,#10247,
#10248,#10249,#10250,#10251,#10252,#10253,#10254,#10255,#10256,#10257,#10258,
#10259,#10260,#10261,#10262,#10263,#10264,#10265,#10266,#10267,#10268,#10269,
#10270,#10271,#10272,#10273,#10274,#10275,#10276,#10277,#10278,#10279,#10280,
#10281,#10282,#10283,#10284,#10285,#10286,#10287,#10288,#10289,#10290,#10291,
#10292,#10293,#10294,#10295,#10296,#10297,#10298,#10299,#10300,#10301,#10302,
#10303,#10304,#10305,#10306,#10307,#10308,#10309,#10310,#10311,#10312,#10313,
#10314,#10315,#10316,#10317,#10318,#10319,#10320,#10321,#10322,#10323,#10324,
#10325,#10326,#10327,#10328,#10329,#10330,#10331,#10332,#10333,#10334,#10335,
#10336,#10337,#10338,#10339,#10340,#10341,#10342,#10343,#10344,#10345,#10346,
#10347,#10348,#10349,#10350,#10351,#10352,#10353,#10354,#10355,#10356,#10357,
#10358,#10359,#10360,#10361,#10362,#10363,#10364,#10365,#10366,#10367,#10368,
#10369,#10370,#10371,#10372,#10373,#10374,#10375,#10376,#10377,#10378,#10379,
#10380,#10381,#10382,#10383,#10384,#10385,#10386,#10387,#10388,#10389,#10390,
#10391,#10392,#10393,#10394,#10395,#10396,#10397,#10398,#10399,#10400,#10401,
#10402,#10403,#10404,#10405,#10406,#10407,#10408,#10409,#10410,#10411,#10412,
#10413,#10414,#10415,#10416,#10417,#10418,#10419),.UNSPECIFIED.,.F.,.F.,
(4,2,2,2,2,2,2,2,2,2,2,2,2,2,2,2,2,2,2,2,2,2,2,2,2,2,2,2,2,2,2,2,2,2,2,
2,2,2,2,2,2,2,2,2,2,2,2,2,2,2,2,2,2,2,2,2,2,2,2,2,2,2,2,2,2,2,2,2,2,2,2,
2,2,2,2,2,2,2,2,2,2,2,2,2,2,2,2,2,2,2,2,2,2,2,2,2,2,2,2,2,2,2,2,2,4),(-1.24265200671274,
-1.22719957996762,-1.21800259183579,-1.20382165019046,-1.20176176771288,
-1.20066777501492,-1.19975295499178,-1.19859491083029,-1.19674574147489,
-1.19527393431518,-1.17407659103393,-1.1562619318333,-1.14985971710055,
-1.14512306508982,-1.14295754968399,-1.14130994991724,-1.139521864745,-1.13664417352646,
-1.12737883775365,-1.10236807716455,-1.0866709045022,-1.0845788593499,-1.08347809206551,
-1.08256360919259,-1.08141354901745,-1.0795909959997,-1.06917604326802,
-1.0606999415883,-1.04629040673359,-1.03025647923327,-1.02700050579771,
-1.02513003986385,-1.02349840154925,-1.02147694157929,-1.01835423119893,
-0.995658223040673,-0.97825456008128,-0.972107808314153,-0.968191255742003,
-0.966778688550653,-0.965825300982004,-0.964966239807481,-0.963781601828935,
-0.960766223140326,-0.942700796067431,-0.923326769326904,-0.912437615006063,
-0.909506902339477,-0.907707169076331,-0.906062861392199,-0.903957612653297,
-0.899425656055709,-0.87279334065823,-0.866955856400763,-0.856875298955461,
-0.851370175331793,-0.849770420736875,-0.848776496300703,-0.847846239855462,
-0.846715056964892,-0.843927777383174,-0.819514641309596,-0.803793839945378,
-0.797842212731947,-0.793364258774201,-0.791246225694342,-0.789604830855865,
-0.787793527369268,-0.784809967171913,-0.774545218488185,-0.742269625666963,
-0.73460858950906,-0.732772356677799,-0.731715454356179,-0.73088818939534,
-0.729728816690724,-0.727348157480081,-0.72417946655417,-0.716214982995178,
-0.692714662962205,-0.678601259858895,-0.675369880401874,-0.673485803329206,
-0.672018143879595,-0.670085991925144,-0.66654187774207,-0.641493766653995,
-0.619098326283343,-0.616205651112152,-0.615041527318315,-0.614102649424678,
-0.613122203160549,-0.611584194157185,-0.606661724495914,-0.598144730113181,
-0.572290524813978,-0.560994513900779,-0.557917033245088,-0.55608507410508,
-0.554447719210809,-0.552366265779187,-0.548082007112975,-0.531634463220765,
-0.506056827056548,-0.500712197120109),.UNSPECIFIED.);
#110=B_SPLINE_CURVE_WITH_KNOTS('',3,(#10421,#10422,#10423,#10424,#10425,
#10426,#10427,#10428,#10429,#10430,#10431,#10432,#10433,#10434,#10435,#10436,
#10437,#10438,#10439,#10440,#10441,#10442,#10443,#10444,#10445,#10446,#10447,
#10448,#10449,#10450,#10451,#10452,#10453,#10454,#10455,#10456,#10457,#10458,
#10459,#10460,#10461,#10462,#10463,#10464,#10465,#10466,#10467,#10468,#10469,
#10470,#10471,#10472,#10473,#10474,#10475,#10476,#10477,#10478,#10479,#10480,
#10481,#10482,#10483,#10484,#10485,#10486,#10487,#10488,#10489,#10490,#10491,
#10492),.UNSPECIFIED.,.F.,.F.,(4,2,2,2,2,2,2,2,2,2,2,2,2,2,2,2,2,2,2,2,
2,2,2,2,2,2,2,2,2,2,2,2,2,2,2,4),(-0.242040300785714,-0.228597739999477,
-0.220089037302706,-0.20966768651593,-0.207844639056614,-0.206694397094238,
-0.205779854275758,-0.204679124381012,-0.202587473559587,-0.18691084659806,
-0.161955516755339,-0.152637453339446,-0.149754055762204,-0.147964629307045,
-0.14631726825784,-0.144281346116536,-0.139914405248792,-0.134089246407373,
-0.118917821650194,-0.0939154634649374,-0.0909957444604389,-0.0898271140801679,
-0.0889720410306897,-0.0880137787955856,-0.0870372998373829,-0.0843343282204052,
-0.071989764230856,-0.0545185270730589,-0.0364418201534302,-0.033342502060549,
-0.0313280574066432,-0.0296967933063195,-0.0278209284362617,-0.0258592177881634,
-0.0228608516323196,-0.000340552445936415),.UNSPECIFIED.);
#111=B_SPLINE_CURVE_WITH_KNOTS('',3,(#10493,#10494,#10495,#10496,#10497,
#10498,#10499,#10500,#10501,#10502,#10503,#10504,#10505,#10506,#10507,#10508,
#10509,#10510,#10511,#10512,#10513,#10514,#10515,#10516,#10517,#10518,#10519,
#10520,#10521,#10522,#10523,#10524,#10525,#10526,#10527,#10528,#10529,#10530,
#10531,#10532,#10533,#10534,#10535,#10536,#10537,#10538,#10539,#10540,#10541,
#10542,#10543,#10544,#10545,#10546,#10547,#10548,#10549,#10550,#10551,#10552,
#10553,#10554,#10555,#10556,#10557,#10558,#10559,#10560,#10561,#10562,#10563,
#10564,#10565,#10566,#10567,#10568,#10569,#10570,#10571,#10572,#10573,#10574,
#10575,#10576,#10577,#10578,#10579,#10580,#10581,#10582,#10583,#10584,#10585,
#10586,#10587,#10588,#10589,#10590,#10591,#10592,#10593,#10594,#10595,#10596,
#10597,#10598,#10599,#10600,#10601,#10602,#10603,#10604,#10605,#10606,#10607,
#10608,#10609,#10610,#10611,#10612,#10613,#10614,#10615,#10616,#10617,#10618,
#10619,#10620,#10621,#10622,#10623,#10624,#10625,#10626,#10627,#10628,#10629,
#10630,#10631,#10632,#10633,#10634,#10635,#10636,#10637,#10638,#10639,#10640,
#10641,#10642),.UNSPECIFIED.,.F.,.F.,(4,2,2,2,2,2,2,2,2,2,2,2,2,2,2,2,2,
2,2,2,2,2,2,2,2,2,2,2,2,2,2,2,2,2,2,2,2,2,2,2,2,2,2,2,2,2,2,2,2,2,2,2,2,
2,2,2,2,2,2,2,2,2,2,2,2,2,2,2,2,2,2,2,2,2,4),(-1.48450003793453,-1.46287590279009,
-1.45982402878966,-1.45818847912071,-1.45677398097135,-1.45582014616151,
-1.45496135988593,-1.4537779697734,-1.45077043850895,-1.43245112533197,
-1.41332429557885,-1.4024311153063,-1.39961975102648,-1.39778822759921,
-1.39615100963953,-1.39406938960619,-1.38978357236929,-1.36164388380195,
-1.34813055164141,-1.34370901783773,-1.34066777723663,-1.33937093337936,
-1.33843931368745,-1.33742568729945,-1.33573713892179,-1.32998390352211,
-1.30409417468053,-1.28751148795387,-1.2832099247477,-1.28112528423152,
-1.27948773869952,-1.27765797570941,-1.27459000701043,-1.26341572476417,
-1.23742564777199,-1.22888554065074,-1.22395449314357,-1.22241558919221,
-1.2214350084424,-1.22049637956714,-1.21933298815086,-1.21644421135776,
-1.19402388573959,-1.17701973658039,-1.17078551762507,-1.16614436730831,
-1.16399596271834,-1.16235047137383,-1.16055394673447,-1.15763864382601,
-1.14803077950044,-1.12043803744325,-1.11171861793898,-1.10671770284436,
-1.10517095094971,-1.10418860508198,-1.10325107886563,-1.10209198800552,
-1.09922845709034,-1.07647851393198,-1.05968089198163,-1.05349064870514,
-1.04887464056812,-1.04673076625755,-1.04508579964447,-1.04328693390141,
-1.04036124690405,-1.03065755880463,-1.00601282647642,-0.990454733507967,
-0.988364718932059,-0.987264194398857,-0.986349438227163,-0.985198449752847,
-0.984126425382023),.UNSPECIFIED.);
#112=B_SPLINE_CURVE_WITH_KNOTS('',3,(#10648,#10649,#10650,#10651,#10652,
#10653,#10654,#10655,#10656,#10657,#10658,#10659,#10660,#10661,#10662,#10663,
#10664,#10665,#10666,#10667,#10668,#10669,#10670,#10671,#10672,#10673,#10674,
#10675,#10676,#10677,#10678,#10679,#10680,#10681,#10682,#10683,#10684,#10685,
#10686,#10687,#10688,#10689,#10690,#10691,#10692,#10693,#10694,#10695,#10696,
#10697,#10698,#10699,#10700,#10701,#10702,#10703,#10704,#10705,#10706,#10707,
#10708,#10709,#10710,#10711,#10712,#10713,#10714,#10715,#10716,#10717,#10718,
#10719,#10720,#10721,#10722,#10723,#10724,#10725,#10726,#10727,#10728,#10729,
#10730,#10731,#10732,#10733,#10734,#10735,#10736,#10737,#10738,#10739,#10740,
#10741,#10742,#10743,#10744,#10745,#10746,#10747,#10748,#10749,#10750,#10751,
#10752,#10753,#10754,#10755,#10756,#10757,#10758,#10759,#10760,#10761,#10762,
#10763,#10764,#10765,#10766,#10767,#10768,#10769,#10770,#10771,#10772,#10773,
#10774,#10775,#10776,#10777,#10778,#10779,#10780,#10781,#10782,#10783,#10784,
#10785,#10786,#10787,#10788,#10789,#10790,#10791,#10792,#10793,#10794,#10795,
#10796,#10797,#10798,#10799,#10800,#10801,#10802,#10803,#10804,#10805),
 .UNSPECIFIED.,.F.,.F.,(4,2,2,2,2,2,2,2,2,2,2,2,2,2,2,2,2,2,2,2,2,2,2,2,
2,2,2,2,2,2,2,2,2,2,2,2,2,2,2,2,2,2,2,2,2,2,2,2,2,2,2,2,2,2,2,2,2,2,2,2,
2,2,2,2,2,2,2,2,2,2,2,2,2,2,2,2,2,2,4),(-0.500854930573822,-0.486075548964709,
-0.481734828916494,-0.479642564627619,-0.478004024270296,-0.476178306202764,
-0.47312945105295,-0.460706260795896,-0.429924054507328,-0.422952536531026,
-0.421148758649097,-0.420109613554019,-0.419186103588324,-0.417943400011714,
-0.415115777483494,-0.40224200702912,-0.393704480343706,-0.36926014305392,
-0.364625685841479,-0.362501381634948,-0.360853960802749,-0.359062657667822,
-0.356172200613966,-0.345758949958123,-0.325315360564438,-0.317751558646107,
-0.312660167920223,-0.305710990210885,-0.303909110442994,-0.302870381811186,
-0.301946764313685,-0.300703268918895,-0.297871159456327,-0.284954985031877,
-0.276059760720306,-0.252042212729601,-0.247395002600144,-0.245268388807385,
-0.243620626473954,-0.241830402803363,-0.238944913963799,-0.228587769603937,
-0.208349904171972,-0.190477443323002,-0.187464749125807,-0.186280330461392,
-0.185421147783713,-0.18446727661304,-0.183053408682288,-0.179129394696484,
-0.172967935187127,-0.155586796920719,-0.132903481814581,-0.129779761096779,
-0.127757635343345,-0.126203544961513,-0.124402424605798,-0.122501968967435,
-0.119652995467467,-0.114423204676567,-0.101655907336608,-0.0830142693867631,
-0.0787861475531215,-0.071306942697782,-0.0694837304140167,-0.0684297112479054,
-0.0676018237803621,-0.0664378360264485,-0.0640341176443245,-0.0608259398031352,
-0.0527118768185914,-0.0229576793455864,-0.0143961687149711,-0.0115987725285022,
-0.00982773786947007,-0.00825972761001749,-0.00665241883828211,-0.00386429324692953,
-0.000340360607640195),.UNSPECIFIED.);
#113=B_SPLINE_CURVE_WITH_KNOTS('',3,(#10806,#10807,#10808,#10809,#10810,
#10811,#10812,#10813,#10814,#10815,#10816,#10817,#10818,#10819,#10820,#10821,
#10822,#10823,#10824,#10825,#10826,#10827,#10828,#10829,#10830,#10831,#10832,
#10833,#10834,#10835,#10836,#10837,#10838,#10839,#10840,#10841,#10842,#10843,
#10844,#10845,#10846,#10847,#10848,#10849,#10850,#10851,#10852,#10853,#10854,
#10855,#10856,#10857,#10858,#10859,#10860,#10861,#10862,#10863,#10864,#10865,
#10866,#10867,#10868,#10869,#10870,#10871,#10872,#10873,#10874,#10875,#10876,
#10877,#10878,#10879,#10880,#10881,#10882,#10883,#10884,#10885,#10886,#10887,
#10888,#10889,#10890,#10891,#10892,#10893,#10894,#10895,#10896,#10897,#10898,
#10899,#10900,#10901,#10902,#10903,#10904,#10905,#10906,#10907),
 .UNSPECIFIED.,.F.,.F.,(4,2,2,2,2,2,2,2,2,2,2,2,2,2,2,2,2,2,2,2,2,2,2,2,
2,2,2,2,2,2,2,2,2,2,2,2,2,2,2,2,2,2,2,2,2,2,2,2,2,2,4),(-1.48415514651379,
-1.45149920551291,-1.44244211629787,-1.43731255766761,-1.43575204220037,
-1.43476685356475,-1.433831635031,-1.43246270329097,-1.42986122343986,-1.4061924457234,
-1.38541357703921,-1.38163060098673,-1.37934788511961,-1.37731925181912,
-1.3772983125346,-1.37727586732553,-1.37725174788944,-1.37722575916579,
-1.37719767368199,-1.37716722436655,-1.37713409534207,-1.37709790995652,
-1.37705821505763,-1.37701446000724,-1.37696596824716,-1.37691189805811,
-1.37685118732537,-1.37678247397149,-1.37674965215004,-1.37667856265869,
-1.37508854787638,-1.37306558233999,-1.36993756341773,-1.34725092169245,
-1.32984167098033,-1.3237024152774,-1.31978941393382,-1.31837742282627,
-1.31742421890925,-1.31656516220981,-1.31538032592114,-1.31236334101688,
-1.29433178935098,-1.27425428314318,-1.26394326012941,-1.26106272044498,
-1.25927404078754,-1.25762667722671,-1.25549914243146,-1.25084401886462,
-1.24265200671274),.UNSPECIFIED.);
#114=B_SPLINE_CURVE_WITH_KNOTS('',3,(#10908,#10909,#10910,#10911,#10912,
#10913,#10914,#10915,#10916,#10917,#10918,#10919,#10920,#10921,#10922,#10923,
#10924,#10925,#10926,#10927,#10928,#10929,#10930,#10931,#10932,#10933,#10934,
#10935,#10936,#10937,#10938,#10939,#10940,#10941,#10942,#10943,#10944,#10945,
#10946,#10947,#10948,#10949,#10950,#10951,#10952,#10953,#10954,#10955,#10956,
#10957,#10958,#10959,#10960,#10961,#10962,#10963,#10964,#10965,#10966,#10967,
#10968,#10969,#10970,#10971,#10972,#10973,#10974,#10975,#10976,#10977,#10978,
#10979,#10980,#10981,#10982,#10983,#10984,#10985,#10986,#10987,#10988,#10989,
#10990,#10991,#10992,#10993,#10994,#10995,#10996,#10997,#10998,#10999,#11000,
#11001,#11002,#11003,#11004,#11005,#11006,#11007,#11008,#11009,#11010,#11011,
#11012,#11013,#11014,#11015,#11016,#11017,#11018,#11019,#11020,#11021,#11022,
#11023,#11024,#11025,#11026,#11027,#11028,#11029,#11030,#11031,#11032,#11033,
#11034,#11035,#11036,#11037,#11038,#11039,#11040,#11041,#11042,#11043,#11044,
#11045,#11046,#11047,#11048,#11049,#11050,#11051,#11052,#11053,#11054,#11055,
#11056,#11057,#11058,#11059,#11060,#11061,#11062,#11063,#11064,#11065,#11066,
#11067,#11068,#11069,#11070,#11071,#11072,#11073,#11074,#11075,#11076,#11077,
#11078,#11079,#11080,#11081,#11082,#11083,#11084,#11085,#11086,#11087,#11088,
#11089,#11090,#11091,#11092,#11093,#11094,#11095,#11096,#11097,#11098,#11099,
#11100,#11101,#11102,#11103,#11104,#11105,#11106,#11107,#11108,#11109,#11110,
#11111,#11112,#11113,#11114,#11115,#11116,#11117),.UNSPECIFIED.,.F.,.F.,
(4,2,2,2,2,2,2,2,2,2,2,2,2,2,2,2,2,2,2,2,2,2,2,2,2,2,2,2,2,2,2,2,2,2,2,
2,2,2,2,2,2,2,2,2,2,2,2,2,2,2,2,2,2,2,2,2,2,2,2,2,2,2,2,2,2,2,2,2,2,2,2,
2,2,2,2,2,2,2,2,2,2,2,2,2,2,2,2,2,2,2,2,2,2,2,2,2,2,2,2,2,2,2,2,2,4),(-0.984126425382023,
-0.983373365694033,-0.972905881216294,-0.96440508188655,-0.944486287465323,
-0.933431938592775,-0.930487001827596,-0.928683873097357,-0.92703995418775,
-0.924940004467587,-0.920438620203604,-0.893336752663696,-0.873797532864454,
-0.871327513572878,-0.870150693646636,-0.869234327455437,-0.868154122712197,
-0.86621562404796,-0.856915362097018,-0.837265444012163,-0.820172839227312,
-0.814728758241953,-0.812440769945779,-0.810773058499702,-0.809236966256497,
-0.807147299654878,-0.802985899498695,-0.778077028674095,-0.770491729308653,
-0.757142158191999,-0.754264791825363,-0.753013336330303,-0.752088605896066,
-0.751053954240847,-0.749270710216774,-0.742536657701058,-0.728157707544133,
-0.701569538465855,-0.6970339008539,-0.694927624767163,-0.69328279890119,
-0.691482791774579,-0.688552312985616,-0.677673742852565,-0.658340794028179,
-0.64016692608942,-0.637153807938739,-0.635969333996813,-0.635110150305577,
-0.634156332939673,-0.632742651598299,-0.628819870039803,-0.62266115183107,
-0.605273799859729,-0.5825841984773,-0.579460660601513,-0.577438613171592,
-0.575806484002945,-0.573935440464655,-0.570678443187492,-0.554643588932069,
-0.540207700435531,-0.531713365710718,-0.521291872639942,-0.519468479745616,
-0.51831798827299,-0.517403225285627,-0.516302204207945,-0.514209928708041,
-0.498523035351526,-0.473541380321435,-0.464243314699706,-0.46136156623328,
-0.459572217995092,-0.457924297183967,-0.455759598764231,-0.451029887520897,
-0.444639846263575,-0.426891207045569,-0.405545692995482,-0.402605810537817,
-0.401433612918007,-0.400577530298193,-0.399620091151593,-0.398188887347618,
-0.394137084093678,-0.387694401476146,-0.370627114237207,-0.348075710368098,
-0.344949807772665,-0.342927065866851,-0.341294918907402,-0.339424450217873,
-0.336169997443571,-0.320188811190221,-0.305714433171593,-0.29720386249206,
-0.286780218720869,-0.284956769767485,-0.283806274447871,-0.282891530162832,
-0.28179055775546,-0.279698446018787,-0.264018358063324,-0.241971004323415),
 .UNSPECIFIED.);
#115=B_SPLINE_CURVE_WITH_KNOTS('',3,(#11122,#11123,#11124,#11125,#11126,
#11127,#11128,#11129,#11130,#11131,#11132,#11133,#11134,#11135,#11136,#11137,
#11138,#11139,#11140,#11141,#11142,#11143,#11144,#11145,#11146,#11147,#11148,
#11149,#11150,#11151,#11152,#11153,#11154,#11155,#11156,#11157,#11158,#11159,
#11160,#11161,#11162,#11163,#11164,#11165,#11166,#11167,#11168,#11169,#11170,
#11171,#11172,#11173,#11174,#11175,#11176,#11177,#11178,#11179,#11180,#11181,
#11182,#11183,#11184,#11185,#11186,#11187,#11188,#11189,#11190,#11191,#11192,
#11193,#11194,#11195,#11196,#11197,#11198,#11199,#11200,#11201,#11202,#11203,
#11204,#11205,#11206,#11207,#11208,#11209,#11210,#11211,#11212,#11213,#11214,
#11215,#11216,#11217,#11218,#11219,#11220,#11221,#11222,#11223,#11224,#11225,
#11226,#11227,#11228,#11229,#11230,#11231,#11232,#11233,#11234,#11235,#11236,
#11237,#11238,#11239,#11240,#11241,#11242,#11243,#11244,#11245,#11246,#11247,
#11248,#11249,#11250,#11251,#11252,#11253,#11254,#11255,#11256,#11257,#11258,
#11259,#11260,#11261,#11262,#11263,#11264,#11265,#11266,#11267,#11268,#11269,
#11270,#11271,#11272,#11273,#11274,#11275,#11276,#11277,#11278,#11279,#11280,
#11281,#11282,#11283,#11284,#11285,#11286,#11287,#11288,#11289,#11290,#11291,
#11292,#11293,#11294,#11295,#11296,#11297,#11298,#11299,#11300,#11301,#11302,
#11303,#11304,#11305,#11306,#11307,#11308,#11309,#11310,#11311,#11312,#11313,
#11314,#11315,#11316,#11317,#11318,#11319,#11320,#11321,#11322,#11323,#11324,
#11325,#11326,#11327,#11328,#11329,#11330,#11331,#11332,#11333,#11334,#11335,
#11336,#11337),.UNSPECIFIED.,.F.,.F.,(4,2,2,2,2,2,2,2,2,2,2,2,2,2,2,2,2,
2,2,2,2,2,2,2,2,2,2,2,2,2,2,2,2,2,2,2,2,2,2,2,2,2,2,2,2,2,2,2,2,2,2,2,2,
2,2,2,2,2,2,2,2,2,2,2,2,2,2,2,2,2,2,2,2,2,2,2,2,2,2,2,2,2,2,2,2,2,2,2,2,
2,2,2,2,2,2,2,2,2,2,2,2,2,2,2,2,2,2,4),(-1.24288726449128,-1.24163342877597,
-1.24065148247496,-1.23971399027183,-1.23855456628014,-1.23568835295016,
-1.21300160884336,-1.19617494378115,-1.18997916861392,-1.18536022569125,
-1.18321606753075,-1.18157132481516,-1.17977313763682,-1.17684952619924,
-1.16716146154078,-1.13631403244112,-1.12979850884176,-1.12571465366471,
-1.12427931995828,-1.12332113562735,-1.12246593316861,-1.12129687952411,
-1.11834450385232,-1.09713198867436,-1.08891161571426,-1.07227074593167,
-1.06796179849435,-1.06587571137707,-1.06423796846684,-1.06240895519245,
-1.0593445658533,-1.04821575680757,-1.02477530920776,-1.00970577855156,
-1.00762561154606,-1.00652721495725,-1.00561244168765,-1.0044591642126,
-1.00262628343159,-0.991958228061934,-0.98392943416366,-0.963130008609321,
-0.956165846235589,-0.951114761823736,-0.948893279039927,-0.947236904566019,
-0.945684622485903,-0.94310382069536,-0.936219008662551,-0.905685438203178,
-0.896642236282482,-0.893197693911649,-0.890658404777163,-0.889468444510046,
-0.888559318249259,-0.887491966658089,-0.885610059085682,-0.877271087301634,
-0.847860136594266,-0.835620927876824,-0.832585251292835,-0.830762428581112,
-0.829123335681778,-0.827026007287135,-0.822658622109339,-0.794113753893987,
-0.789047536182051,-0.779575591033752,-0.774290458738673,-0.772713091474382,
-0.771723993276586,-0.77079071192917,-0.769433081074306,-0.76687557349804,
-0.742576440167406,-0.719163860961597,-0.716031534274363,-0.714006938726207,
-0.71237478398984,-0.710505931928709,-0.707258487523441,-0.691420629244765,
-0.667199684751267,-0.657762157472976,-0.655816397579372,-0.654734615219692,
-0.653818485833921,-0.652643990423514,-0.650185746470363,-0.646883203323154,
-0.638404239760665,-0.612787283335558,-0.601233334434435,-0.598136504368191,
-0.596300303557412,-0.594827344822309,-0.592833235264844,-0.588990277410438,
-0.569376559148978,-0.549534964027653,-0.540486204516383,-0.538561582925485,
-0.5374845601196,-0.536567924843716,-0.535386922748773,-0.53289477986775,
-0.514846765038427,-0.500854930573822),.UNSPECIFIED.);
#116=B_SPLINE_CURVE_WITH_KNOTS('',3,(#11339,#11340,#11341,#11342,#11343,
#11344,#11345,#11346,#11347,#11348,#11349,#11350,#11351,#11352,#11353,#11354,
#11355,#11356,#11357,#11358,#11359,#11360,#11361,#11362,#11363,#11364,#11365,
#11366,#11367,#11368,#11369,#11370,#11371,#11372,#11373,#11374,#11375,#11376,
#11377,#11378,#11379,#11380,#11381,#11382,#11383,#11384,#11385,#11386,#11387,
#11388,#11389,#11390,#11391,#11392,#11393,#11394,#11395,#11396,#11397,#11398,
#11399,#11400,#11401,#11402,#11403,#11404,#11405,#11406,#11407,#11408,#11409,
#11410,#11411,#11412,#11413,#11414),.UNSPECIFIED.,.F.,.F.,(4,2,2,2,2,2,
2,2,2,2,2,2,2,2,2,2,2,2,2,2,2,2,2,2,2,2,2,2,2,2,2,2,2,2,2,2,2,4),(-0.241971004323415,
-0.239053971418212,-0.229736799381529,-0.22685307708173,-0.22506332408183,
-0.22341557890168,-0.221251912997029,-0.216527745168172,-0.210147422237314,
-0.192445910058425,-0.171033428826221,-0.168085358638406,-0.166917316565231,
-0.166062277525162,-0.165103567731153,-0.163666241889273,-0.159568416394568,
-0.153023023648686,-0.121691640522961,-0.11244487918447,-0.109568666996894,
-0.107780600902137,-0.106201075113282,-0.106181872856666,-0.104141339135245,
-0.10185902694292,-0.0980775006358801,-0.0902103746626518,-0.076223358344637,
-0.0536758840913093,-0.0507959511513297,-0.0496340231114811,-0.0486957404565197,
-0.0477144793902815,-0.0461727153274274,-0.041216633357305,-0.0326138141010124,
-0.000340852960060052),.UNSPECIFIED.);
#117=B_SPLINE_CURVE_WITH_KNOTS('',3,(#11415,#11416,#11417,#11418,#11419,
#11420,#11421,#11422,#11423,#11424,#11425,#11426,#11427,#11428,#11429,#11430,
#11431,#11432,#11433,#11434,#11435,#11436,#11437,#11438,#11439,#11440,#11441,
#11442,#11443,#11444,#11445,#11446,#11447,#11448,#11449,#11450,#11451,#11452,
#11453,#11454,#11455,#11456,#11457,#11458,#11459,#11460,#11461,#11462,#11463,
#11464,#11465,#11466,#11467,#11468,#11469,#11470,#11471,#11472,#11473,#11474,
#11475,#11476,#11477,#11478,#11479,#11480,#11481,#11482,#11483,#11484,#11485,
#11486,#11487,#11488,#11489,#11490,#11491,#11492,#11493,#11494,#11495,#11496,
#11497,#11498,#11499,#11500,#11501,#11502,#11503,#11504,#11505,#11506,#11507,
#11508,#11509,#11510,#11511,#11512,#11513,#11514,#11515,#11516,#11517,#11518,
#11519,#11520,#11521,#11522,#11523,#11524,#11525,#11526,#11527,#11528,#11529,
#11530,#11531,#11532,#11533,#11534,#11535,#11536,#11537,#11538,#11539,#11540,
#11541,#11542,#11543,#11544,#11545,#11546,#11547,#11548,#11549,#11550,#11551,
#11552,#11553,#11554,#11555,#11556,#11557,#11558,#11559,#11560,#11561,#11562,
#11563,#11564,#11565,#11566,#11567,#11568,#11569,#11570),.UNSPECIFIED.,
 .F.,.F.,(4,2,2,2,2,2,2,2,2,2,2,2,2,2,2,2,2,2,2,2,2,2,2,2,2,2,2,2,2,2,2,
2,2,2,2,2,2,2,2,2,2,2,2,2,2,2,2,2,2,2,2,2,2,2,2,2,2,2,2,2,2,2,2,2,2,2,2,
2,2,2,2,2,2,2,2,2,2,4),(-1.48431280040011,-1.47896056546552,-1.47689292482486,
-1.47529572669305,-1.47371992892605,-1.47193220443593,-1.46905506899411,
-1.45978888255018,-1.43819039265586,-1.42492169717083,-1.42054823772937,
-1.4175020382775,-1.41622215306785,-1.41529358812556,-1.41427335838495,
-1.41255378430918,-1.40649295880256,-1.38450574218668,-1.37007018954134,
-1.36442059579054,-1.36141528466624,-1.35945096227819,-1.35805699629727,
-1.3564493497163,-1.35463627557722,-1.35164285402985,-1.34126858027713,
-1.31117265327994,-1.30470819826332,-1.30064753724468,-1.29921556738997,
-1.29825828937859,-1.2974028668826,-1.29623223184307,-1.29329962648975,
-1.27178996015631,-1.25418919766581,-1.2478309444976,-1.24311937298221,
-1.24095856523215,-1.23931180718429,-1.23752196386011,-1.23463551625966,
-1.22528507866461,-1.19406517724991,-1.18752623024879,-1.18343208354017,
-1.18199556015604,-1.18103726039389,-1.1801824852927,-1.17901468807528,
-1.17606736578505,-1.15471040666525,-1.13700043088882,-1.13061945590468,
-1.12589485831694,-1.12373155754217,-1.12208431203236,-1.12029531728363,
-1.11741330022025,-1.10810671568076,-1.0831269318708,-1.06744091024756,
-1.06534906821887,-1.06424836164924,-1.06333390643313,-1.06218386598269,
-1.06036132482472,-1.04994657472771,-1.04146389337108,-1.02704592886333,
-1.01101876958153,-1.00776311751941,-1.00589275325785,-1.0042611590973,
-1.00223970033911,-0.999116899707024,-0.983965850740792),.UNSPECIFIED.);
#118=B_SPLINE_CURVE_WITH_KNOTS('',3,(#11576,#11577,#11578,#11579,#11580,
#11581,#11582,#11583,#11584,#11585,#11586,#11587,#11588,#11589,#11590,#11591,
#11592,#11593,#11594,#11595,#11596,#11597,#11598,#11599,#11600,#11601,#11602,
#11603,#11604,#11605,#11606,#11607,#11608,#11609,#11610,#11611,#11612,#11613,
#11614,#11615,#11616,#11617,#11618,#11619,#11620,#11621,#11622,#11623,#11624,
#11625,#11626,#11627,#11628,#11629,#11630,#11631,#11632,#11633,#11634,#11635,
#11636,#11637,#11638,#11639,#11640,#11641,#11642,#11643,#11644,#11645,#11646,
#11647,#11648,#11649,#11650,#11651,#11652,#11653,#11654,#11655,#11656,#11657,
#11658,#11659,#11660,#11661,#11662,#11663,#11664,#11665,#11666,#11667,#11668,
#11669,#11670,#11671,#11672,#11673,#11674,#11675,#11676,#11677,#11678,#11679,
#11680,#11681,#11682,#11683,#11684,#11685,#11686,#11687,#11688,#11689,#11690,
#11691,#11692,#11693,#11694,#11695,#11696,#11697,#11698,#11699,#11700,#11701,
#11702,#11703,#11704,#11705,#11706,#11707,#11708,#11709,#11710,#11711,#11712,
#11713,#11714,#11715,#11716,#11717,#11718,#11719),.UNSPECIFIED.,.F.,.F.,
(4,2,2,2,2,2,2,2,2,2,2,2,2,2,2,2,2,2,2,2,2,2,2,2,2,2,2,2,2,2,2,2,2,2,2,
2,2,2,2,2,2,2,2,2,2,2,2,2,2,2,2,2,2,2,2,2,2,2,2,2,2,2,2,2,2,2,2,2,2,2,2,
4),(-0.500801107159108,-0.496719065298586,-0.482294243553749,-0.473808490442153,
-0.463388293448443,-0.461565209675061,-0.460414906796204,-0.459500285784731,
-0.458399412973998,-0.456307344596265,-0.440613399579905,-0.415608457267786,
-0.40634982463576,-0.403472564478538,-0.401684376828063,-0.400036432618386,
-0.397870099126282,-0.39313018891593,-0.386721806429579,-0.368880059124788,
-0.347686747930129,-0.344731566857804,-0.343562416108004,-0.342707179701646,
-0.341748992382079,-0.340313724936937,-0.336230432660855,-0.329717053164425,
-0.298870969127536,-0.28919746513731,-0.286275355303111,-0.284477439454449,
-0.282832513660004,-0.280687496388851,-0.276064258498405,-0.269860370559074,
-0.252996759706132,-0.230336790507938,-0.22746686859608,-0.226306747010982,
-0.22536902236462,-0.224387225669904,-0.222842659074172,-0.217860248016697,
-0.209188959324149,-0.182095666929319,-0.172053928327316,-0.169090290863669,
-0.167283331368708,-0.165640858576464,-0.163514331183331,-0.158990961236074,
-0.152960381091844,-0.13688889987488,-0.112980279065176,-0.110135095017116,
-0.109012950430518,-0.108084887205651,-0.107106739772946,-0.105622849083686,
-0.10379912883353,-0.100231194655918,-0.0906818545504389,-0.0829888986598714,
-0.0575747013332469,-0.0530377262946375,-0.0508997778988846,-0.0492506615316133,
-0.0474663484896398,-0.0446066631603827,-0.0345296234097491,-0.000340926357595197),
 .UNSPECIFIED.);
#119=B_SPLINE_CURVE_WITH_KNOTS('',3,(#11720,#11721,#11722,#11723,#11724,
#11725,#11726,#11727,#11728,#11729,#11730,#11731,#11732,#11733,#11734,#11735,
#11736,#11737,#11738,#11739,#11740,#11741,#11742,#11743,#11744,#11745,#11746,
#11747,#11748,#11749,#11750,#11751,#11752,#11753,#11754,#11755,#11756,#11757,
#11758,#11759,#11760,#11761,#11762,#11763,#11764,#11765,#11766,#11767,#11768,
#11769,#11770,#11771,#11772,#11773,#11774,#11775,#11776,#11777,#11778,#11779,
#11780,#11781,#11782,#11783,#11784,#11785,#11786,#11787,#11788,#11789,#11790,
#11791,#11792,#11793,#11794,#11795,#11796,#11797),.UNSPECIFIED.,.F.,.F.,
(4,2,2,2,2,2,2,2,2,2,2,2,2,2,2,2,2,2,2,2,2,2,2,2,2,2,2,2,2,2,2,2,2,2,2,
2,2,2,4),(-1.48440949910283,-1.4781158042,-1.47680243786291,-1.47585385357628,
-1.47499593067532,-1.47413998146761,-1.47296752304019,-1.47001584976481,
-1.46266620479669,-1.43155466603343,-1.42484447046188,-1.41993456996183,
-1.41773818743503,-1.41608612565901,-1.4145273566791,-1.41191052624761,
-1.40476913271227,-1.37446864224158,-1.36550713048265,-1.36208323358632,
-1.36031134764514,-1.35882320203303,-1.35787181397324,-1.35693581026479,
-1.35578187816802,-1.35294711884787,-1.32977967194719,-1.31326405289154,
-1.30713574232963,-1.30255564838505,-1.30041873287133,-1.29877504491022,
-1.29697353758565,-1.29403436310168,-1.28420275305495,-1.25686630998966,
-1.24817035041627,-1.2431789305523,-1.24288726449128),.UNSPECIFIED.);
#120=B_SPLINE_CURVE_WITH_KNOTS('',3,(#11798,#11799,#11800,#11801,#11802,
#11803,#11804,#11805,#11806,#11807,#11808,#11809,#11810,#11811,#11812,#11813,
#11814,#11815,#11816,#11817,#11818,#11819,#11820,#11821,#11822,#11823,#11824,
#11825,#11826,#11827,#11828,#11829,#11830,#11831,#11832,#11833,#11834,#11835,
#11836,#11837,#11838,#11839,#11840,#11841,#11842,#11843,#11844,#11845,#11846,
#11847,#11848,#11849,#11850,#11851,#11852,#11853,#11854,#11855,#11856,#11857,
#11858,#11859,#11860,#11861,#11862,#11863,#11864,#11865,#11866,#11867,#11868,
#11869,#11870,#11871,#11872,#11873,#11874,#11875,#11876,#11877,#11878,#11879,
#11880,#11881,#11882,#11883,#11884,#11885,#11886,#11887,#11888,#11889,#11890,
#11891,#11892,#11893,#11894,#11895,#11896,#11897,#11898,#11899,#11900,#11901,
#11902,#11903,#11904,#11905,#11906,#11907,#11908,#11909,#11910,#11911,#11912,
#11913,#11914,#11915,#11916,#11917,#11918,#11919,#11920,#11921,#11922,#11923,
#11924,#11925,#11926,#11927,#11928,#11929,#11930,#11931,#11932,#11933,#11934,
#11935,#11936,#11937,#11938,#11939,#11940,#11941,#11942,#11943,#11944,#11945,
#11946,#11947,#11948,#11949,#11950,#11951,#11952,#11953,#11954,#11955,#11956,
#11957,#11958,#11959,#11960,#11961,#11962,#11963,#11964,#11965,#11966,#11967,
#11968,#11969,#11970,#11971,#11972,#11973,#11974,#11975,#11976,#11977,#11978,
#11979,#11980,#11981,#11982,#11983,#11984,#11985,#11986,#11987,#11988,#11989,
#11990,#11991,#11992,#11993,#11994,#11995,#11996,#11997,#11998,#11999,#12000,
#12001,#12002,#12003,#12004,#12005,#12006,#12007,#12008,#12009,#12010,#12011,
#12012,#12013,#12014,#12015,#12016,#12017,#12018,#12019),.UNSPECIFIED.,
 .F.,.F.,(4,2,2,2,2,2,2,2,2,2,2,2,2,2,2,2,2,2,2,2,2,2,2,2,2,2,2,2,2,2,2,
2,2,2,2,2,2,2,2,2,2,2,2,2,2,2,2,2,2,2,2,2,2,2,2,2,2,2,2,2,2,2,2,2,2,2,2,
2,2,2,2,2,2,2,2,2,2,2,2,2,2,2,2,2,2,2,2,2,2,2,2,2,2,2,2,2,2,2,2,2,2,2,2,
2,2,2,2,2,2,2,4),(-0.983965850740792,-0.976428697428846,-0.959045095961489,
-0.952876404968067,-0.948949764161217,-0.947535827801338,-0.946582177705485,
-0.945723405608626,-0.944539842061414,-0.941530835141036,-0.922281673275152,
-0.903762537031074,-0.896724178341862,-0.891632474803611,-0.889404206799181,
-0.887746973845169,-0.886196914496551,-0.883626948700429,-0.876814880707329,
-0.846213007603617,-0.83715097356694,-0.833701920004943,-0.831160152720884,
-0.829969847312564,-0.829060827846964,-0.827994052118297,-0.826114188563904,
-0.817802398410004,-0.792860302132136,-0.776564021948787,-0.77329597848607,
-0.771422870431342,-0.76979143471797,-0.767773467493801,-0.764662372283216,
-0.74225374988622,-0.718463153736229,-0.714550134167476,-0.713093994412623,
-0.712227047949536,-0.71128142153802,-0.709907802106248,-0.706265635557273,
-0.7007048015412,-0.68098909362998,-0.659699936987695,-0.656561536305509,
-0.654535206144928,-0.652903074845401,-0.651035807311733,-0.647795149662252,
-0.632095427960709,-0.609174234092233,-0.604739213945095,-0.59796325257311,
-0.596176533825275,-0.595141251301399,-0.594216936000927,-0.592967396330633,
-0.590100111197881,-0.576846030924175,-0.568460602809955,-0.544317396501895,
-0.539674031624726,-0.537548345915618,-0.53590096725911,-0.534110828263999,
-0.531224746360662,-0.520857145987655,-0.500579691464689,-0.498155800088846,
-0.481347157268226,-0.479411982654054,-0.478228173420962,-0.477311400996102,
-0.476236606468444,-0.474267874747157,-0.463013411690192,-0.447187888902494,
-0.425228744858819,-0.422086261431702,-0.420058659823978,-0.418426385971435,
-0.416559917619868,-0.413323126686715,-0.397704962907729,-0.375492237198176,
-0.370616026629478,-0.363532450079602,-0.361719435784044,-0.360678368129702,
-0.359755537405875,-0.35851698649178,-0.355712159094041,-0.343050632059556,
-0.339789268291339,-0.311247873410837,-0.305737138156674,-0.303607241145018,
-0.30206118217053,-0.300401119482355,-0.298156542080228,-0.292970615229178,
-0.285759137709564,-0.26639756419925,-0.248273508693048,-0.245258751663719,
-0.244074127698381,-0.243215004790582,-0.242261459367992,-0.241913378149247),
 .UNSPECIFIED.);
#121=B_SPLINE_CURVE_WITH_KNOTS('',3,(#12024,#12025,#12026,#12027,#12028,
#12029,#12030,#12031,#12032,#12033,#12034,#12035,#12036,#12037,#12038,#12039,
#12040,#12041,#12042,#12043,#12044,#12045,#12046,#12047,#12048,#12049,#12050,
#12051,#12052,#12053,#12054,#12055,#12056,#12057,#12058,#12059,#12060,#12061,
#12062,#12063,#12064,#12065,#12066,#12067,#12068,#12069,#12070,#12071,#12072,
#12073,#12074,#12075,#12076,#12077,#12078,#12079,#12080,#12081,#12082,#12083,
#12084,#12085,#12086,#12087,#12088,#12089,#12090,#12091,#12092,#12093,#12094,
#12095,#12096,#12097,#12098,#12099,#12100,#12101,#12102,#12103,#12104,#12105,
#12106,#12107,#12108,#12109,#12110,#12111,#12112,#12113,#12114,#12115,#12116,
#12117,#12118,#12119,#12120,#12121,#12122,#12123,#12124,#12125,#12126,#12127,
#12128,#12129,#12130,#12131,#12132,#12133,#12134,#12135,#12136,#12137,#12138,
#12139,#12140,#12141,#12142,#12143,#12144,#12145,#12146,#12147,#12148,#12149,
#12150,#12151,#12152,#12153,#12154,#12155,#12156,#12157,#12158,#12159,#12160,
#12161,#12162,#12163,#12164,#12165,#12166,#12167,#12168,#12169,#12170,#12171,
#12172,#12173,#12174,#12175,#12176,#12177,#12178,#12179,#12180,#12181,#12182,
#12183,#12184,#12185,#12186,#12187,#12188,#12189,#12190,#12191,#12192,#12193,
#12194,#12195,#12196,#12197,#12198,#12199,#12200,#12201,#12202,#12203,#12204,
#12205,#12206,#12207,#12208,#12209,#12210,#12211,#12212,#12213,#12214,#12215,
#12216,#12217,#12218,#12219,#12220,#12221,#12222,#12223,#12224,#12225,#12226,
#12227,#12228,#12229,#12230,#12231,#12232,#12233,#12234,#12235,#12236,#12237,
#12238,#12239,#12240,#12241,#12242,#12243,#12244,#12245),.UNSPECIFIED.,
 .F.,.F.,(4,2,2,2,2,2,2,2,2,2,2,2,2,2,2,2,2,2,2,2,2,2,2,2,2,2,2,2,2,2,2,
2,2,2,2,2,2,2,2,2,2,2,2,2,2,2,2,2,2,2,2,2,2,2,2,2,2,2,2,2,2,2,2,2,2,2,2,
2,2,2,2,2,2,2,2,2,2,2,2,2,2,2,2,2,2,2,2,2,2,2,2,2,2,2,2,2,2,2,2,2,2,2,2,
2,2,2,2,2,2,2,4),(-1.24275875787133,-1.22762709042559,-1.22439557108871,
-1.22253040814363,-1.22089824662139,-1.21886943960928,-1.21572244605731,
-1.19377471854145,-1.1779530859873,-1.16668254077522,-1.16471331138028,
-1.1636385000826,-1.16272186196663,-1.16153841649317,-1.15960421697158,
-1.1434311354434,-1.14040894422488,-1.12013411227508,-1.11326239930923,
-1.10826253976813,-1.10605016131273,-1.10439542077469,-1.10284093033319,
-1.10024756798278,-1.09327378678655,-1.06282525540613,-1.05380937532503,
-1.04869512696797,-1.04713608115745,-1.04615109810587,-1.04521546079699,
-1.04384498891157,-1.04123808540654,-1.01765465716894,-1.00141723025515,
-0.995349644485654,-0.990804417400253,-0.988673760726219,-0.987030681099189,
-0.985225638721172,-0.982271084517546,-0.972308353985407,-0.941761417526941,
-0.935265240655457,-0.931189948491823,-0.929755678374846,-0.928797660019481,
-0.927942185370316,-0.926772233310791,-0.923845209926974,-0.902247053177529,
-0.884696379319723,-0.878347622556955,-0.873641060241546,-0.871480653994794,
-0.869833424525861,-0.868042305160197,-0.865152090496027,-0.855774016661728,
-0.830787781031016,-0.815186007645975,-0.813095244649029,-0.811994570448843,
-0.811079827689608,-0.809929016013944,-0.808104496425623,-0.79764984218356,
-0.789148471402704,-0.762083629338326,-0.75670033941679,-0.754422528616797,
-0.752756721290641,-0.751218527442592,-0.748713842179597,-0.742321661881945,
-0.732501371157368,-0.717302382328109,-0.716304926794569,-0.709948205956288,
-0.697948099926155,-0.696068579989618,-0.694901291903405,-0.693985708609038,
-0.692898547487598,-0.690871865540765,-0.677931799445221,-0.649154283611957,
-0.640627360955181,-0.637831985324643,-0.636061554521682,-0.634407203720999,
-0.632198307072287,-0.627219327042051,-0.620384717817706,-0.600321734957142,
-0.582231537016983,-0.579215353915678,-0.578030480957579,-0.577171283423045,
-0.576217775081048,-0.57480509047453,-0.570888516213993,-0.564742830092001,
-0.547349286418453,-0.524661547707217,-0.52153867618665,-0.519517001818466,
-0.517885131453972,-0.516014334483734,-0.512757624437976,-0.500801107159108),
 .UNSPECIFIED.);
#122=B_SPLINE_CURVE_WITH_KNOTS('',3,(#12247,#12248,#12249,#12250,#12251,
#12252,#12253,#12254,#12255,#12256,#12257,#12258,#12259,#12260,#12261,#12262,
#12263,#12264,#12265,#12266,#12267,#12268,#12269,#12270,#12271,#12272,#12273,
#12274,#12275,#12276,#12277,#12278,#12279,#12280,#12281,#12282,#12283,#12284,
#12285,#12286,#12287,#12288,#12289,#12290,#12291,#12292,#12293,#12294,#12295,
#12296,#12297,#12298,#12299,#12300,#12301,#12302,#12303,#12304,#12305,#12306,
#12307,#12308,#12309,#12310,#12311,#12312,#12313,#12314,#12315,#12316,#12317,
#12318,#12319,#12320,#12321,#12322),.UNSPECIFIED.,.F.,.F.,(4,2,2,2,2,2,
2,2,2,2,2,2,2,2,2,2,2,2,2,2,2,2,2,2,2,2,2,2,2,2,2,2,2,2,2,2,2,4),(-0.241913378149247,
-0.240848529093374,-0.236930072495017,-0.230780351330327,-0.213387702374564,
-0.190697843519608,-0.187574853042253,-0.185553162085369,-0.183921322020081,
-0.182050611408162,-0.178794197570654,-0.162762320117167,-0.148323804694671,
-0.131022001665608,-0.128017273181183,-0.126834312529553,-0.125975612122178,
-0.125040770468585,-0.123674078159674,-0.122081740969019,-0.119145492171102,
-0.0866091802778103,-0.0730245358674191,-0.0698237409054384,-0.0679467365411574,
-0.0663156176982367,-0.0643028117346279,-0.060366494308501,-0.0379726691064073,
-0.019855373815882,-0.0125687094178807,-0.010314958382663,-0.00916598278167907,
-0.00830796414785512,-0.00744080725723779,-0.00637243950620114,-0.00397627449831531,
-0.000340284409424339),.UNSPECIFIED.);
#123=B_SPLINE_CURVE_WITH_KNOTS('',3,(#12323,#12324,#12325,#12326,#12327,
#12328,#12329,#12330,#12331,#12332,#12333,#12334,#12335,#12336,#12337,#12338,
#12339,#12340,#12341,#12342,#12343,#12344,#12345,#12346,#12347,#12348,#12349,
#12350,#12351,#12352,#12353,#12354,#12355,#12356,#12357,#12358,#12359,#12360,
#12361,#12362,#12363,#12364,#12365,#12366,#12367,#12368,#12369,#12370,#12371,
#12372,#12373,#12374,#12375,#12376,#12377,#12378,#12379,#12380,#12381,#12382,
#12383,#12384,#12385,#12386,#12387,#12388,#12389,#12390,#12391,#12392,#12393,
#12394,#12395,#12396,#12397,#12398,#12399,#12400,#12401,#12402,#12403,#12404,
#12405,#12406,#12407,#12408,#12409,#12410,#12411,#12412,#12413,#12414,#12415,
#12416,#12417,#12418,#12419,#12420,#12421,#12422,#12423,#12424,#12425,#12426,
#12427,#12428,#12429,#12430,#12431,#12432,#12433,#12434,#12435,#12436,#12437,
#12438,#12439,#12440,#12441,#12442,#12443,#12444,#12445,#12446,#12447,#12448,
#12449,#12450,#12451,#12452,#12453,#12454,#12455,#12456,#12457,#12458,#12459,
#12460,#12461,#12462,#12463,#12464,#12465,#12466),.UNSPECIFIED.,.F.,.F.,
(4,2,2,2,2,2,2,2,2,2,2,2,2,2,2,2,2,2,2,2,2,2,2,2,2,2,2,2,2,2,2,2,2,2,2,
2,2,2,2,2,2,2,2,2,2,2,2,2,2,2,2,2,2,2,2,2,2,2,2,2,2,2,2,2,2,2,2,2,2,2,2,
4),(-1.48418159104277,-1.44929736991942,-1.43894158361684,-1.4360579623585,
-1.43426916311607,-1.43262289081551,-1.43049845413665,-1.42585712116349,
-1.40172735276898,-1.38793036424003,-1.38161779511944,-1.37890912617517,
-1.37740357484174,-1.37612666886343,-1.37520494917929,-1.37434013478619,
-1.37313204004411,-1.37063563727009,-1.34588640567838,-1.33035881398873,
-1.32445255784646,-1.32000161110428,-1.31788943205404,-1.31624961354488,
-1.31443705457726,-1.31144445990731,-1.30107279587294,-1.27098596656034,
-1.26452340553208,-1.26046392915307,-1.25903237427002,-1.2580753728876,
-1.25722019698239,-1.25604989864143,-1.25311813286199,-1.23161483158907,
-1.21401904208531,-1.207662601943,-1.20295237769528,-1.2007921912895,-1.19914590817853,
-1.19735658243439,-1.19447097258771,-1.18512327836783,-1.15391233762704,
-1.14737527465886,-1.14328230813391,-1.14184619914704,-1.1408881759123,
-1.14003364753053,-1.13886618746356,-1.13591971620666,-1.11456890259433,
-1.09686405051954,-1.09048491967064,-1.08576168707199,-1.0835990108936,
-1.08195224081831,-1.08016376225593,-1.07728257639724,-1.06797867254565,
-1.04300610243364,-1.02732460955563,-1.02523337126674,-1.02413298236893,
-1.02321879106532,-1.02206908251009,-1.02024706731368,-1.00983532228453,
-1.00135508142519,-0.986941262039221,-0.98392338245625),.UNSPECIFIED.);
#124=B_SPLINE_CURVE_WITH_KNOTS('',3,(#12472,#12473,#12474,#12475,#12476,
#12477,#12478,#12479,#12480,#12481,#12482,#12483,#12484,#12485,#12486,#12487,
#12488,#12489,#12490,#12491,#12492,#12493,#12494,#12495,#12496,#12497,#12498,
#12499,#12500,#12501,#12502,#12503,#12504,#12505,#12506,#12507,#12508,#12509,
#12510,#12511,#12512,#12513,#12514,#12515,#12516,#12517,#12518,#12519,#12520,
#12521,#12522,#12523,#12524,#12525,#12526,#12527,#12528,#12529,#12530,#12531,
#12532,#12533,#12534,#12535,#12536,#12537,#12538,#12539,#12540,#12541,#12542,
#12543,#12544,#12545,#12546,#12547,#12548,#12549,#12550,#12551,#12552,#12553,
#12554,#12555,#12556,#12557,#12558,#12559,#12560,#12561,#12562,#12563,#12564,
#12565,#12566,#12567,#12568,#12569,#12570,#12571,#12572,#12573,#12574,#12575,
#12576,#12577,#12578,#12579,#12580,#12581,#12582,#12583,#12584,#12585,#12586,
#12587,#12588,#12589,#12590,#12591,#12592,#12593,#12594,#12595,#12596,#12597,
#12598,#12599,#12600,#12601,#12602,#12603,#12604,#12605,#12606,#12607,#12608,
#12609,#12610,#12611,#12612,#12613,#12614,#12615,#12616,#12617,#12618,#12619,
#12620,#12621),.UNSPECIFIED.,.F.,.F.,(4,2,2,2,2,2,2,2,2,2,2,2,2,2,2,2,2,
2,2,2,2,2,2,2,2,2,2,2,2,2,2,2,2,2,2,2,2,2,2,2,2,2,2,2,2,2,2,2,2,2,2,2,2,
2,2,2,2,2,2,2,2,2,2,2,2,2,2,2,2,2,2,2,2,2,4),(-0.500743339736994,-0.500421455876749,
-0.499506597245934,-0.49840543860593,-0.496312827532433,-0.480614849588234,
-0.455603525682823,-0.446342355606896,-0.443464334025091,-0.44167567878242,
-0.440027307419358,-0.437860417924,-0.433119313896671,-0.426709332808253,
-0.408863275680894,-0.387663978310866,-0.38470805180707,-0.38353860100022,
-0.382683143320616,-0.381724705912274,-0.380289060085995,-0.376204665646574,
-0.36968950165102,-0.338833978450358,-0.329159255197456,-0.32623652512599,
-0.324438172499309,-0.322792810799851,-0.320647172804963,-0.316022388278023,
-0.309816286013742,-0.29294548214833,-0.270284042353455,-0.267413052528543,
-0.266252574012108,-0.265314591024113,-0.264332560995082,-0.262787692009562,
-0.257804876891455,-0.24913362992991,-0.22205701802673,-0.211989251081525,
-0.20902297549004,-0.207215138753453,-0.205572341918865,-0.203446066573736,
-0.198925841160012,-0.192901155243357,-0.176858899977733,-0.152929626487514,
-0.150341589158695,-0.148975882894424,-0.148040995266714,-0.147054229540533,
-0.145487807603155,-0.140404622250099,-0.131426679864947,-0.099285778178127,
-0.0935252617907595,-0.0911211697337286,-0.0894489453937931,-0.0877405569327365,
-0.0854750105786094,-0.0794775833616094,-0.0706309881269793,-0.0545732589707769,
-0.0359720291257095,-0.032960140758076,-0.031775904382688,-0.0309168077256966,
-0.0299629763195435,-0.0285490724174048,-0.0269145647411012,-0.0238658217156568,
-0.000340704748871543),.UNSPECIFIED.);
#125=B_SPLINE_CURVE_WITH_KNOTS('',3,(#12622,#12623,#12624,#12625,#12626,
#12627,#12628,#12629,#12630,#12631,#12632,#12633,#12634,#12635,#12636,#12637,
#12638,#12639,#12640,#12641,#12642,#12643,#12644,#12645,#12646,#12647,#12648,
#12649,#12650,#12651,#12652,#12653,#12654,#12655,#12656,#12657,#12658,#12659,
#12660,#12661,#12662,#12663,#12664,#12665,#12666,#12667,#12668,#12669,#12670,
#12671,#12672,#12673,#12674,#12675,#12676,#12677,#12678,#12679,#12680,#12681,
#12682,#12683,#12684,#12685,#12686,#12687,#12688,#12689,#12690,#12691,#12692,
#12693),.UNSPECIFIED.,.F.,.F.,(4,2,2,2,2,2,2,2,2,2,2,2,2,2,2,2,2,2,2,2,
2,2,2,2,2,2,2,2,2,2,2,2,2,2,2,4),(-1.48439292099721,-1.46367001774405,-1.46072402984557,
-1.458783958121,-1.45722482916291,-1.45559553177565,-1.45369435093942,-1.45038621433275,
-1.43466982309695,-1.42023860716416,-1.40260871447461,-1.39970369498598,
-1.39842711079842,-1.3974989050233,-1.39647683777673,-1.39474958742878,
-1.38861335916595,-1.36449168775534,-1.35154719928667,-1.34627169432974,
-1.34223098290889,-1.34025737936908,-1.33861898239508,-1.33679518963765,
-1.33375375619854,-1.32300731311845,-1.29661177082536,-1.28397018117173,
-1.28195284410562,-1.28086779668327,-1.27995223177072,-1.27878272149796,
-1.27689537761869,-1.26467333372395,-1.24314862470824,-1.24275875787133),
 .UNSPECIFIED.);
#126=B_SPLINE_CURVE_WITH_KNOTS('',3,(#12694,#12695,#12696,#12697,#12698,
#12699,#12700,#12701,#12702,#12703,#12704,#12705,#12706,#12707,#12708,#12709,
#12710,#12711,#12712,#12713,#12714,#12715,#12716,#12717,#12718,#12719,#12720,
#12721,#12722,#12723,#12724,#12725,#12726,#12727,#12728,#12729,#12730,#12731,
#12732,#12733,#12734,#12735,#12736,#12737,#12738,#12739,#12740,#12741,#12742,
#12743,#12744,#12745,#12746,#12747,#12748,#12749,#12750,#12751,#12752,#12753,
#12754,#12755,#12756,#12757,#12758,#12759,#12760,#12761,#12762,#12763,#12764,
#12765,#12766,#12767,#12768,#12769,#12770,#12771,#12772,#12773,#12774,#12775,
#12776,#12777,#12778,#12779,#12780,#12781,#12782,#12783,#12784,#12785,#12786,
#12787,#12788,#12789,#12790,#12791,#12792,#12793,#12794,#12795,#12796,#12797,
#12798,#12799,#12800,#12801,#12802,#12803,#12804,#12805,#12806,#12807,#12808,
#12809,#12810,#12811,#12812,#12813,#12814,#12815,#12816,#12817,#12818,#12819,
#12820,#12821,#12822,#12823,#12824,#12825,#12826,#12827,#12828,#12829,#12830,
#12831,#12832,#12833,#12834,#12835,#12836,#12837,#12838,#12839,#12840,#12841,
#12842,#12843,#12844,#12845,#12846,#12847,#12848,#12849,#12850,#12851,#12852,
#12853,#12854,#12855,#12856,#12857,#12858,#12859,#12860,#12861,#12862,#12863,
#12864,#12865,#12866,#12867,#12868,#12869,#12870,#12871,#12872,#12873,#12874,
#12875,#12876,#12877,#12878,#12879,#12880,#12881,#12882,#12883,#12884,#12885,
#12886,#12887,#12888,#12889,#12890,#12891,#12892,#12893,#12894,#12895,#12896,
#12897,#12898,#12899,#12900,#12901,#12902,#12903,#12904,#12905,#12906,#12907,
#12908,#12909,#12910,#12911,#12912,#12913,#12914,#12915,#12916,#12917,#12918,
#12919),.UNSPECIFIED.,.F.,.F.,(4,2,2,2,2,2,2,2,2,2,2,2,2,2,2,2,2,2,2,2,
2,2,2,2,2,2,2,2,2,2,2,2,2,2,2,2,2,2,2,2,2,2,2,2,2,2,2,2,2,2,2,2,2,2,2,2,
2,2,2,2,2,2,2,2,2,2,2,2,2,2,2,2,2,2,2,2,2,2,2,2,2,2,2,2,2,2,2,2,2,2,2,2,
2,2,2,2,2,2,2,2,2,2,2,2,2,2,2,2,2,2,2,2,4),(-0.98392338245625,-0.970918750570274,
-0.967664039126509,-0.965794214877276,-0.964163091574368,-0.96214221590316,
-0.959020315499482,-0.936334225555645,-0.918946970736374,-0.912788245005535,
-0.908866491933244,-0.907453480822628,-0.906500212350217,-0.905641593853108,
-0.904458000835556,-0.901447624246592,-0.883296323715773,-0.867241660699311,
-0.853509265326825,-0.850376134030576,-0.848532635420459,-0.846898178277098,
-0.844838229386295,-0.840661813294719,-0.810527176040019,-0.807808209204365,
-0.794190764617428,-0.791286786422429,-0.790031127090533,-0.78910621761936,
-0.788074607086689,-0.786303533793514,-0.779698445446821,-0.77309351987115,
-0.754039015969418,-0.742463178524203,-0.735286453883284,-0.732664830466287,
-0.731105251187416,-0.729453828775095,-0.727260871287469,-0.722369737277023,
-0.715692211867115,-0.682455098181662,-0.675250834469183,-0.673449353171648,
-0.672400578454938,-0.671572180997403,-0.6704014391641,-0.667961477888814,
-0.664690357240238,-0.656332468101261,-0.63138609296106,-0.619095480185138,
-0.615943131111451,-0.614095225128673,-0.612624482837142,-0.610648422290045,
-0.606891812071816,-0.602139266854766,-0.591113263942786,-0.567929528437556,
-0.558309446846038,-0.556354594489674,-0.555270966905107,-0.554355330924907,
-0.553184117199866,-0.550741768405048,-0.547466526286373,-0.539092711311397,
-0.514062657832062,-0.501866994545461,-0.498720820905074,-0.496874240061176,
-0.495403300203329,-0.49342535611242,-0.489659664291114,-0.484892526088455,
-0.473815358624704,-0.448218747985731,-0.440836754737095,-0.439021268654963,
-0.437969247007175,-0.437141381312766,-0.435975421877467,-0.433560309165682,
-0.43033218654854,-0.422140429973167,-0.398022286911143,-0.384773859320031,
-0.381594253175902,-0.379722172598729,-0.378090769949651,-0.376071730868114,
-0.372103801650872,-0.34650241058291,-0.325457552277464,-0.322505295114932,
-0.321331188708105,-0.320474780316983,-0.319518278195589,-0.318090716740568,
-0.314064244250429,-0.307677074877968,-0.293559909055934,-0.269885403914129,
-0.265230968057928,-0.263103425792196,-0.261455922618325,-0.259666962080203,
-0.256785697064329,-0.246469729589058,-0.242037410218006),.UNSPECIFIED.);
#127=B_SPLINE_CURVE_WITH_KNOTS('',3,(#12924,#12925,#12926,#12927,#12928,
#12929,#12930,#12931,#12932,#12933,#12934,#12935,#12936,#12937,#12938,#12939,
#12940,#12941,#12942,#12943,#12944,#12945,#12946,#12947,#12948,#12949,#12950,
#12951,#12952,#12953,#12954,#12955,#12956,#12957,#12958,#12959,#12960,#12961,
#12962,#12963,#12964,#12965,#12966,#12967,#12968,#12969,#12970,#12971,#12972,
#12973,#12974,#12975,#12976,#12977,#12978,#12979,#12980,#12981,#12982,#12983,
#12984,#12985,#12986,#12987,#12988,#12989,#12990,#12991,#12992,#12993,#12994,
#12995,#12996,#12997,#12998,#12999,#13000,#13001,#13002,#13003,#13004,#13005,
#13006,#13007,#13008,#13009,#13010,#13011,#13012,#13013,#13014,#13015,#13016,
#13017,#13018,#13019,#13020,#13021,#13022,#13023,#13024,#13025,#13026,#13027,
#13028,#13029,#13030,#13031,#13032,#13033,#13034,#13035,#13036,#13037,#13038,
#13039,#13040,#13041,#13042,#13043,#13044,#13045,#13046,#13047,#13048,#13049,
#13050,#13051,#13052,#13053,#13054,#13055,#13056,#13057,#13058,#13059,#13060,
#13061,#13062,#13063,#13064,#13065,#13066,#13067,#13068,#13069,#13070,#13071,
#13072,#13073,#13074,#13075,#13076,#13077,#13078,#13079,#13080,#13081,#13082,
#13083,#13084,#13085,#13086,#13087,#13088,#13089,#13090,#13091,#13092,#13093,
#13094,#13095,#13096,#13097,#13098,#13099,#13100,#13101,#13102,#13103,#13104,
#13105,#13106,#13107,#13108,#13109,#13110,#13111,#13112,#13113,#13114,#13115,
#13116,#13117,#13118,#13119,#13120,#13121,#13122,#13123,#13124,#13125,#13126,
#13127,#13128,#13129,#13130,#13131),.UNSPECIFIED.,.F.,.F.,(4,2,2,2,2,2,
2,2,2,2,2,2,2,2,2,2,2,2,2,2,2,2,2,2,2,2,2,2,2,2,2,2,2,2,2,2,2,2,2,2,2,2,
2,2,2,2,2,2,2,2,2,2,2,2,2,2,2,2,2,2,2,2,2,2,2,2,2,2,2,2,2,2,2,2,2,2,2,2,
2,2,2,2,2,2,2,2,2,2,2,2,2,2,2,2,2,2,2,2,2,2,2,2,2,4),(-1.24292430977669,
-1.22009850972989,-1.21117710213601,-1.20776282107661,-1.20524074898063,
-1.2040540418608,-1.20313692546008,-1.20206393200115,-1.20015717115628,
-1.19142022094294,-1.15971845873916,-1.15315464924074,-1.14832643144998,
-1.14614415127837,-1.14449380396601,-1.14271239640236,-1.13986663518086,
-1.13091402299806,-1.09717191663782,-1.08926948880272,-1.08747306209823,
-1.08643552429681,-1.08551158324381,-1.08428737171035,-1.0814893181499,
-1.05681554278257,-1.03442687168121,-1.03052803654771,-1.02852250440633,
-1.02689148096121,-1.02500813191233,-1.02178059200139,-1.0077440924415,
-0.984206081141666,-0.972353882315983,-0.97036242914734,-0.969282656895497,
-0.968366229833341,-0.967188777629931,-0.965275467936706,-0.951334726570139,
-0.934728329995926,-0.917880693945739,-0.91354506953747,-0.911453584049901,
-0.909814915394111,-0.907988292250247,-0.904936104965671,-0.893981686742702,
-0.867781741071759,-0.859210709444466,-0.85426725340917,-0.85272670799984,
-0.851745599744519,-0.850806907834202,-0.849643893636765,-0.846758324974834,
-0.8242946418618,-0.800006927103579,-0.796051507034116,-0.794034483656647,
-0.792402609987792,-0.790527671492334,-0.787337555593231,-0.773936388515977,
-0.751720296040212,-0.742327945440058,-0.737167921714137,-0.735545207780734,
-0.734545984105842,-0.733607309992557,-0.732271387261892,-0.728880933198242,
-0.723835784409313,-0.706744720142412,-0.683863525512931,-0.679195931896086,
-0.677065537869152,-0.675417112106932,-0.673628429504836,-0.670750439014821,
-0.660478934899834,-0.640551609385216,-0.622258878077178,-0.619249388201306,
-0.618065446390248,-0.617206340419922,-0.616252229611334,-0.614837453166633,
-0.610907346566536,-0.60473279506166,-0.587363628894845,-0.564684751763273,
-0.561561087344327,-0.559538893347397,-0.557906599438009,-0.556035312403824,
-0.552777737550461,-0.536734606063427,-0.522306323992666,-0.513818536135711,
-0.503395615840758,-0.501572057791962,-0.500743339736994),.UNSPECIFIED.);
#128=B_SPLINE_CURVE_WITH_KNOTS('',3,(#13133,#13134,#13135,#13136,#13137,
#13138,#13139,#13140,#13141,#13142,#13143,#13144,#13145,#13146,#13147,#13148,
#13149,#13150,#13151,#13152,#13153,#13154,#13155,#13156,#13157,#13158,#13159,
#13160,#13161,#13162,#13163,#13164,#13165,#13166,#13167,#13168,#13169,#13170,
#13171,#13172,#13173,#13174,#13175,#13176,#13177,#13178,#13179,#13180,#13181,
#13182,#13183,#13184,#13185,#13186,#13187,#13188,#13189,#13190,#13191,#13192,
#13193,#13194,#13195,#13196,#13197,#13198,#13199,#13200,#13201,#13202,#13203,
#13204,#13205,#13206,#13207,#13208,#13209,#13210,#13211,#13212,#13213,#13214,
#13215,#13216,#13217,#13218,#13219,#13220,#13221,#13222,#13223,#13224,#13225,
#13226,#13227,#13228,#13229,#13230,#13231,#13232,#13233,#13234,#13235,#13236,
#13237,#13238,#13239,#13240,#13241,#13242,#13243,#13244,#13245,#13246,#13247,
#13248,#13249,#13250),.UNSPECIFIED.,.F.,.F.,(4,2,2,2,2,2,2,2,2,2,2,2,2,
2,2,2,2,2,2,2,2,2,2,2,2,2,2,2,2,2,2,2,2,2,2,2,2,2,2,2,2,2,2,2,2,2,2,2,2,
2,2,2,2,2,2,2,2,2,4),(-0.242037410218006,-0.226377901503412,-0.208326430520444,
-0.205307938065085,-0.204122761128431,-0.203263550654683,-0.202310285714343,
-0.200898413453342,-0.196987019685073,-0.1908524427467,-0.173446015566506,
-0.15075166387754,-0.147628322635545,-0.145606627344241,-0.143974928387371,
-0.143947604441549,-0.143910219998259,-0.143875060873207,-0.14384198161352,
-0.143810847108984,-0.143781531857172,-0.143753919264978,-0.143727900992463,
-0.143703376333799,-0.143680251642651,-0.143658439798503,-0.143637859708992,
-0.143618435852104,-0.143600097857734,-0.143582780115167,-0.143566421414623,
-0.143550964619338,-0.143536356363321,-0.143522546769911,-0.143509489196654,
-0.143497140002465,-0.143485458325707,-0.143474405892461,-0.141501492676609,
-0.137462678591979,-0.132191756499697,-0.119265489938714,-0.0956030438442445,
-0.0890174849576289,-0.0872477763152912,-0.0862162683394732,-0.0852909391395101,
-0.0840340317944949,-0.0812441417872272,-0.0615593745656791,-0.0478414017756538,
-0.0332210227450641,-0.0299624167846491,-0.028072259689996,-0.0264420824065228,
-0.0248792806951741,-0.0229262642438582,-0.0199490446044993,-0.000340462828452178),
 .UNSPECIFIED.);
#129=B_SPLINE_CURVE_WITH_KNOTS('',3,(#13251,#13252,#13253,#13254,#13255,
#13256,#13257,#13258,#13259,#13260,#13261,#13262,#13263,#13264,#13265,#13266,
#13267,#13268,#13269,#13270,#13271,#13272,#13273,#13274,#13275,#13276,#13277,
#13278,#13279,#13280,#13281,#13282,#13283,#13284,#13285,#13286,#13287,#13288,
#13289,#13290,#13291,#13292,#13293,#13294,#13295,#13296,#13297,#13298,#13299,
#13300,#13301,#13302,#13303,#13304,#13305,#13306,#13307,#13308,#13309,#13310,
#13311,#13312,#13313,#13314,#13315,#13316,#13317,#13318,#13319,#13320,#13321,
#13322,#13323,#13324,#13325,#13326,#13327,#13328,#13329,#13330,#13331,#13332,
#13333,#13334,#13335,#13336,#13337,#13338,#13339,#13340,#13341,#13342,#13343,
#13344,#13345,#13346,#13347,#13348,#13349,#13350,#13351,#13352,#13353,#13354,
#13355,#13356,#13357,#13358,#13359,#13360,#13361,#13362,#13363,#13364,#13365,
#13366,#13367,#13368,#13369,#13370,#13371,#13372,#13373,#13374,#13375,#13376,
#13377,#13378,#13379,#13380,#13381,#13382,#13383,#13384,#13385,#13386,#13387,
#13388,#13389,#13390,#13391,#13392,#13393,#13394,#13395,#13396),
 .UNSPECIFIED.,.F.,.F.,(4,2,2,2,2,2,2,2,2,2,2,2,2,2,2,2,2,2,2,2,2,2,2,2,
2,2,2,2,2,2,2,2,2,2,2,2,2,2,2,2,2,2,2,2,2,2,2,2,2,2,2,2,2,2,2,2,2,2,2,2,
2,2,2,2,2,2,2,2,2,2,2,2,4),(-1.48433926685641,-1.45975807135474,-1.45670672976863,
-1.45507153755693,-1.45365737853428,-1.45270382492361,-1.45184533297032,
-1.4506624006039,-1.44765631229039,-1.42927933722712,-1.41475180710344,
-1.40052827236496,-1.3970514075773,-1.39544137590594,-1.39379363977833,
-1.39200704275363,-1.38913537389381,-1.37992472697872,-1.34648009397227,
-1.33860887100355,-1.33681039869128,-1.33577266208209,-1.33484924480734,
-1.33362665282004,-1.33083620409697,-1.30610364428062,-1.29057021029139,
-1.28466143703557,-1.28020851699269,-1.27809532681376,-1.27645469125338,
-1.2746411966735,-1.27164698147662,-1.26126888175128,-1.23116827023616,
-1.22470255631403,-1.22064108319677,-1.21920881525891,-1.21825133469458,
-1.21739572865764,-1.21622483926031,-1.21329158030501,-1.19177799241002,
-1.17417302845576,-1.16781332727807,-1.16310069872849,-1.16093942081488,
-1.15929231039467,-1.15750208988553,-1.15461504691953,-1.14526280523583,
-1.11403604048543,-1.10749568649636,-1.1034006612034,-1.10196383082756,
-1.10100532662837,-1.10015036944996,-1.09898232382121,-1.09603437509939,
-1.0746727870226,-1.05695908921771,-1.05057676492827,-1.04585116641477,
-1.0436874056261,-1.0420398091453,-1.04025043254736,-1.0373677988348,-1.02805920854845,
-1.00307411900119,-0.987384761064561,-0.985292473269602,-0.984191532099586,
-0.984010680622453),.UNSPECIFIED.);
#130=B_SPLINE_CURVE_WITH_KNOTS('',3,(#13402,#13403,#13404,#13405,#13406,
#13407,#13408,#13409,#13410,#13411,#13412,#13413,#13414,#13415,#13416,#13417,
#13418,#13419,#13420,#13421,#13422,#13423,#13424,#13425,#13426,#13427,#13428,
#13429,#13430,#13431,#13432,#13433,#13434,#13435,#13436,#13437,#13438,#13439,
#13440,#13441,#13442,#13443,#13444,#13445,#13446,#13447,#13448,#13449,#13450,
#13451,#13452,#13453,#13454,#13455,#13456,#13457,#13458,#13459,#13460,#13461,
#13462,#13463,#13464,#13465,#13466,#13467,#13468,#13469,#13470,#13471,#13472,
#13473,#13474,#13475,#13476,#13477,#13478,#13479,#13480,#13481,#13482,#13483,
#13484,#13485,#13486,#13487,#13488,#13489,#13490,#13491,#13492,#13493,#13494,
#13495,#13496,#13497,#13498,#13499,#13500,#13501,#13502,#13503,#13504,#13505,
#13506,#13507,#13508,#13509,#13510,#13511,#13512,#13513,#13514,#13515,#13516,
#13517,#13518,#13519,#13520,#13521,#13522,#13523,#13524,#13525,#13526,#13527,
#13528,#13529,#13530,#13531,#13532,#13533,#13534,#13535,#13536,#13537,#13538,
#13539,#13540,#13541,#13542,#13543,#13544,#13545,#13546,#13547,#13548,#13549,
#13550,#13551,#13552,#13553,#13554,#13555,#13556,#13557,#13558,#13559,#13560,
#13561),.UNSPECIFIED.,.F.,.F.,(4,2,2,2,2,2,2,2,2,2,2,2,2,2,2,2,2,2,2,2,
2,2,2,2,2,2,2,2,2,2,2,2,2,2,2,2,2,2,2,2,2,2,2,2,2,2,2,2,2,2,2,2,2,2,2,2,
2,2,2,2,2,2,2,2,2,2,2,2,2,2,2,2,2,2,2,2,2,2,2,4),(-0.500877068977447,-0.49420957397851,
-0.486243983230943,-0.483515943791592,-0.481759892900288,-0.480098968662855,
-0.477850391714746,-0.472642111419001,-0.465389743434716,-0.445822728983988,
-0.445056384759463,-0.437175356889427,-0.432966972603491,-0.425977449462116,
-0.424172203267863,-0.423132765937003,-0.422209386113219,-0.420967385311406,
-0.418143546064314,-0.405304815542059,-0.397169964439075,-0.372258221694176,
-0.368099080270406,-0.36601003283837,-0.364474158175748,-0.362806451946846,
-0.360518058034401,-0.355071007657741,-0.337852482692718,-0.317949735414949,
-0.308983947659993,-0.307063941704096,-0.305987938915715,-0.305071151693919,
-0.303888634881919,-0.301388685124148,-0.298013510633306,-0.289248655473679,
-0.26093496766503,-0.252001180990559,-0.249157279351985,-0.247376193767869,
-0.245725571351519,-0.243542077473293,-0.238707630352702,-0.232132103012891,
-0.200301395977919,-0.191673048791492,-0.18977333179338,-0.188701865905234,
-0.187784435283943,-0.186595228402586,-0.184060370545395,-0.163146355380599,
-0.137714066662209,-0.133563567964447,-0.131476569575409,-0.129941135191168,
-0.128306076750681,-0.126087476837623,-0.12360049236534,-0.119307513195447,
-0.109836791920459,-0.0941729325307969,-0.0762350431130515,-0.0732083045110218,
-0.072021527449423,-0.0711617440546169,-0.0702085423299039,-0.0687979376692082,
-0.0648975489169137,-0.0587874788908426,-0.0283441025441875,-0.0179681887086096,
-0.0148622485381598,-0.0130240025463066,-0.0114216011731331,-0.00984350975623947,
-0.00783814363815093,-0.000340318648320376),.UNSPECIFIED.);
#131=B_SPLINE_CURVE_WITH_KNOTS('',3,(#13562,#13563,#13564,#13565,#13566,
#13567,#13568,#13569,#13570,#13571,#13572,#13573,#13574,#13575,#13576,#13577,
#13578,#13579,#13580,#13581,#13582,#13583,#13584,#13585,#13586,#13587,#13588,
#13589,#13590,#13591,#13592,#13593,#13594,#13595,#13596,#13597,#13598,#13599,
#13600,#13601,#13602,#13603,#13604,#13605,#13606,#13607,#13608,#13609,#13610,
#13611,#13612,#13613,#13614,#13615,#13616,#13617,#13618,#13619,#13620,#13621,
#13622,#13623,#13624,#13625,#13626,#13627,#13628,#13629,#13630,#13631,#13632,
#13633,#13634,#13635),.UNSPECIFIED.,.F.,.F.,(4,2,2,2,2,2,2,2,2,2,2,2,2,
2,2,2,2,2,2,2,2,2,2,2,2,2,2,2,2,2,2,2,2,2,2,2,4),(-1.48451647550027,-1.453138561461,
-1.44142514844035,-1.43943890349013,-1.43836032782819,-1.43744390944019,
-1.43626517033315,-1.43434725721046,-1.4201148900124,-1.39668872794447,
-1.38876710752721,-1.38496742502763,-1.38267773562576,-1.38062685302709,
-1.38061075126092,-1.37903116612738,-1.3774642065727,-1.37480629934549,
-1.36737046093308,-1.33758067704553,-1.32851982802648,-1.32507088549672,
-1.32252908068291,-1.32133862648736,-1.32042943146041,-1.31936236402633,
-1.31748178086799,-1.30916291412439,-1.27705216305228,-1.27045655340445,
-1.26561044795672,-1.26342496301681,-1.26177412635694,-1.26021137240343,
-1.25757536252991,-1.25029959662761,-1.24292430977669),.UNSPECIFIED.);
#132=B_SPLINE_CURVE_WITH_KNOTS('',3,(#13636,#13637,#13638,#13639,#13640,
#13641,#13642,#13643,#13644,#13645,#13646,#13647,#13648,#13649,#13650,#13651,
#13652,#13653,#13654,#13655,#13656,#13657,#13658,#13659,#13660,#13661,#13662,
#13663,#13664,#13665,#13666,#13667,#13668,#13669,#13670,#13671,#13672,#13673,
#13674,#13675,#13676,#13677,#13678,#13679,#13680,#13681,#13682,#13683,#13684,
#13685,#13686,#13687,#13688,#13689,#13690,#13691,#13692,#13693,#13694,#13695,
#13696,#13697,#13698,#13699,#13700,#13701,#13702,#13703,#13704,#13705,#13706,
#13707,#13708,#13709,#13710,#13711,#13712,#13713,#13714,#13715,#13716,#13717,
#13718,#13719,#13720,#13721,#13722,#13723,#13724,#13725,#13726,#13727,#13728,
#13729,#13730,#13731,#13732,#13733,#13734,#13735,#13736,#13737,#13738,#13739,
#13740,#13741,#13742,#13743,#13744,#13745,#13746,#13747,#13748,#13749,#13750,
#13751,#13752,#13753,#13754,#13755,#13756,#13757,#13758,#13759,#13760,#13761,
#13762,#13763,#13764,#13765,#13766,#13767,#13768,#13769,#13770,#13771,#13772,
#13773,#13774,#13775,#13776,#13777,#13778,#13779,#13780,#13781,#13782,#13783,
#13784,#13785,#13786,#13787,#13788,#13789,#13790,#13791,#13792,#13793,#13794,
#13795,#13796,#13797,#13798,#13799,#13800,#13801,#13802,#13803,#13804,#13805,
#13806,#13807,#13808,#13809,#13810,#13811,#13812,#13813,#13814,#13815,#13816,
#13817,#13818,#13819,#13820,#13821,#13822,#13823,#13824,#13825,#13826,#13827,
#13828,#13829,#13830,#13831,#13832,#13833,#13834,#13835,#13836,#13837,#13838,
#13839,#13840,#13841,#13842,#13843,#13844,#13845,#13846,#13847,#13848,#13849,
#13850,#13851),.UNSPECIFIED.,.F.,.F.,(4,2,2,2,2,2,2,2,2,2,2,2,2,2,2,2,2,
2,2,2,2,2,2,2,2,2,2,2,2,2,2,2,2,2,2,2,2,2,2,2,2,2,2,2,2,2,2,2,2,2,2,2,2,
2,2,2,2,2,2,2,2,2,2,2,2,2,2,2,2,2,2,2,2,2,2,2,2,2,2,2,2,2,2,2,2,2,2,2,2,
2,2,2,2,2,2,2,2,2,2,2,2,2,2,2,2,2,2,4),(-0.984010680622453,-0.983276881955298,
-0.98212659632752,-0.980303666564888,-0.969886693743268,-0.961402172228227,
-0.946981067485029,-0.930950585751214,-0.927694244051038,-0.925823482036929,
-0.924191539989635,-0.922169649038764,-0.919046178479495,-0.896342672471697,
-0.878934906128747,-0.872784213011067,-0.868865597600561,-0.867452581316968,
-0.866498979134825,-0.865639801050707,-0.864455107846331,-0.861440165151471,
-0.843450643038574,-0.823322317990033,-0.812995416730585,-0.81011287859804,
-0.808323434641292,-0.806675689397829,-0.804548118311377,-0.799894835432268,
-0.776072670555639,-0.759683939702214,-0.754751414846854,-0.751417727830103,
-0.750090805574481,-0.749153899838092,-0.748275538754942,-0.746761208071483,
-0.742447345986866,-0.735219838592179,-0.719046110596642,-0.696853774651113,
-0.693716936107176,-0.691690971994999,-0.69005871989835,-0.68819085991827,
-0.684948001728182,-0.669207638321255,-0.645926681006725,-0.635526783116616,
-0.633704347473537,-0.632554181943724,-0.631639486098049,-0.630538314945968,
-0.628445124865518,-0.612701757282371,-0.587572878431817,-0.578447092961069,
-0.575583576041244,-0.573798270086154,-0.57214917910804,-0.569975750365758,
-0.565197208489379,-0.558720846342382,-0.540544821907918,-0.519829276205067,
-0.516862262662472,-0.515685537304518,-0.514828359157599,-0.513872383554146,
-0.512447989490181,-0.508446273233196,-0.502114318679527,-0.488240719495897,
-0.464212075387212,-0.459565066219429,-0.457438606845076,-0.455790995236776,
-0.454000969898426,-0.451115886450697,-0.440761496956498,-0.420533786818844,
-0.402644244852704,-0.399631416357241,-0.398447039642171,-0.397587920762662,
-0.396634168456819,-0.395220571811708,-0.391297949679015,-0.385139407257685,
-0.367753587181906,-0.34506576033978,-0.341942447075718,-0.339920544984728,
-0.338288533086466,-0.336417623938391,-0.333160860478709,-0.317127154123628,
-0.302692305813452,-0.294198583014737,-0.283777838649214,-0.281954576760602,
-0.280804167948434,-0.279889470685409,-0.278788528715068,-0.276696403545102,
-0.261010637430623,-0.241930398828716),.UNSPECIFIED.);
#133=B_SPLINE_CURVE_WITH_KNOTS('',3,(#13856,#13857,#13858,#13859,#13860,
#13861,#13862,#13863,#13864,#13865,#13866,#13867,#13868,#13869,#13870,#13871,
#13872,#13873,#13874,#13875,#13876,#13877,#13878,#13879,#13880,#13881,#13882,
#13883,#13884,#13885,#13886,#13887,#13888,#13889,#13890,#13891,#13892,#13893,
#13894,#13895,#13896,#13897,#13898,#13899,#13900,#13901,#13902,#13903,#13904,
#13905,#13906,#13907,#13908,#13909,#13910,#13911,#13912,#13913,#13914,#13915,
#13916,#13917,#13918,#13919,#13920,#13921,#13922,#13923,#13924,#13925,#13926,
#13927,#13928,#13929,#13930,#13931,#13932,#13933,#13934,#13935,#13936,#13937,
#13938,#13939,#13940,#13941,#13942,#13943,#13944,#13945,#13946,#13947,#13948,
#13949,#13950,#13951,#13952,#13953,#13954,#13955,#13956,#13957,#13958,#13959,
#13960,#13961,#13962,#13963,#13964,#13965,#13966,#13967,#13968,#13969,#13970,
#13971,#13972,#13973,#13974,#13975,#13976,#13977,#13978,#13979,#13980,#13981,
#13982,#13983,#13984,#13985,#13986,#13987,#13988,#13989,#13990,#13991,#13992,
#13993,#13994,#13995,#13996,#13997,#13998,#13999,#14000,#14001,#14002,#14003,
#14004,#14005,#14006,#14007,#14008,#14009,#14010,#14011,#14012,#14013,#14014,
#14015,#14016,#14017,#14018,#14019,#14020,#14021,#14022,#14023,#14024,#14025,
#14026,#14027,#14028,#14029,#14030,#14031,#14032,#14033,#14034,#14035,#14036,
#14037,#14038,#14039,#14040,#14041,#14042,#14043,#14044,#14045,#14046,#14047,
#14048,#14049,#14050,#14051,#14052,#14053,#14054,#14055,#14056,#14057,#14058,
#14059,#14060,#14061,#14062,#14063,#14064,#14065,#14066,#14067),
 .UNSPECIFIED.,.F.,.F.,(4,2,2,2,2,2,2,2,2,2,2,2,2,2,2,2,2,2,2,2,2,2,2,2,
2,2,2,2,2,2,2,2,2,2,2,2,2,2,2,2,2,2,2,2,2,2,2,2,2,2,2,2,2,2,2,2,2,2,2,2,
2,2,2,2,2,2,2,2,2,2,2,2,2,2,2,2,2,2,2,2,2,2,2,2,2,2,2,2,2,2,2,2,2,2,2,2,
2,2,2,2,2,2,2,2,2,4),(-1.24297181640774,-1.2427106352234,-1.2415244771508,
-1.23850109403567,-1.22054474535128,-1.20040417535915,-1.1900740137517,
-1.18719106031416,-1.18540143704267,-1.18375357546074,-1.18162591808405,
-1.17697268172044,-1.15315637795744,-1.14408068768981,-1.13113284813656,
-1.12829756047345,-1.12705353058867,-1.12612987531147,-1.12509148830716,
-1.12329106563629,-1.11635802555883,-1.10980684384822,-1.09226154632467,
-1.07535506155645,-1.07101218902478,-1.06891940979068,-1.06728069583163,
-1.06545502123208,-1.06240680401277,-1.05149331833715,-1.02525592379709,
-1.01668006947385,-1.01173484399188,-1.0101941708909,-1.00921308038126,
-1.00827449133722,-1.00711169498954,-1.00422711830385,-0.981756014399181,
-0.957477768123092,-0.953522707170614,-0.951505842933359,-0.949874086479932,
-0.947999269939254,-0.944809330520898,-0.931408303200817,-0.907395638602045,
-0.899223365514287,-0.896000089831674,-0.893587790363841,-0.892422135123552,
-0.891594066904416,-0.890541183317346,-0.888722921040427,-0.881309130587991,
-0.848294933610726,-0.838251876852001,-0.835395055617807,-0.833611179030274,
-0.831961552434656,-0.829821647757212,-0.82527563189193,-0.800020162397814,
-0.778892589866612,-0.776365809691835,-0.775178192494866,-0.774269262852029,
-0.773200253801601,-0.771311144490131,-0.762861625060097,-0.742599558811807,
-0.722150171937683,-0.719018622593057,-0.716994197198423,-0.715361964365038,
-0.713492787235848,-0.710244168417585,-0.694384701094228,-0.669967392019978,
-0.66072745533532,-0.658792200929812,-0.657712742348565,-0.656796310860641,
-0.655618504355478,-0.653143268783829,-0.649811239174844,-0.641217009952121,
-0.61482244656907,-0.604103548895954,-0.601063861025787,-0.599240044975084,
-0.597600950728689,-0.595504854819668,-0.591144625132405,-0.574098100995862,
-0.555399460614224,-0.549740400851259,-0.54315007293908,-0.541379696464929,
-0.54034790464077,-0.539422391453723,-0.538165316578795,-0.53525542811576,
-0.521588208206566,-0.520367955699403,-0.500877068977447),.UNSPECIFIED.);
#134=B_SPLINE_CURVE_WITH_KNOTS('',3,(#14069,#14070,#14071,#14072,#14073,
#14074,#14075,#14076,#14077,#14078,#14079,#14080,#14081,#14082,#14083,#14084,
#14085,#14086,#14087,#14088,#14089,#14090,#14091,#14092,#14093,#14094,#14095,
#14096,#14097,#14098,#14099,#14100,#14101,#14102,#14103,#14104,#14105,#14106,
#14107,#14108,#14109,#14110,#14111,#14112,#14113,#14114,#14115,#14116,#14117,
#14118,#14119,#14120,#14121,#14122,#14123,#14124,#14125,#14126,#14127,#14128,
#14129,#14130,#14131,#14132,#14133,#14134,#14135,#14136,#14137,#14138,#14139,
#14140,#14141,#14142,#14143,#14144,#14145,#14146,#14147,#14148,#14149,#14150,
#14151,#14152,#14153,#14154),.UNSPECIFIED.,.F.,.F.,(4,2,2,2,2,2,2,2,2,2,
2,2,2,2,2,2,2,2,2,2,2,2,2,2,2,2,2,2,2,2,2,2,2,2,2,2,2,2,2,2,2,2,4),(-0.241930398828716,
-0.236030777710632,-0.226733379673806,-0.223851838207649,-0.222062618520919,
-0.220414816114051,-0.218250273248799,-0.213520901960721,-0.207131320051679,
-0.189383957186124,-0.168039975130289,-0.165100303953539,-0.163928190563805,
-0.163072169454812,-0.162114799096677,-0.16068369811014,-0.156632185875177,
-0.150189965938108,-0.120410251049439,-0.109746059779745,-0.10672139934979,
-0.104900996526418,-0.103332497948253,-0.103306634631637,-0.103283079484542,
-0.103261571819152,-0.103241888231602,-0.103223836103087,-0.103207248426598,
-0.101152458394976,-0.0988694582598129,-0.0950861695135606,-0.0872136052399747,
-0.0732081983171117,-0.0506943593190284,-0.0478117360807718,-0.0466493677125125,
-0.0457109884765509,-0.0447299449399655,-0.043189075351825,-0.0382407101216464,
-0.0296575430855296,-0.000340887607588386),.UNSPECIFIED.);
#135=B_SPLINE_CURVE_WITH_KNOTS('',3,(#14155,#14156,#14157,#14158,#14159,
#14160,#14161,#14162,#14163,#14164,#14165,#14166,#14167,#14168,#14169,#14170,
#14171,#14172,#14173,#14174,#14175,#14176,#14177,#14178,#14179,#14180,#14181,
#14182,#14183,#14184,#14185,#14186,#14187,#14188,#14189,#14190,#14191,#14192,
#14193,#14194,#14195,#14196,#14197,#14198,#14199,#14200,#14201,#14202,#14203,
#14204,#14205,#14206,#14207,#14208,#14209,#14210,#14211,#14212,#14213,#14214,
#14215,#14216,#14217,#14218,#14219,#14220,#14221,#14222,#14223,#14224,#14225,
#14226,#14227,#14228,#14229,#14230,#14231,#14232,#14233,#14234,#14235,#14236,
#14237,#14238,#14239,#14240,#14241,#14242,#14243,#14244,#14245,#14246,#14247,
#14248,#14249,#14250,#14251,#14252,#14253,#14254,#14255,#14256,#14257,#14258,
#14259,#14260,#14261,#14262,#14263,#14264,#14265,#14266,#14267,#14268,#14269,
#14270,#14271,#14272,#14273,#14274,#14275,#14276,#14277,#14278,#14279,#14280,
#14281,#14282,#14283,#14284,#14285,#14286,#14287,#14288,#14289,#14290,#14291,
#14292,#14293,#14294,#14295,#14296,#14297,#14298,#14299,#14300,#14301,#14302,
#14303,#14304,#14305,#14306,#14307,#14308,#14309,#14310,#14311,#14312,#14313,
#14314,#14315,#14316,#14317,#14318,#14319,#14320,#14321,#14322),
 .UNSPECIFIED.,.F.,.F.,(4,2,2,2,2,2,2,2,2,2,2,2,2,2,2,2,2,2,2,2,2,2,2,2,
2,2,2,2,2,2,2,2,2,2,2,2,2,2,2,2,2,2,2,2,2,2,2,2,2,2,2,2,2,2,2,2,2,2,2,2,
2,2,2,2,2,2,2,2,2,2,2,2,2,2,2,2,2,2,2,2,2,2,2,4),(-1.48407147707552,-1.4790909783933,
-1.47552715703634,-1.47352482305757,-1.47194833101917,-1.47034635659878,
-1.4685079991126,-1.46539794028517,-1.45400345281321,-1.43736318535139,
-1.42229969830208,-1.41759374585316,-1.41437540724622,-1.41306733397175,
-1.41213419424307,-1.41125138989792,-1.40971269039337,-1.4052154374298,
-1.38197576830077,-1.36708654208165,-1.36132868007556,-1.35828361202568,
-1.35630302639214,-1.35444807712028,-1.35441075395009,-1.35438404447419,
-1.35434839771111,-1.35430089420225,-1.35423771987009,-1.35260070759151,
-1.35051423600606,-1.34619971912901,-1.31722927351408,-1.30438688378277,
-1.3000976789732,-1.29709594987043,-1.29582364817088,-1.29489635488629,
-1.29387289591846,-1.29213837136344,-1.28592357030251,-1.26044102864552,
-1.24400063263759,-1.23971836295991,-1.23763807212472,-1.23600171912073,
-1.23417097500079,-1.23109577963338,-1.2198137612674,-1.19068249310705,
-1.18428749829588,-1.1802582803677,-1.17883066470394,-1.17787439638152,
-1.17701840178138,-1.17584513137495,-1.17289633343534,-1.15183681683752,
-1.13393219598776,-1.12751223259252,-1.12276578595968,-1.12059886078464,
-1.11895143336478,-1.11716474983886,-1.11429201068576,-1.10506891768792,
-1.07371463983628,-1.06716795273734,-1.06307052272857,-1.06163369569907,
-1.0606754293168,-1.05982086589987,-1.05865358525953,-1.05570893263915,
-1.03427270514195,-1.01662276563985,-1.01025452117868,-1.00553732112314,
-1.00337555510661,-1.00172872608649,-0.999939449474906,-0.997055347208688,
-0.987726305082495,-0.983796640571424),.UNSPECIFIED.);
#136=B_SPLINE_CURVE_WITH_KNOTS('',3,(#14328,#14329,#14330,#14331,#14332,
#14333,#14334,#14335,#14336,#14337,#14338,#14339,#14340,#14341,#14342,#14343,
#14344,#14345,#14346,#14347,#14348,#14349,#14350,#14351,#14352,#14353,#14354,
#14355,#14356,#14357,#14358,#14359,#14360,#14361,#14362,#14363,#14364,#14365,
#14366,#14367,#14368,#14369,#14370,#14371,#14372,#14373,#14374,#14375,#14376,
#14377,#14378,#14379,#14380,#14381,#14382,#14383,#14384,#14385,#14386,#14387,
#14388,#14389,#14390,#14391,#14392,#14393,#14394,#14395,#14396,#14397,#14398,
#14399,#14400,#14401,#14402,#14403,#14404,#14405,#14406,#14407,#14408,#14409,
#14410,#14411,#14412,#14413,#14414,#14415,#14416,#14417,#14418,#14419,#14420,
#14421,#14422,#14423,#14424,#14425,#14426,#14427,#14428,#14429,#14430,#14431,
#14432,#14433,#14434,#14435,#14436,#14437,#14438,#14439,#14440,#14441,#14442,
#14443,#14444,#14445,#14446,#14447,#14448,#14449,#14450,#14451,#14452,#14453,
#14454,#14455,#14456,#14457,#14458,#14459,#14460,#14461,#14462,#14463,#14464,
#14465,#14466,#14467,#14468,#14469),.UNSPECIFIED.,.F.,.F.,(4,2,2,2,2,2,
2,2,2,2,2,2,2,2,2,2,2,2,2,2,2,2,2,2,2,2,2,2,2,2,2,2,2,2,2,2,2,2,2,2,2,2,
2,2,2,2,2,2,2,2,2,2,2,2,2,2,2,2,2,2,2,2,2,2,2,2,2,2,2,2,4),(-0.500788288135055,
-0.496909354727288,-0.478680433900642,-0.466447740647992,-0.464559682535318,
-0.463389837901927,-0.462474075256743,-0.461388860785006,-0.459371407150183,
-0.446733164115451,-0.420481786771817,-0.409606337946016,-0.406561886638268,
-0.404737161680746,-0.403098476802607,-0.401004598713318,-0.396655266018663,
-0.37969380555784,-0.361595782739146,-0.34922615319291,-0.347332784727044,
-0.346161375301015,-0.345245530777721,-0.344161568575389,-0.342149922601397,
-0.329692324407078,-0.304265428489965,-0.292514625806624,-0.289398183819507,
-0.287557806495867,-0.286085613975019,-0.284097920639864,-0.280285955260957,
-0.275444443779777,-0.264105184209276,-0.239336172959036,-0.231587122966427,
-0.229744667455211,-0.228686337190252,-0.227859286584675,-0.226701936589741,
-0.224331604643313,-0.221180620352351,-0.213283079077864,-0.189854511167829,
-0.175584056578841,-0.172344009085957,-0.170457959602764,-0.168827347211825,
-0.166825814556085,-0.162946053922135,-0.139120171130376,-0.115988816610384,
-0.11314887626941,-0.111993849950166,-0.111057381226991,-0.110097381673065,
-0.108653323487789,-0.106907414114786,-0.103555806048688,-0.0948840478971227,
-0.0677948597840799,-0.0577437969955115,-0.0547791176815606,-0.0529717654812986,
-0.0513290927820337,-0.0492025294706793,-0.0446799493256032,-0.038650987578759,
-0.0225883152000793,-0.000340897761007594),.UNSPECIFIED.);
#137=B_SPLINE_CURVE_WITH_KNOTS('',3,(#14470,#14471,#14472,#14473,#14474,
#14475,#14476,#14477,#14478,#14479,#14480,#14481,#14482,#14483,#14484,#14485,
#14486,#14487,#14488,#14489,#14490,#14491,#14492,#14493,#14494,#14495,#14496,
#14497,#14498,#14499,#14500,#14501,#14502,#14503,#14504,#14505,#14506,#14507,
#14508,#14509,#14510,#14511,#14512,#14513,#14514,#14515,#14516,#14517,#14518,
#14519,#14520,#14521,#14522,#14523,#14524,#14525,#14526,#14527,#14528,#14529,
#14530,#14531,#14532,#14533,#14534,#14535,#14536,#14537,#14538,#14539,#14540,
#14541,#14542,#14543,#14544,#14545,#14546,#14547),.UNSPECIFIED.,.F.,.F.,
(4,2,2,2,2,2,2,2,2,2,2,2,2,2,2,2,2,2,2,2,2,2,2,2,2,2,2,2,2,2,2,2,2,2,2,
2,2,2,4),(-1.48455615980153,-1.48089708969997,-1.47968395763997,-1.4787722523958,
-1.47788529481661,-1.47685546778224,-1.47509360323038,-1.46860266426421,
-1.44904999241366,-1.42643989038457,-1.42250204588403,-1.42048886317402,
-1.41885762515121,-1.41698068554125,-1.41378048487863,-1.40020837790193,
-1.36764652902101,-1.36470621038258,-1.36311232939687,-1.36174386184975,
-1.36080885508367,-1.35995009368449,-1.35876716690521,-1.35576310396599,
-1.33847287578786,-1.32405686844856,-1.30801987050693,-1.30476309763374,
-1.30289215387842,-1.30126008789132,-1.29923808401619,-1.29611450644146,
-1.2734675517998,-1.25596220523273,-1.24984023003476,-1.24593478228138,
-1.24452352177923,-1.24357022908271,-1.24297181640774),.UNSPECIFIED.);
#138=B_SPLINE_CURVE_WITH_KNOTS('',3,(#14548,#14549,#14550,#14551,#14552,
#14553,#14554,#14555,#14556,#14557,#14558,#14559,#14560,#14561,#14562,#14563,
#14564,#14565,#14566,#14567,#14568,#14569,#14570,#14571,#14572,#14573,#14574,
#14575,#14576,#14577,#14578,#14579,#14580,#14581,#14582,#14583,#14584,#14585,
#14586,#14587,#14588,#14589,#14590,#14591,#14592,#14593,#14594,#14595,#14596,
#14597,#14598,#14599,#14600,#14601,#14602,#14603,#14604,#14605,#14606,#14607,
#14608,#14609,#14610,#14611,#14612,#14613,#14614,#14615,#14616,#14617,#14618,
#14619,#14620,#14621,#14622,#14623,#14624,#14625,#14626,#14627,#14628,#14629,
#14630,#14631,#14632,#14633,#14634,#14635,#14636,#14637,#14638,#14639,#14640,
#14641,#14642,#14643,#14644,#14645,#14646,#14647,#14648,#14649,#14650,#14651,
#14652,#14653,#14654,#14655,#14656,#14657,#14658,#14659,#14660,#14661,#14662,
#14663,#14664,#14665,#14666,#14667,#14668,#14669,#14670,#14671,#14672,#14673,
#14674,#14675,#14676,#14677,#14678,#14679,#14680,#14681,#14682,#14683,#14684,
#14685,#14686,#14687,#14688,#14689,#14690,#14691,#14692,#14693,#14694,#14695,
#14696,#14697,#14698,#14699,#14700,#14701,#14702,#14703,#14704,#14705,#14706,
#14707,#14708,#14709,#14710,#14711,#14712,#14713,#14714,#14715,#14716,#14717,
#14718,#14719,#14720,#14721,#14722,#14723,#14724,#14725,#14726,#14727,#14728,
#14729,#14730,#14731,#14732,#14733,#14734,#14735,#14736,#14737,#14738,#14739,
#14740,#14741,#14742,#14743,#14744,#14745,#14746,#14747,#14748,#14749,#14750,
#14751,#14752,#14753,#14754,#14755,#14756,#14757,#14758,#14759),
 .UNSPECIFIED.,.F.,.F.,(4,2,2,2,2,2,2,2,2,2,2,2,2,2,2,2,2,2,2,2,2,2,2,2,
2,2,2,2,2,2,2,2,2,2,2,2,2,2,2,2,2,2,2,2,2,2,2,2,2,2,2,2,2,2,2,2,2,2,2,2,
2,2,2,2,2,2,2,2,2,2,2,2,2,2,2,2,2,2,2,2,2,2,2,2,2,2,2,2,2,2,2,2,2,2,2,2,
2,2,2,2,2,2,2,2,2,4),(-0.983796640571424,-0.956484794984907,-0.949944706224993,
-0.945850105421087,-0.944413564360419,-0.943455292227012,-0.942600572183522,
-0.941432888196903,-0.938485894045167,-0.917121734564788,-0.899418311752801,
-0.893038811419795,-0.88831510415133,-0.886152027165743,-0.884504877476798,
-0.882715914037039,-0.879833785882569,-0.870525286050787,-0.845548739859668,
-0.829864258257799,-0.82777253067057,-0.826671879735262,-0.82575746806048,
-0.824607478999084,-0.822785013169212,-0.81237046940453,-0.803900200100683,
-0.789504457661509,-0.773447392466685,-0.770190480607822,-0.768319900147278,
-0.76668841426212,-0.764667473836552,-0.761546211520125,-0.742126035063395,
-0.726823660385851,-0.712717872011902,-0.710802251117728,-0.709624367250383,
-0.708708248563234,-0.707629599368523,-0.705642172186622,-0.693882110996864,
-0.670390058445014,-0.65625735219468,-0.653025475071441,-0.651141589867197,
-0.649511301017205,-0.647508202153237,-0.643619083800875,-0.638652123600562,
-0.626860425760855,-0.605122493345096,-0.595277921221457,-0.593311584848066,
-0.592225386162393,-0.591309986041854,-0.590142152273994,-0.587717226415944,
-0.584472119735296,-0.576214832546439,-0.551777586066478,-0.538899720414151,
-0.535746188117545,-0.533880096667625,-0.532263729264438,-0.530244116587985,
-0.526273029294609,-0.500340623458418,-0.479655883960697,-0.476688786868871,
-0.475512217167811,-0.474655218551756,-0.47369952324976,-0.472275684724341,
-0.468276441904958,-0.461949318945634,-0.448093225921893,-0.424050549859257,
-0.419405242711111,-0.41727941243655,-0.415632226890008,-0.413842603034745,
-0.41095803020165,-0.400603862745452,-0.380372589738605,-0.362498810863909,
-0.359486817239056,-0.358302750155167,-0.357443849481546,-0.356490331972412,
-0.355077070195199,-0.351155292513191,-0.344997992333697,-0.327616840066378,
-0.304934852970566,-0.301812321839301,-0.299790926043583,-0.298159322798514,
-0.296288882116425,-0.293032934138176,-0.277003245726646,-0.262571998948119,
-0.254080382760505,-0.243662255563251,-0.24188530259165),.UNSPECIFIED.);
#139=B_SPLINE_CURVE_WITH_KNOTS('',3,(#14764,#14765,#14766,#14767,#14768,
#14769,#14770,#14771,#14772,#14773,#14774,#14775,#14776,#14777,#14778,#14779,
#14780,#14781,#14782,#14783,#14784,#14785,#14786,#14787,#14788,#14789,#14790,
#14791,#14792,#14793,#14794,#14795,#14796,#14797,#14798,#14799,#14800,#14801,
#14802,#14803,#14804,#14805,#14806,#14807,#14808,#14809,#14810,#14811,#14812,
#14813,#14814,#14815,#14816,#14817,#14818,#14819,#14820,#14821,#14822,#14823,
#14824,#14825,#14826,#14827,#14828,#14829,#14830,#14831,#14832,#14833,#14834,
#14835,#14836,#14837,#14838,#14839,#14840,#14841,#14842,#14843,#14844,#14845,
#14846,#14847,#14848,#14849,#14850,#14851,#14852,#14853,#14854,#14855,#14856,
#14857,#14858,#14859,#14860,#14861,#14862,#14863,#14864,#14865,#14866,#14867,
#14868,#14869,#14870,#14871,#14872,#14873,#14874,#14875,#14876,#14877,#14878,
#14879,#14880,#14881,#14882,#14883,#14884,#14885,#14886,#14887,#14888,#14889,
#14890,#14891,#14892,#14893,#14894,#14895,#14896,#14897,#14898,#14899,#14900,
#14901,#14902,#14903,#14904,#14905,#14906,#14907,#14908,#14909,#14910,#14911,
#14912,#14913,#14914,#14915,#14916,#14917,#14918,#14919,#14920,#14921,#14922,
#14923,#14924,#14925,#14926,#14927,#14928,#14929,#14930,#14931,#14932,#14933,
#14934,#14935,#14936,#14937,#14938,#14939,#14940,#14941,#14942,#14943,#14944,
#14945,#14946,#14947,#14948,#14949,#14950,#14951,#14952,#14953,#14954,#14955,
#14956,#14957,#14958,#14959,#14960,#14961,#14962,#14963,#14964,#14965,#14966,
#14967,#14968,#14969,#14970,#14971,#14972,#14973,#14974,#14975,#14976,#14977,
#14978,#14979),.UNSPECIFIED.,.F.,.F.,(4,2,2,2,2,2,2,2,2,2,2,2,2,2,2,2,2,
2,2,2,2,2,2,2,2,2,2,2,2,2,2,2,2,2,2,2,2,2,2,2,2,2,2,2,2,2,2,2,2,2,2,2,2,
2,2,2,2,2,2,2,2,2,2,2,2,2,2,2,2,2,2,2,2,2,2,2,2,2,2,2,2,2,2,2,2,2,2,2,2,
2,2,2,2,2,2,2,2,2,2,2,2,2,2,2,2,2,2,4),(-1.24270960294557,-1.23057108915488,
-1.22732602055169,-1.22545793559639,-1.22382609545871,-1.22180143006595,
-1.21866808826137,-1.19670716888601,-1.18091872095959,-1.16959477406654,
-1.16762361808609,-1.1665484792736,-1.16563203873022,-1.16444947668023,
-1.16251793232035,-1.14714449873207,-1.13194244786246,-1.11516132864751,
-1.11083508105137,-1.10874599200114,-1.10710826866319,-1.10528173937671,
-1.10222742295277,-1.09123775839418,-1.06179496057393,-1.05537591847317,
-1.05133551768838,-1.04990613702097,-1.04894930113395,-1.04809314592959,
-1.04692024190248,-1.04397172484588,-1.02285705837319,-1.0049812210747,
-0.998566005281528,-0.993821732748724,-0.991654546968834,-0.990006406352709,
-0.988218442563936,-0.985342508731116,-0.97609767273325,-0.951067149571288,
-0.935361831899937,-0.933269228074998,-0.932168172877487,-0.931253496325791,
-0.930103229502069,-0.928280329786855,-0.917862539400722,-0.90938655183576,
-0.894974554798651,-0.878939289563961,-0.875682893889256,-0.873812168213393,
-0.872180293451031,-0.870158528136357,-0.867035324269992,-0.844343705568824,
-0.826954044235385,-0.820789956984208,-0.816865292766497,-0.815451497226935,
-0.814497774347033,-0.813638796843363,-0.81245477007217,-0.809443611488359,
-0.79055008858818,-0.771103730870406,-0.764382522453055,-0.759466137497427,
-0.757268230294995,-0.755615560299651,-0.753840706857694,-0.751025005139501,
-0.742323621541982,-0.726847220848381,-0.701984995824586,-0.6992058495356,
-0.697985057490443,-0.697061701628054,-0.696022507756908,-0.694218220923099,
-0.686193343773232,-0.666884545894673,-0.644867787040151,-0.641736354619933,
-0.639712033490797,-0.638079902981726,-0.636210862666873,-0.632962531176757,
-0.617105597930535,-0.592701098365589,-0.58345111678198,-0.581515406698485,
-0.580435884016506,-0.579519528268489,-0.578341981854396,-0.575867831930763,
-0.572537620133231,-0.563950201397443,-0.537604989793406,-0.526838664232318,
-0.523795011014158,-0.521970419909316,-0.52033163855543,-0.518237337911599,
-0.513886018832894,-0.500788288135055),.UNSPECIFIED.);
#140=B_SPLINE_CURVE_WITH_KNOTS('',3,(#14981,#14982,#14983,#14984,#14985,
#14986,#14987,#14988,#14989,#14990,#14991,#14992,#14993,#14994,#14995,#14996,
#14997,#14998,#14999,#15000,#15001,#15002,#15003,#15004,#15005,#15006,#15007,
#15008,#15009,#15010,#15011,#15012,#15013,#15014,#15015,#15016,#15017,#15018,
#15019,#15020,#15021,#15022,#15023,#15024,#15025,#15026,#15027,#15028,#15029,
#15030,#15031,#15032,#15033,#15034,#15035,#15036,#15037,#15038,#15039,#15040,
#15041,#15042,#15043,#15044,#15045,#15046,#15047,#15048,#15049,#15050,#15051,
#15052,#15053,#15054,#15055,#15056,#15057,#15058,#15059,#15060,#15061,#15062),
 .UNSPECIFIED.,.F.,.F.,(4,2,2,2,2,2,2,2,2,2,2,2,2,2,2,2,2,2,2,2,2,2,2,2,
2,2,2,2,2,2,2,2,2,2,2,2,2,2,2,2,4),(-0.24188530259165,-0.241839450645931,
-0.240689330117789,-0.239774862237138,-0.238674196696723,-0.236582597120152,
-0.220900822173211,-0.195927396293197,-0.186632072550096,-0.183751225943813,
-0.181962448638454,-0.180315060969418,-0.178151073629708,-0.173422960231241,
-0.167035107506178,-0.149292817673318,-0.127952574016593,-0.125014146572647,
-0.123842412036512,-0.122986626178238,-0.12204872217306,-0.120665006406587,
-0.119049417498415,-0.116050969259377,-0.108718177744274,-0.0926687435394361,
-0.070491433295743,-0.0673729381326236,-0.0653527843429346,-0.063721292694102,
-0.0618500015231068,-0.0585900309526913,-0.042472028592819,-0.0142557204442416,
-0.00858106725857966,-0.00690303169297602,-0.00589177633641331,-0.00501456269788023,
-0.00409375962618727,-0.00241338029616013,-0.000340362829803059),
 .UNSPECIFIED.);
#141=B_SPLINE_CURVE_WITH_KNOTS('',3,(#15063,#15064,#15065,#15066,#15067,
#15068,#15069,#15070,#15071,#15072,#15073,#15074,#15075,#15076,#15077,#15078,
#15079,#15080,#15081,#15082,#15083,#15084,#15085,#15086,#15087,#15088,#15089,
#15090,#15091,#15092,#15093,#15094,#15095,#15096,#15097,#15098,#15099,#15100,
#15101,#15102,#15103,#15104,#15105,#15106,#15107,#15108,#15109,#15110,#15111,
#15112,#15113,#15114,#15115,#15116,#15117,#15118,#15119,#15120,#15121,#15122,
#15123,#15124,#15125,#15126,#15127,#15128,#15129,#15130,#15131,#15132,#15133,
#15134,#15135,#15136,#15137,#15138,#15139,#15140,#15141,#15142,#15143,#15144,
#15145,#15146,#15147,#15148,#15149,#15150,#15151,#15152,#15153,#15154,#15155,
#15156,#15157,#15158,#15159,#15160,#15161,#15162,#15163,#15164,#15165,#15166,
#15167,#15168,#15169,#15170,#15171,#15172,#15173,#15174,#15175,#15176,#15177),
 .UNSPECIFIED.,.F.,.F.,(4,3,3,3,3,3,3,3,3,3,3,3,3,3,3,3,3,3,3,3,3,3,3,3,
3,3,3,3,3,3,3,3,3,3,3,3,3,3,4),(128.805298797898,128.924201779237,129.04293631556,
129.161556862562,129.280117685512,129.398763030493,129.517442715942,129.636360823461,
129.752144419847,129.876237071814,129.995823262841,130.115290601643,130.234691807728,
130.354079486213,130.473588015411,130.593169388511,130.712965709663,130.744885635581,
130.868978287548,130.988564690371,131.108032242172,131.227433662028,131.346821554623,
131.466330296828,131.585911882519,131.705708413522,131.737626851315,131.861719503282,
131.981305172712,132.100771992196,132.220172682235,132.339559848936,132.45906787637,
132.578648753008,132.698444590347,132.730368067049,132.850162253262,132.969754580808,
133.043149374429),.UNSPECIFIED.);
#142=B_SPLINE_CURVE_WITH_KNOTS('',3,(#15183,#15184,#15185,#15186,#15187,
#15188,#15189,#15190,#15191,#15192,#15193,#15194,#15195,#15196,#15197,#15198,
#15199,#15200,#15201,#15202,#15203,#15204,#15205,#15206,#15207,#15208,#15209,
#15210,#15211,#15212,#15213,#15214,#15215,#15216,#15217,#15218,#15219,#15220,
#15221,#15222,#15223,#15224,#15225,#15226,#15227,#15228,#15229,#15230,#15231,
#15232,#15233,#15234,#15235,#15236,#15237,#15238,#15239,#15240,#15241,#15242,
#15243,#15244,#15245,#15246,#15247,#15248,#15249,#15250,#15251,#15252,#15253,
#15254,#15255,#15256,#15257,#15258,#15259,#15260,#15261,#15262,#15263,#15264,
#15265,#15266,#15267,#15268,#15269,#15270,#15271,#15272,#15273,#15274,#15275,
#15276,#15277,#15278,#15279,#15280,#15281,#15282,#15283,#15284,#15285,#15286,
#15287,#15288,#15289,#15290,#15291,#15292,#15293,#15294),.UNSPECIFIED.,
 .F.,.F.,(4,3,3,3,3,3,3,3,3,3,3,3,3,3,3,3,3,3,3,3,3,3,3,3,3,3,3,3,3,3,3,
3,3,3,3,3,3,4),(135.088484104826,135.235310991762,135.372911768261,135.497004420228,
135.616616883007,135.73611026417,135.855537234829,135.974950351382,136.094483653774,
136.214089438881,136.333909405395,136.365652983995,136.489745635962,136.609369624872,
136.728875103783,136.848314712737,136.967740977844,137.087288072282,137.206908039,
137.326742605226,137.358394199729,137.482486851696,137.601899867957,137.721194162145,
137.84042278402,137.959638669042,138.078977825563,138.19839104728,138.318022674585,
138.351135415463,138.472970870233,138.592784589194,138.712476256388,138.832098163482,
138.955528386017,139.075242304231,139.200530678927,139.325819053623),
 .UNSPECIFIED.);
#143=B_SPLINE_CURVE_WITH_KNOTS('',3,(#15295,#15296,#15297,#15298,#15299,
#15300,#15301,#15302,#15303,#15304,#15305,#15306,#15307,#15308,#15309,#15310,
#15311,#15312,#15313,#15314,#15315,#15316,#15317,#15318,#15319,#15320,#15321,
#15322,#15323,#15324,#15325,#15326,#15327,#15328,#15329,#15330,#15331,#15332,
#15333,#15334,#15335,#15336,#15337,#15338,#15339,#15340,#15341,#15342,#15343,
#15344,#15345,#15346,#15347,#15348,#15349,#15350,#15351,#15352,#15353,#15354,
#15355,#15356,#15357,#15358,#15359,#15360,#15361,#15362,#15363,#15364,#15365,
#15366,#15367,#15368,#15369,#15370,#15371,#15372,#15373,#15374,#15375,#15376,
#15377,#15378,#15379,#15380,#15381,#15382,#15383,#15384,#15385,#15386,#15387,
#15388,#15389,#15390,#15391,#15392,#15393,#15394,#15395,#15396,#15397,#15398),
 .UNSPECIFIED.,.F.,.F.,(4,2,2,2,2,2,2,2,2,2,2,2,2,2,2,2,2,2,2,2,2,2,2,2,
2,2,2,2,2,2,2,2,2,2,2,2,2,2,2,2,2,2,2,2,2,2,2,2,2,2,2,4),(-1.48431867888129,
-1.4667432062449,-1.46372645311139,-1.46175797776396,-1.46019207361964,
-1.45856261866385,-1.45668983668337,-1.45350196093862,-1.44009136080204,
-1.4263596585778,-1.41496328252652,-1.404029850154,-1.40203099020675,-1.40095061468933,
-1.40003509582519,-1.39886102772239,-1.39695859516784,-1.38363937752364,
-1.36747010047829,-1.35446538446697,-1.34917344444698,-1.34511944004517,
-1.34314400077368,-1.34313291116912,-1.34312119108408,-1.34310880227671,
-1.34309570394019,-1.34308185249518,-1.34306720138911,-1.34305170085914,
-1.34303529767782,-1.34301793488256,-1.34299955147528,-1.34298008210286,
-1.34295945670407,-1.34293760012776,-1.34291443172066,-1.34144236516171,
-1.3395974673014,-1.33646176715407,-1.3244389990526,-1.29922619837416,-1.29085256337213,
-1.2875770389686,-1.28513440788799,-1.28396260013633,-1.28304646209334,
-1.28196223494932,-1.28000539409258,-1.27034980175605,-1.2463741601058,
-1.24270960294557),.UNSPECIFIED.);
#144=B_SPLINE_CURVE_WITH_KNOTS('',3,(#15400,#15401,#15402,#15403,#15404,
#15405,#15406,#15407,#15408,#15409,#15410,#15411,#15412,#15413,#15414,#15415,
#15416,#15417,#15418,#15419,#15420,#15421,#15422,#15423,#15424,#15425,#15426,
#15427,#15428,#15429,#15430,#15431,#15432,#15433,#15434,#15435,#15436,#15437,
#15438,#15439,#15440,#15441,#15442,#15443,#15444,#15445,#15446,#15447,#15448,
#15449,#15450,#15451,#15452,#15453,#15454),.UNSPECIFIED.,.F.,.F.,(4,3,3,
3,3,3,3,3,3,3,3,3,3,3,3,3,3,3,4),(133.043149374429,133.162572277305,133.281959474831,
133.401451670163,133.520996801097,133.640772313025,133.723109282783,133.84720193475,
133.966789439693,134.086258097906,134.205660626244,134.325049627171,134.444559469222,
134.564142150987,134.683939761574,134.715850498517,134.851214190363,134.985564663725,
135.088484103629),.UNSPECIFIED.);
#145=B_SPLINE_CURVE_WITH_KNOTS('',3,(#15455,#15456,#15457,#15458,#15459,
#15460,#15461,#15462,#15463,#15464,#15465,#15466,#15467,#15468,#15469,#15470,
#15471,#15472,#15473,#15474,#15475,#15476,#15477,#15478,#15479,#15480,#15481,
#15482,#15483,#15484,#15485,#15486,#15487,#15488,#15489,#15490,#15491,#15492,
#15493,#15494,#15495,#15496,#15497,#15498,#15499,#15500,#15501,#15502,#15503,
#15504,#15505,#15506,#15507,#15508,#15509,#15510,#15511,#15512,#15513,#15514,
#15515,#15516,#15517,#15518,#15519,#15520,#15521,#15522,#15523,#15524,#15525,
#15526,#15527,#15528,#15529,#15530,#15531,#15532,#15533,#15534,#15535,#15536,
#15537,#15538,#15539,#15540,#15541,#15542,#15543,#15544,#15545,#15546,#15547,
#15548,#15549,#15550,#15551,#15552,#15553,#15554,#15555,#15556,#15557,#15558,
#15559,#15560,#15561,#15562,#15563,#15564,#15565,#15566,#15567,#15568,#15569,
#15570,#15571,#15572,#15573,#15574,#15575,#15576,#15577,#15578,#15579,#15580,
#15581,#15582,#15583,#15584,#15585,#15586,#15587,#15588,#15589,#15590,#15591,
#15592,#15593,#15594,#15595,#15596,#15597,#15598,#15599,#15600,#15601,#15602,
#15603,#15604,#15605,#15606,#15607,#15608,#15609,#15610,#15611,#15612,#15613,
#15614,#15615,#15616,#15617,#15618,#15619,#15620,#15621,#15622,#15623,#15624,
#15625,#15626,#15627,#15628,#15629,#15630),.UNSPECIFIED.,.F.,.F.,(4,2,2,
2,2,2,2,2,2,2,2,2,2,2,2,2,2,2,2,2,2,2,2,2,2,2,2,2,2,2,2,2,2,2,2,2,2,2,2,
2,2,2,2,2,2,2,2,2,2,2,2,2,2,2,2,2,2,2,2,2,2,2,2,2,2,2,2,2,2,2,2,2,2,2,2,
2,2,2,2,2,2,2,2,2,2,2,2,4),(0.500726922102148,0.512053449536436,0.515135237800579,
0.516968195480732,0.518441729180792,0.520440786485293,0.524307895967392,
0.529237734536915,0.540890162523225,0.559827955558004,0.563368821419012,
0.572753881272379,0.574695973166796,0.575776446253112,0.576691552793251,
0.57786488463665,0.580322056859391,0.583624206918134,0.592106616308757,
0.617744957846055,0.629294310569344,0.632388093721572,0.63422195242595,
0.635692707788795,0.63768336756942,0.641517930563704,0.646397038493051,
0.657875033052619,0.671538479196515,0.676843014242143,0.683403133368924,
0.690269330375383,0.692062247539759,0.693097959669159,0.69402122377621,
0.695266605018847,0.698111072722151,0.711150880215098,0.720448642156198,
0.743915549589254,0.748575275676725,0.750704046190909,0.75235202460641,
0.754141040194108,0.757021416462893,0.767324890412671,0.787379695059129,
0.805413291061802,0.808429734647613,0.809614810110556,0.810474230127405,
0.811427641817489,0.812840413066334,0.816758895748538,0.822910060012445,
0.8403048847854,0.862990676082221,0.866114028152321,0.868135430836476,0.869766713769115,
0.869798997363329,0.869823226361995,0.869860125153782,0.86989484839628,
0.86992752877563,0.869958290853728,0.871853904361353,0.875321569590384,
0.879661674174444,0.889288037155004,0.904766569068977,0.92261703224887,
0.925627836315947,0.926811451732629,0.927670036347477,0.928623170320318,
0.930035840011454,0.933955717604712,0.94011048814423,0.968114063101643,
0.979419476580892,0.982960671678051,0.985083168893455,0.986729295537634,
0.988255585788787,0.990013618796802,0.992513189891128,1.00100352361353),
 .UNSPECIFIED.);
#146=B_SPLINE_CURVE_WITH_KNOTS('',3,(#15636,#15637,#15638,#15639,#15640,
#15641),.UNSPECIFIED.,.F.,.F.,(4,1,1,4),(-4.09202352044853,-3.97096486293603,
-2.97822364720202,-2.0736150725356),.UNSPECIFIED.);
#147=B_SPLINE_CURVE_WITH_KNOTS('',3,(#15644,#15645,#15646,#15647,#15648),
 .UNSPECIFIED.,.F.,.F.,(4,1,4),(0.,0.992741215733998,1.12274180646084),
 .UNSPECIFIED.);
#148=B_SPLINE_CURVE_WITH_KNOTS('',3,(#15653,#15654,#15655,#15656,#15657,
#15658,#15659,#15660,#15661,#15662),.UNSPECIFIED.,.F.,.F.,(4,1,1,1,1,1,
1,4),(-10.3752088276281,-9.92741215734008,-8.93467094160607,-7.94192972587206,
-6.94918851013805,-5.95644729440404,-4.96370607867004,-4.09202352044853),
 .UNSPECIFIED.);
#149=B_SPLINE_CURVE_WITH_KNOTS('',3,(#15663,#15664,#15665,#15666,#15667,
#15668,#15669,#15670,#15671,#15672,#15673,#15674,#15675,#15676,#15677,#15678,
#15679,#15680,#15681,#15682,#15683,#15684,#15685,#15686,#15687,#15688,#15689,
#15690,#15691,#15692,#15693,#15694,#15695,#15696,#15697,#15698,#15699,#15700,
#15701,#15702,#15703,#15704,#15705,#15706,#15707,#15708,#15709,#15710,#15711,
#15712,#15713,#15714,#15715,#15716,#15717,#15718,#15719,#15720,#15721,#15722,
#15723,#15724,#15725,#15726,#15727,#15728,#15729,#15730,#15731,#15732,#15733,
#15734,#15735,#15736,#15737,#15738,#15739,#15740,#15741,#15742,#15743,#15744,
#15745,#15746,#15747,#15748,#15749,#15750,#15751,#15752,#15753,#15754,#15755,
#15756,#15757,#15758,#15759,#15760,#15761,#15762,#15763,#15764,#15765,#15766,
#15767,#15768,#15769,#15770,#15771,#15772,#15773,#15774,#15775,#15776,#15777,
#15778,#15779,#15780,#15781,#15782,#15783,#15784,#15785,#15786,#15787,#15788,
#15789,#15790,#15791,#15792,#15793,#15794,#15795,#15796,#15797,#15798,#15799,
#15800,#15801,#15802,#15803,#15804,#15805,#15806,#15807,#15808,#15809,#15810,
#15811,#15812,#15813,#15814,#15815,#15816,#15817,#15818,#15819,#15820,#15821,
#15822,#15823,#15824,#15825,#15826,#15827,#15828,#15829,#15830,#15831,#15832,
#15833,#15834),.UNSPECIFIED.,.F.,.F.,(4,3,3,3,3,3,3,3,3,3,3,3,3,3,3,3,3,
3,3,3,3,3,3,3,3,3,3,3,3,3,3,3,3,3,3,3,3,3,3,3,3,3,3,3,3,3,3,3,3,3,3,3,3,
3,3,3,3,4),(1.12274180646084,1.23343629746888,1.34399240446288,1.45445841687218,
1.56488243774564,1.67539231942886,1.78594226536294,1.89670153729216,1.98548243146801,
2.09914339557329,2.21260275597674,2.32594994134661,2.43922941306601,2.55248553226531,
2.6658428728994,2.77925047355754,2.89286747779434,2.97822364720202,3.09189566254516,
3.20537231958541,3.31874061986118,3.43204499121717,3.54532976590842,3.6587213982951,
3.77216647795867,3.8858257585652,3.97096486293603,4.08428886198503,4.19740786099008,
4.31041287767409,4.4233490066995,4.53626124008659,4.6492766385696,4.76234285582213,
4.87562368571185,4.96370607867004,5.07722135155215,5.19053517232557,5.30373703723263,
5.4168716877161,5.5299837652683,5.64319947242412,5.75646656994225,5.86994671152142,
5.95644729440405,6.06994872957337,6.1832492800824,6.29643823328387,6.40956035469253,
6.52266031031201,6.63586462950835,6.74912072961629,6.86259065731568,6.94918851013806,
7.07058093650876,7.19167798873108,7.31234457608894,7.40592711324294),
 .UNSPECIFIED.);
#150=B_SPLINE_CURVE_WITH_KNOTS('',3,(#15839,#15840,#15841,#15842,#15843,
#15844,#15845,#15846,#15847,#15848),.UNSPECIFIED.,.F.,.F.,(4,1,1,1,1,1,
1,4),(-16.6583930095603,-15.8838594517441,-14.8911182360101,-13.8983770202761,
-12.9056358045421,-11.9128945888081,-10.9201533730741,-10.3752088276281),
 .UNSPECIFIED.);
#151=B_SPLINE_CURVE_WITH_KNOTS('',3,(#15849,#15850,#15851,#15852,#15853,
#15854,#15855,#15856,#15857,#15858,#15859,#15860,#15861,#15862,#15863,#15864,
#15865,#15866,#15867,#15868,#15869,#15870,#15871,#15872,#15873,#15874,#15875,
#15876,#15877,#15878,#15879,#15880,#15881,#15882,#15883,#15884,#15885,#15886,
#15887,#15888,#15889,#15890,#15891,#15892,#15893,#15894,#15895,#15896,#15897,
#15898,#15899,#15900,#15901,#15902,#15903,#15904,#15905,#15906,#15907,#15908,
#15909,#15910,#15911,#15912,#15913,#15914,#15915,#15916,#15917,#15918,#15919,
#15920,#15921,#15922,#15923,#15924,#15925,#15926,#15927,#15928,#15929,#15930,
#15931,#15932,#15933,#15934,#15935,#15936,#15937,#15938,#15939,#15940,#15941,
#15942,#15943,#15944,#15945,#15946,#15947,#15948,#15949,#15950,#15951,#15952,
#15953,#15954,#15955,#15956,#15957,#15958,#15959,#15960,#15961,#15962,#15963,
#15964,#15965,#15966,#15967,#15968,#15969,#15970,#15971,#15972,#15973,#15974,
#15975,#15976,#15977,#15978,#15979,#15980,#15981,#15982,#15983,#15984,#15985,
#15986,#15987,#15988,#15989,#15990,#15991,#15992,#15993,#15994,#15995,#15996,
#15997,#15998,#15999,#16000,#16001,#16002,#16003,#16004,#16005,#16006,#16007,
#16008,#16009,#16010,#16011,#16012,#16013,#16014,#16015,#16016,#16017,#16018,
#16019,#16020),.UNSPECIFIED.,.F.,.F.,(4,3,3,3,3,3,3,3,3,3,3,3,3,3,3,3,3,
3,3,3,3,3,3,3,3,3,3,3,3,3,3,3,3,3,3,3,3,3,3,3,3,3,3,3,3,3,3,3,3,3,3,3,3,
3,3,3,3,4),(7.40592711364043,7.52253753703482,7.63939496513354,7.75638371478664,
7.87366366059931,7.94192972587207,8.05541582244172,8.16870031392625,8.28187277923307,
8.39497801395519,8.5080607136396,8.62124733990233,8.7344854771366,8.84793722088447,
8.93467094160608,9.04815243188051,9.16143233640877,9.2746002302422,9.38770091736713,
9.50077910174122,9.61396129959615,9.72719504990304,9.84064253031215,9.92741215734009,
10.0408880929723,10.1541622655264,10.2673243231986,10.3804190806018,10.4934912521889,
10.606667356083,10.7198949579502,10.8333362768889,10.9201533730741,11.0336337732337,
11.1469125068194,11.2600791810862,11.3731786022268,11.4862554763447,11.5994363053865,
11.7126686522404,11.8261146895023,11.9128945888081,12.0263739592526,12.1396516566805,
12.2528172916576,12.3659156722783,12.4789915065442,12.5921713051742,12.7054026252761,
12.8188476547086,12.9056358045421,13.0175005710598,13.1292059416967,13.2407992579844,
13.352877548586,13.4644294254286,13.5767709229096,13.6891124203907),
 .UNSPECIFIED.);
#152=B_SPLINE_CURVE_WITH_KNOTS('',3,(#16025,#16026,#16027,#16028,#16029,
#16030,#16031,#16032,#16033,#16034,#16035,#16036,#16037,#16038,#16039,#16040,
#16041,#16042,#16043,#16044,#16045,#16046,#16047,#16048,#16049,#16050,#16051,
#16052,#16053,#16054,#16055,#16056,#16057,#16058,#16059,#16060,#16061,#16062,
#16063,#16064,#16065,#16066,#16067,#16068,#16069,#16070,#16071,#16072,#16073,
#16074,#16075,#16076,#16077,#16078,#16079,#16080,#16081,#16082,#16083,#16084,
#16085,#16086,#16087,#16088,#16089,#16090,#16091,#16092,#16093,#16094,#16095,
#16096,#16097,#16098,#16099,#16100,#16101,#16102,#16103,#16104,#16105,#16106,
#16107,#16108,#16109,#16110,#16111,#16112,#16113,#16114,#16115,#16116,#16117,
#16118,#16119,#16120,#16121,#16122,#16123,#16124,#16125,#16126,#16127,#16128,
#16129,#16130,#16131,#16132,#16133,#16134,#16135,#16136,#16137,#16138,#16139,
#16140,#16141,#16142,#16143,#16144,#16145,#16146,#16147,#16148,#16149,#16150,
#16151,#16152,#16153,#16154,#16155,#16156,#16157,#16158,#16159,#16160,#16161,
#16162,#16163,#16164,#16165,#16166,#16167,#16168,#16169,#16170,#16171,#16172,
#16173,#16174,#16175,#16176,#16177,#16178,#16179,#16180,#16181,#16182,#16183,
#16184,#16185,#16186,#16187,#16188,#16189,#16190,#16191,#16192,#16193,#16194,
#16195,#16196),.UNSPECIFIED.,.F.,.F.,(4,3,3,3,3,3,3,3,3,3,3,3,3,3,3,3,3,
3,3,3,3,3,3,3,3,3,3,3,3,3,3,3,3,3,3,3,3,3,3,3,3,3,3,3,3,3,3,3,3,3,3,3,3,
3,3,3,3,4),(-22.9415794419873,-22.8330479618822,-22.7195687858932,-22.6062912943685,
-22.4931258721497,-22.3800277107567,-22.2669521018115,-22.1537725361979,
-22.040541453747,-21.9270966666516,-21.8403067461482,-21.7268275697863,
-21.613550077918,-21.500384655374,-21.3872864936743,-21.2742108844412,-21.1610313185711,
-21.0478002358805,-20.9343554485756,-20.8475655304142,-20.734086348015,
-20.6208088500747,-20.5076434214419,-20.3945452536477,-20.2814696383254,
-20.1682900664222,-20.0550589777206,-19.9416141845158,-19.8548243146802,
-19.7413451461789,-19.6280676621022,-19.5149022473017,-19.4018040932847,
-19.2887284916603,-19.1755489332253,-19.0623178578849,-18.9488730777009,
-18.8620830989462,-18.7486039233986,-18.6353264324728,-18.5221610109485,
-18.4090628503432,-18.2959872422765,-18.1828076776731,-18.0695765963069,
-17.9561318104028,-17.8693418832121,-17.7558626720325,-17.642585145189,
-17.5294196875997,-17.4163214908473,-17.3032458466163,-17.1900662461109,
-17.0768351289333,-16.9633903078139,-16.8766006674781,-16.7220057020924,
-16.6583941348077),.UNSPECIFIED.);
#153=B_SPLINE_CURVE_WITH_KNOTS('',3,(#16197,#16198,#16199,#16200,#16201,
#16202,#16203,#16204,#16205,#16206,#16207,#16208,#16209,#16210,#16211,#16212,
#16213,#16214,#16215,#16216,#16217,#16218,#16219,#16220,#16221,#16222,#16223,
#16224,#16225,#16226,#16227,#16228,#16229,#16230,#16231,#16232,#16233,#16234,
#16235,#16236,#16237,#16238,#16239,#16240,#16241,#16242,#16243,#16244,#16245,
#16246,#16247,#16248,#16249,#16250,#16251,#16252,#16253,#16254,#16255,#16256,
#16257,#16258,#16259,#16260,#16261,#16262,#16263,#16264,#16265,#16266,#16267,
#16268,#16269,#16270,#16271,#16272,#16273,#16274,#16275,#16276,#16277,#16278,
#16279,#16280,#16281,#16282,#16283,#16284,#16285,#16286,#16287,#16288,#16289,
#16290,#16291,#16292,#16293,#16294,#16295,#16296,#16297,#16298,#16299,#16300,
#16301,#16302,#16303,#16304,#16305,#16306,#16307,#16308,#16309,#16310,#16311,
#16312,#16313,#16314,#16315,#16316,#16317,#16318,#16319,#16320,#16321,#16322,
#16323,#16324,#16325,#16326,#16327,#16328,#16329,#16330,#16331,#16332,#16333,
#16334,#16335,#16336,#16337,#16338,#16339,#16340,#16341,#16342,#16343,#16344,
#16345,#16346,#16347,#16348,#16349,#16350,#16351,#16352,#16353,#16354,#16355,
#16356,#16357,#16358,#16359,#16360,#16361,#16362,#16363,#16364,#16365,#16366,
#16367,#16368),.UNSPECIFIED.,.F.,.F.,(4,3,3,3,3,3,3,3,3,3,3,3,3,3,3,3,3,
3,3,3,3,3,3,3,3,3,3,3,3,3,3,3,3,3,3,3,3,3,3,3,3,3,3,3,3,3,3,3,3,3,3,3,3,
3,3,3,3,4),(13.68911242082,13.84668731327,13.8983770202761,14.0118564019841,
14.125134102677,14.2382997360134,14.3513981100881,14.4644739328963,14.577653712491,
14.6908850093181,14.8043300087562,14.8911182360101,15.0045974196722,15.1178749200623,
15.2310403518703,15.3441385235596,15.4572141434919,15.5703937210833,15.6836248160808,
15.7970696165069,15.8838594517441,15.9973385684418,16.1106159990213,16.2237813593291,
16.3368794579583,16.4499550033988,16.5631345048636,16.6763655227092,16.7898102452546,
16.8766006674781,16.9900798773989,17.1033574034607,17.2165228605604,17.3296210571146,
17.4426967014383,17.5558763024844,17.6691074204524,17.7825522427601,17.8693418832121,
17.9828210580819,18.0960985485814,18.2092639698335,18.3223621303203,18.4354377384218,
18.5486173032965,18.6618483850657,18.7752931715828,18.8620830989461,18.9755622681843,
19.0888397527214,19.202005167813,19.3151033219523,19.4281789235304,19.5413584816595,
19.6545895565493,19.768034336052,19.8548243146801,19.9722977279996),
 .UNSPECIFIED.);
#154=B_SPLINE_CURVE_WITH_KNOTS('',3,(#16373,#16374,#16375,#16376,#16377,
#16378,#16379,#16380,#16381,#16382),.UNSPECIFIED.,.F.,.F.,(4,1,1,1,1,1,
1,4),(-29.2247647491669,-28.7894952562862,-27.7967540405522,-26.8040128248182,
-25.8112716090842,-24.8185303933502,-23.8257891776162,-22.9415879141924),
 .UNSPECIFIED.);
#155=B_SPLINE_CURVE_WITH_KNOTS('',3,(#16383,#16384,#16385,#16386,#16387,
#16388,#16389,#16390,#16391,#16392),.UNSPECIFIED.,.F.,.F.,(4,1,1,1,1,1,
1,4),(19.9723060732156,20.8475655304142,21.8403067461482,22.8330479618822,
23.8257891776162,24.8185303933502,25.8112716090842,26.2554830351792),
 .UNSPECIFIED.);
#156=B_SPLINE_CURVE_WITH_KNOTS('',3,(#16397,#16398,#16399,#16400,#16401,
#16402,#16403,#16404,#16405,#16406),.UNSPECIFIED.,.F.,.F.,(4,1,1,1,1,1,
1,4),(-35.5079500563465,-34.7459425506903,-33.7532013349563,-32.7604601192223,
-31.7677189034882,-30.7749776877542,-29.7822364720202,-29.2247647491669),
 .UNSPECIFIED.);
#157=B_SPLINE_CURVE_WITH_KNOTS('',3,(#16407,#16408,#16409,#16410,#16411,
#16412,#16413,#16414,#16415,#16416),.UNSPECIFIED.,.F.,.F.,(4,1,1,1,1,1,
1,4),(26.2554830351792,26.8040128248182,27.7967540405522,28.7894952562862,
29.7822364720202,30.7749776877543,31.7677189034883,32.5386675302423),
 .UNSPECIFIED.);
#158=B_SPLINE_CURVE_WITH_KNOTS('',3,(#16421,#16422,#16423,#16424,#16425,
#16426,#16427,#16428,#16429,#16430,#16431),.UNSPECIFIED.,.F.,.F.,(4,1,1,
1,1,1,1,1,4),(-41.791135363526,-41.6951310608283,-40.7023898450943,-39.7096486293603,
-38.7169074136263,-37.7241661978923,-36.7314249821583,-35.7386837664243,
-35.5079500563465),.UNSPECIFIED.);
#159=B_SPLINE_CURVE_WITH_KNOTS('',3,(#16432,#16433,#16434,#16435,#16436,
#16437,#16438,#16439,#16440,#16441,#16442,#16443,#16444,#16445,#16446,#16447,
#16448,#16449,#16450,#16451,#16452,#16453,#16454,#16455,#16456,#16457,#16458,
#16459,#16460,#16461,#16462,#16463,#16464,#16465,#16466,#16467,#16468,#16469,
#16470,#16471,#16472,#16473,#16474,#16475,#16476,#16477,#16478,#16479,#16480,
#16481,#16482,#16483,#16484,#16485,#16486,#16487,#16488,#16489,#16490,#16491,
#16492,#16493,#16494,#16495,#16496,#16497,#16498,#16499,#16500,#16501,#16502,
#16503,#16504,#16505,#16506,#16507,#16508,#16509,#16510,#16511,#16512,#16513,
#16514,#16515,#16516,#16517,#16518,#16519,#16520,#16521,#16522,#16523,#16524,
#16525,#16526,#16527,#16528,#16529,#16530,#16531,#16532,#16533,#16534,#16535,
#16536,#16537,#16538,#16539,#16540,#16541,#16542,#16543,#16544,#16545,#16546,
#16547,#16548,#16549,#16550,#16551,#16552,#16553,#16554,#16555,#16556,#16557,
#16558,#16559,#16560,#16561,#16562,#16563,#16564,#16565,#16566,#16567,#16568,
#16569,#16570,#16571,#16572,#16573,#16574,#16575,#16576,#16577,#16578,#16579,
#16580,#16581,#16582,#16583,#16584,#16585,#16586,#16587,#16588,#16589,#16590,
#16591,#16592,#16593,#16594,#16595,#16596,#16597,#16598,#16599,#16600,#16601,
#16602,#16603),.UNSPECIFIED.,.F.,.F.,(4,3,3,3,3,3,3,3,3,3,3,3,3,3,3,3,3,
3,3,3,3,3,3,3,3,3,3,3,3,3,3,3,3,3,3,3,3,3,3,3,3,3,3,3,3,3,3,3,3,3,3,3,3,
3,3,3,3,4),(32.5386683423588,32.6921491728441,32.7604601192223,32.8739392962833,
32.9872167888717,33.1003822121482,33.2134803745913,33.3265559845771,33.4397355512085,
33.5529666346662,33.6664114227379,33.7532013349563,33.8666805120183,33.9799580046077,
34.0931234278852,34.2062215903293,34.3192972003161,34.4324767669485,34.5457078504072,
34.6591526384799,34.7459425506903,34.8594217277526,34.9726992203424,35.0858646436203,
35.1989628060648,35.312038416052,35.4252179826848,35.5384490661439,35.651893854217,
35.7386837664243,35.8521629434862,35.9654404360755,36.0786058593529,36.1917040217968,
36.3047796317836,36.4179591984159,36.5311902818745,36.6446350699471,36.7314249821583,
36.8449041592204,36.9581816518098,37.0713470750875,37.1844452375316,37.2975208475185,
37.4107004141509,37.5239314976098,37.6373762856826,37.7241661978923,37.8376453749544,
37.9509228675439,38.0640882908215,38.1771864532657,38.2902620632527,38.4034416298852,
38.516672713344,38.6301175014168,38.7169074136263,38.8218536495384),
 .UNSPECIFIED.);
#160=B_SPLINE_CURVE_WITH_KNOTS('',3,(#16608,#16609,#16610,#16611,#16612,
#16613,#16614,#16615,#16616,#16617,#16618,#16619,#16620,#16621,#16622,#16623,
#16624,#16625,#16626,#16627,#16628,#16629,#16630,#16631,#16632,#16633,#16634,
#16635,#16636,#16637,#16638,#16639,#16640,#16641,#16642,#16643,#16644,#16645,
#16646,#16647,#16648,#16649,#16650,#16651,#16652,#16653,#16654,#16655,#16656,
#16657,#16658,#16659,#16660,#16661,#16662,#16663,#16664,#16665,#16666,#16667,
#16668,#16669,#16670,#16671,#16672,#16673,#16674,#16675,#16676,#16677,#16678,
#16679,#16680,#16681,#16682,#16683,#16684,#16685,#16686,#16687,#16688,#16689,
#16690,#16691,#16692,#16693,#16694,#16695,#16696,#16697,#16698,#16699,#16700,
#16701,#16702,#16703,#16704,#16705,#16706,#16707,#16708,#16709,#16710,#16711,
#16712,#16713,#16714,#16715,#16716,#16717,#16718,#16719,#16720,#16721,#16722,
#16723,#16724,#16725,#16726,#16727,#16728,#16729,#16730,#16731,#16732,#16733,
#16734,#16735,#16736,#16737,#16738,#16739,#16740,#16741,#16742,#16743,#16744,
#16745,#16746,#16747,#16748,#16749,#16750,#16751,#16752,#16753,#16754,#16755,
#16756,#16757,#16758,#16759,#16760,#16761,#16762,#16763,#16764,#16765,#16766,
#16767,#16768,#16769,#16770,#16771,#16772,#16773,#16774,#16775,#16776,#16777,
#16778,#16779),.UNSPECIFIED.,.F.,.F.,(4,3,3,3,3,3,3,3,3,3,3,3,3,3,3,3,3,
3,3,3,3,3,3,3,3,3,3,3,3,3,3,3,3,3,3,3,3,3,3,3,3,3,3,3,3,3,3,3,3,3,3,3,3,
3,3,3,3,4),(-48.0743203223387,-47.9513556297491,-47.8280197994362,-47.7041579646634,
-47.6515783552324,-47.5380991781703,-47.4248216855808,-47.3116562623032,
-47.198558099859,-47.0854824898721,-46.9723029232396,-46.8590718397807,
-46.7456270517079,-46.6588371394984,-46.5453579624364,-46.4320804698469,
-46.3189150465693,-46.2058168841252,-46.0927412741383,-45.9795617075059,
-45.8663306240471,-45.7528858359743,-45.6660959237644,-45.5526167467024,
-45.439339254113,-45.3261738308354,-45.2130756683913,-45.1000000584044,
-44.9868204917719,-44.8735894083132,-44.7601446202404,-44.6733547080304,
-44.5598755309683,-44.4465980383788,-44.3334326151012,-44.220334452657,
-44.1072588426701,-43.9940792760376,-43.8808481925788,-43.767403404506,
-43.6806134922963,-43.5671343152342,-43.4538568226448,-43.3406913993672,
-43.2275932369231,-43.1145176269361,-43.0013380603037,-42.8881069768448,
-42.774662188772,-42.6878722765623,-42.5757801624328,-42.4638771065427,
-42.3520829463607,-42.2403507815932,-42.1280469270764,-42.0162357828843,
-41.9036855732051,-41.791135363526),.UNSPECIFIED.);
#161=B_SPLINE_CURVE_WITH_KNOTS('',3,(#16780,#16781,#16782,#16783,#16784,
#16785,#16786,#16787,#16788,#16789,#16790,#16791,#16792,#16793,#16794,#16795,
#16796,#16797,#16798,#16799,#16800,#16801,#16802,#16803,#16804,#16805,#16806,
#16807,#16808,#16809,#16810,#16811,#16812,#16813,#16814,#16815,#16816,#16817,
#16818,#16819,#16820,#16821,#16822,#16823,#16824,#16825,#16826,#16827,#16828,
#16829,#16830,#16831,#16832,#16833,#16834,#16835,#16836,#16837,#16838,#16839,
#16840,#16841,#16842,#16843,#16844,#16845,#16846,#16847,#16848,#16849,#16850,
#16851,#16852,#16853,#16854,#16855,#16856,#16857,#16858,#16859,#16860,#16861,
#16862,#16863,#16864,#16865,#16866,#16867,#16868,#16869,#16870,#16871,#16872,
#16873,#16874,#16875,#16876,#16877,#16878,#16879,#16880,#16881,#16882,#16883,
#16884,#16885,#16886,#16887,#16888,#16889,#16890,#16891,#16892,#16893,#16894,
#16895,#16896,#16897,#16898,#16899,#16900,#16901,#16902,#16903,#16904,#16905,
#16906,#16907,#16908,#16909,#16910,#16911,#16912,#16913,#16914,#16915,#16916,
#16917,#16918,#16919,#16920,#16921,#16922,#16923,#16924,#16925,#16926,#16927,
#16928,#16929,#16930,#16931,#16932,#16933,#16934,#16935,#16936,#16937,#16938,
#16939,#16940,#16941,#16942,#16943,#16944,#16945,#16946,#16947,#16948,#16949,
#16950,#16951),.UNSPECIFIED.,.F.,.F.,(4,3,3,3,3,3,3,3,3,3,3,3,3,3,3,3,3,
3,3,3,3,3,3,3,3,3,3,3,3,3,3,3,3,3,3,3,3,3,3,3,3,3,3,3,3,3,3,3,3,3,3,3,3,
3,3,3,3,4),(38.8218536499681,38.9337807794497,39.0455700846134,39.1572686518211,
39.2689234195268,39.3806624113741,39.492437953727,39.6044275384719,39.7096486293603,
39.8231278064224,39.9364052990119,40.0495707222895,40.1626688847337,40.2757444947207,
40.3889240613532,40.5021551448119,40.6155999328847,40.7023898450943,40.8158690221565,
40.9291465147459,41.0423119380236,41.1554101004677,41.2684857104546,41.381665277087,
41.4948963605459,41.6083411486187,41.6951310608283,41.8086102378904,41.9218877304799,
42.0350531537575,42.1481513162015,42.2612269261883,42.3744064928208,42.4876375762796,
42.6010823643523,42.6878722765623,42.8013514536243,42.9146289462136,43.0277943694913,
43.1408925319353,43.2539681419224,43.3671477085548,43.4803787920136,43.5938235800864,
43.6806134922963,43.7940926693583,43.9073701619478,44.0205355852255,44.1336337476696,
44.2467093576563,44.3598889242888,44.4731200077475,44.5865647958202,44.6733547080304,
44.7964919319002,44.919285871168,45.0415576688195,45.1050386426266),
 .UNSPECIFIED.);
#162=B_SPLINE_CURVE_WITH_KNOTS('',3,(#16956,#16957,#16958,#16959,#16960,
#16961,#16962,#16963,#16964,#16965),.UNSPECIFIED.,.F.,.F.,(4,1,1,1,1,1,
1,4),(-54.3575059778852,-53.6080256496364,-52.6152844339024,-51.6225432181684,
-50.6298020024344,-49.6370607867004,-48.6443195709664,-48.0743206707056),
 .UNSPECIFIED.);
#163=B_SPLINE_CURVE_WITH_KNOTS('',3,(#16966,#16967,#16968,#16969,#16970,
#16971,#16972,#16973,#16974,#16975),.UNSPECIFIED.,.F.,.F.,(4,1,1,1,1,1,
1,4),(45.105038956718,45.6660959237644,46.6588371394984,47.6515783552324,
48.6443195709664,49.6370607867004,50.6298020024344,51.3882242638976),
 .UNSPECIFIED.);
#164=B_SPLINE_CURVE_WITH_KNOTS('',3,(#16980,#16981,#16982,#16983,#16984,
#16985,#16986,#16987,#16988,#16989,#16990),.UNSPECIFIED.,.F.,.F.,(4,1,1,
1,1,1,1,1,4),(-60.6406912850648,-60.5572141597745,-59.5644729440405,-58.5717317283065,
-57.5789905125725,-56.5862492968384,-55.5935080811044,-54.6007668653704,
-54.3575059778852),.UNSPECIFIED.);
#165=B_SPLINE_CURVE_WITH_KNOTS('',3,(#16991,#16992,#16993,#16994,#16995,
#16996,#16997,#16998,#16999,#17000,#17001),.UNSPECIFIED.,.F.,.F.,(4,1,1,
1,1,1,1,1,4),(51.3882242638976,51.6225432181684,52.6152844339024,53.6080256496364,
54.6007668653704,55.5935080811044,56.5862492968384,57.5789905125724,57.6714095710771),
 .UNSPECIFIED.);
#166=B_SPLINE_CURVE_WITH_KNOTS('',3,(#17006,#17007,#17008,#17009,#17010,
#17011,#17012,#17013,#17014,#17015),.UNSPECIFIED.,.F.,.F.,(4,1,1,1,1,1,
1,4),(-66.9238707158243,-66.5136614541785,-65.5209202384445,-64.5281790227105,
-63.5354378069765,-62.5426965912425,-61.5499553755085,-60.6406912850648),
 .UNSPECIFIED.);
#167=B_SPLINE_CURVE_WITH_KNOTS('',3,(#17016,#17017,#17018,#17019,#17020,
#17021,#17022,#17023,#17024,#17025,#17026,#17027,#17028,#17029,#17030,#17031,
#17032,#17033,#17034,#17035,#17036,#17037,#17038,#17039,#17040,#17041,#17042,
#17043,#17044,#17045,#17046,#17047,#17048,#17049,#17050,#17051,#17052,#17053,
#17054,#17055,#17056,#17057,#17058,#17059,#17060,#17061,#17062,#17063,#17064,
#17065,#17066,#17067,#17068,#17069,#17070,#17071,#17072,#17073,#17074,#17075,
#17076,#17077,#17078,#17079,#17080,#17081,#17082,#17083,#17084,#17085,#17086,
#17087,#17088,#17089,#17090,#17091,#17092,#17093,#17094,#17095,#17096,#17097,
#17098,#17099,#17100,#17101,#17102,#17103,#17104,#17105,#17106,#17107,#17108,
#17109,#17110,#17111,#17112,#17113,#17114,#17115,#17116,#17117,#17118,#17119,
#17120,#17121,#17122,#17123,#17124,#17125,#17126,#17127,#17128,#17129,#17130,
#17131,#17132,#17133,#17134,#17135,#17136,#17137,#17138,#17139,#17140,#17141,
#17142,#17143,#17144,#17145,#17146,#17147,#17148,#17149,#17150,#17151,#17152,
#17153,#17154,#17155,#17156,#17157,#17158,#17159,#17160,#17161,#17162,#17163,
#17164,#17165,#17166,#17167,#17168,#17169,#17170,#17171,#17172,#17173,#17174,
#17175,#17176,#17177,#17178,#17179,#17180,#17181,#17182,#17183,#17184,#17185,
#17186,#17187),.UNSPECIFIED.,.F.,.F.,(4,3,3,3,3,3,3,3,3,3,3,3,3,3,3,3,3,
3,3,3,3,3,3,3,3,3,3,3,3,3,3,3,3,3,3,3,3,3,3,3,3,3,3,3,3,3,3,3,3,3,3,3,3,
3,3,3,3,4),(57.6714095710771,57.7839498407308,57.8958482195883,58.0076522188625,
58.1194086610543,58.2324894278674,58.3443610884006,58.4580464083536,58.5717317283065,
58.6852109053686,58.798488397958,58.9116538212356,59.0247519836798,59.1378275936667,
59.2510071602991,59.3642382437579,59.4776830318307,59.5644729440405,59.6779521211026,
59.791229613692,59.9043950369696,60.0174931994137,60.1305688094004,60.2437483760328,
60.3569794594915,60.4704242475643,60.5572141597745,60.6706933368365,60.783970829426,
60.8971362527036,61.0102344151477,61.1233100251347,61.2364895917672,61.349720675226,
61.4631654632988,61.5499553755085,61.6634345525706,61.7767120451601,61.8898774684378,
62.0029756308819,62.1160512408686,62.2292308075011,62.3424618909597,62.4559066790326,
62.5426965912425,62.6561757683045,62.7694532608939,62.8826186841715,62.9957168466155,
63.1087924566024,63.2219720232348,63.3352031066935,63.4486478947663,63.5354378069765,
63.6595194390276,63.7832273544186,63.9063594692533,63.9545948779103),
 .UNSPECIFIED.);
#168=B_SPLINE_CURVE_WITH_KNOTS('',3,(#17192,#17193,#17194,#17195,#17196,
#17197,#17198,#17199,#17200,#17201,#17202,#17203,#17204,#17205,#17206,#17207,
#17208,#17209,#17210,#17211,#17212,#17213,#17214,#17215,#17216,#17217,#17218,
#17219,#17220,#17221,#17222,#17223,#17224,#17225,#17226,#17227,#17228,#17229,
#17230,#17231,#17232,#17233,#17234,#17235,#17236,#17237,#17238,#17239,#17240,
#17241,#17242,#17243,#17244,#17245,#17246,#17247,#17248,#17249,#17250,#17251,
#17252,#17253,#17254,#17255,#17256,#17257,#17258,#17259,#17260,#17261,#17262,
#17263,#17264,#17265,#17266,#17267,#17268,#17269,#17270,#17271,#17272,#17273,
#17274,#17275,#17276,#17277,#17278,#17279,#17280,#17281,#17282,#17283,#17284,
#17285,#17286,#17287,#17288,#17289,#17290,#17291,#17292,#17293,#17294,#17295,
#17296,#17297,#17298,#17299,#17300,#17301,#17302,#17303,#17304,#17305,#17306,
#17307,#17308,#17309,#17310,#17311,#17312,#17313,#17314,#17315,#17316,#17317,
#17318,#17319,#17320,#17321,#17322,#17323,#17324,#17325,#17326,#17327,#17328,
#17329,#17330,#17331,#17332,#17333,#17334,#17335,#17336,#17337,#17338,#17339,
#17340,#17341,#17342,#17343,#17344,#17345,#17346,#17347,#17348,#17349,#17350,
#17351,#17352,#17353,#17354,#17355,#17356,#17357,#17358,#17359,#17360,#17361,
#17362,#17363),.UNSPECIFIED.,.F.,.F.,(4,3,3,3,3,3,3,3,3,3,3,3,3,3,3,3,3,
3,3,3,3,3,3,3,3,3,3,3,3,3,3,3,3,3,3,3,3,3,3,3,3,3,3,3,3,3,3,3,3,3,3,3,3,
3,3,3,3,4),(-73.207061899424,-73.0950948311733,-72.9831980604613,-72.8713249933925,
-72.7593511740308,-72.6473233814792,-72.5350916115429,-72.4701087485826,
-72.3566295715204,-72.243352078931,-72.1301866556534,-72.0170884932093,
-71.9040128832223,-71.7908333165898,-71.6776022331311,-71.5641574450583,
-71.4773675328486,-71.3638883557865,-71.250610863197,-71.1374454399194,
-71.0243472774753,-70.9112716674884,-70.798092100856,-70.6848610173971,
-70.5714162293243,-70.4846263171145,-70.3711471400525,-70.2578696474631,
-70.1447042241855,-70.0316060617414,-69.9185304517545,-69.8053508851221,
-69.6921198016633,-69.5786750135905,-69.4918851013805,-69.3784059243185,
-69.2651284317291,-69.1519630084515,-69.0388648460074,-68.9257892360203,
-68.8126096693879,-68.6993785859291,-68.5859337978563,-68.4991438856465,
-68.3856647085845,-68.272387215995,-68.1592217927174,-68.0461236302732,
-67.9330480202862,-67.8198684536538,-67.7066373701951,-67.5931925821223,
-67.5064026699125,-67.3908458947149,-67.2741035690973,-67.1589453653598,
-67.0414109788021,-66.9238765922444),.UNSPECIFIED.);
#169=B_SPLINE_CURVE_WITH_KNOTS('',3,(#17364,#17365,#17366,#17367,#17368,
#17369,#17370,#17371,#17372,#17373,#17374,#17375,#17376,#17377,#17378,#17379,
#17380,#17381,#17382,#17383,#17384,#17385,#17386,#17387,#17388,#17389,#17390,
#17391,#17392,#17393,#17394,#17395,#17396,#17397,#17398,#17399,#17400,#17401,
#17402,#17403,#17404,#17405,#17406,#17407,#17408,#17409,#17410,#17411,#17412,
#17413,#17414,#17415,#17416,#17417,#17418,#17419,#17420,#17421,#17422,#17423,
#17424,#17425,#17426,#17427,#17428,#17429,#17430,#17431,#17432,#17433,#17434,
#17435,#17436,#17437,#17438,#17439,#17440,#17441,#17442,#17443,#17444,#17445,
#17446,#17447,#17448,#17449,#17450,#17451,#17452,#17453,#17454,#17455,#17456,
#17457,#17458,#17459,#17460,#17461,#17462,#17463,#17464,#17465,#17466,#17467,
#17468,#17469,#17470,#17471,#17472,#17473,#17474,#17475,#17476,#17477,#17478,
#17479,#17480,#17481,#17482,#17483,#17484,#17485,#17486,#17487,#17488,#17489,
#17490,#17491,#17492,#17493,#17494,#17495,#17496,#17497,#17498,#17499,#17500,
#17501,#17502,#17503,#17504,#17505,#17506,#17507,#17508,#17509,#17510,#17511,
#17512,#17513,#17514,#17515,#17516,#17517,#17518,#17519,#17520,#17521,#17522,
#17523,#17524,#17525,#17526,#17527,#17528,#17529,#17530,#17531,#17532,#17533,
#17534,#17535),.UNSPECIFIED.,.F.,.F.,(4,3,3,3,3,3,3,3,3,3,3,3,3,3,3,3,3,
3,3,3,3,3,3,3,3,3,3,3,3,3,3,3,3,3,3,3,3,3,3,3,3,3,3,3,3,3,3,3,3,3,3,3,3,
3,3,3,3,4),(63.9545948782567,64.0698636722457,64.1853150539345,64.3008548231996,
64.4166721465948,64.5281790227105,64.6416581997725,64.7549356923619,64.8681011156395,
64.9811992780837,65.0942748880707,65.2074544547032,65.320685538162,65.4341303262348,
65.5209202384445,65.6343994155066,65.747676908096,65.8608423313736,65.9739404938177,
66.0870161038044,66.2001956704368,66.3134267538955,66.4268715419683,66.5136614541785,
66.6271406312406,66.74041812383,66.8535835471076,66.9666817095518,67.0797573195387,
67.1929368861711,67.3061679696299,67.4196127577027,67.5064026699125,67.6198818469747,
67.7331593395641,67.8463247628417,67.9594229252858,68.0724985352727,68.1856781019051,
68.298909185364,68.4123539734367,68.4991438856465,68.6126230627086,68.725900555298,
68.8390659785756,68.9521641410198,69.0652397510066,69.1784193176391,69.2916504010978,
69.4050951891706,69.4918851013805,69.6040236394296,69.7159996034553,69.827860005518,
69.9396848486519,70.0514850869985,70.1633755926544,70.2377801854363),
 .UNSPECIFIED.);
#170=B_SPLINE_CURVE_WITH_KNOTS('',3,(#17540,#17541,#17542,#17543,#17544,
#17545,#17546,#17547,#17548,#17549,#17550),.UNSPECIFIED.,.F.,.F.,(4,1,1,
1,1,1,1,1,4),(-79.4902472066036,-79.4192972587206,-78.4265560429866,-77.4338148272526,
-76.4410736115186,-75.4483323957846,-74.4555911800506,-73.4628499643166,
-73.2070640903504),.UNSPECIFIED.);
#171=B_SPLINE_CURVE_WITH_KNOTS('',3,(#17551,#17552,#17553,#17554,#17555,
#17556,#17557,#17558,#17559,#17560,#17561),.UNSPECIFIED.,.F.,.F.,(4,1,1,
1,1,1,1,1,4),(70.2377816044152,70.4846263171145,71.4773675328486,72.4701087485826,
73.4628499643166,74.4555911800506,75.4483323957846,76.4410736115186,76.5209654926159),
 .UNSPECIFIED.);
#172=B_SPLINE_CURVE_WITH_KNOTS('',3,(#17566,#17567,#17568,#17569,#17570,
#17571,#17572,#17573,#17574,#17575),.UNSPECIFIED.,.F.,.F.,(4,1,1,1,1,1,
1,4),(-85.7734325137832,-85.3757445531247,-84.3830033373907,-83.3902621216566,
-82.3975209059226,-81.4047796901886,-80.4120384744546,-79.4902472066036),
 .UNSPECIFIED.);
#173=B_SPLINE_CURVE_WITH_KNOTS('',3,(#17576,#17577,#17578,#17579,#17580,
#17581,#17582,#17583,#17584,#17585),.UNSPECIFIED.,.F.,.F.,(4,1,1,1,1,1,
1,4),(76.5209654926159,77.4338148272526,78.4265560429866,79.4192972587206,
80.4120384744546,81.4047796901886,82.3975209059226,82.8041447673426),
 .UNSPECIFIED.);
#174=B_SPLINE_CURVE_WITH_KNOTS('',3,(#17590,#17591,#17592,#17593,#17594,
#17595,#17596,#17597,#17598,#17599),.UNSPECIFIED.,.F.,.F.,(4,1,1,1,1,1,
1,4),(-92.0566178209628,-91.3321918475287,-90.3394506317947,-89.3467094160607,
-88.3539682003267,-87.3612269845927,-86.3684857688587,-85.7734325137832),
 .UNSPECIFIED.);
#175=B_SPLINE_CURVE_WITH_KNOTS('',3,(#17600,#17601,#17602,#17603,#17604,
#17605,#17606,#17607,#17608,#17609,#17610,#17611,#17612,#17613,#17614,#17615,
#17616,#17617,#17618,#17619,#17620,#17621,#17622,#17623,#17624,#17625,#17626,
#17627,#17628,#17629,#17630,#17631,#17632,#17633,#17634,#17635,#17636,#17637,
#17638,#17639,#17640,#17641,#17642,#17643,#17644,#17645,#17646,#17647,#17648,
#17649,#17650,#17651,#17652,#17653,#17654,#17655,#17656,#17657,#17658,#17659,
#17660,#17661,#17662,#17663,#17664,#17665,#17666,#17667,#17668,#17669,#17670,
#17671,#17672,#17673,#17674,#17675,#17676,#17677,#17678,#17679,#17680,#17681,
#17682,#17683,#17684,#17685,#17686,#17687,#17688,#17689,#17690,#17691,#17692,
#17693,#17694,#17695,#17696,#17697,#17698,#17699,#17700,#17701,#17702,#17703,
#17704,#17705,#17706,#17707,#17708,#17709,#17710,#17711,#17712,#17713,#17714,
#17715,#17716,#17717,#17718,#17719,#17720,#17721,#17722,#17723,#17724,#17725,
#17726,#17727,#17728,#17729,#17730,#17731,#17732,#17733,#17734,#17735,#17736,
#17737,#17738,#17739,#17740,#17741,#17742,#17743,#17744,#17745,#17746,#17747,
#17748,#17749,#17750,#17751,#17752,#17753,#17754,#17755,#17756,#17757,#17758,
#17759,#17760,#17761,#17762,#17763,#17764,#17765,#17766,#17767,#17768,#17769,
#17770,#17771),.UNSPECIFIED.,.F.,.F.,(4,3,3,3,3,3,3,3,3,3,3,3,3,3,3,3,3,
3,3,3,3,3,3,3,3,3,3,3,3,3,3,3,3,3,3,3,3,3,3,3,3,3,3,3,3,3,3,3,3,3,3,3,3,
3,3,3,3,4),(82.8041507997955,82.9190225628796,83.0368324525739,83.1519469049723,
83.2711045133145,83.3902621216566,83.5037412987187,83.6170187913081,83.7301842145858,
83.8432823770299,83.9563579870168,84.0695375536493,84.1827686371081,84.296213425181,
84.3830033373907,84.4964825144529,84.6097600070423,84.7229254303199,84.836023592764,
84.9490992027509,85.0622787693834,85.1755098528421,85.2889546409149,85.3757445531247,
85.4892237301868,85.6025012227762,85.7156666460537,85.8287648084979,85.9418404184848,
86.0550199851172,86.168251068576,86.2816958566488,86.3684857688587,86.4819649459207,
86.5952424385102,86.7084078617878,86.8215060242319,86.9345816342187,87.0477612008512,
87.1609922843099,87.2744370723827,87.3612269845927,87.4747061616548,87.5879836542442,
87.7011490775218,87.8142472399659,87.9273228499528,88.0405024165852,88.1537335000438,
88.2671782881166,88.3539682003267,88.4662367419805,88.5783413179202,88.6903287715849,
88.8022749438312,88.914195125773,89.0261943465739,89.0873361069751),
 .UNSPECIFIED.);
#176=B_SPLINE_CURVE_WITH_KNOTS('',3,(#17776,#17777,#17778,#17779,#17780,
#17781,#17782,#17783,#17784,#17785,#17786,#17787,#17788,#17789,#17790,#17791,
#17792,#17793,#17794,#17795,#17796,#17797,#17798,#17799,#17800,#17801,#17802,
#17803,#17804,#17805,#17806,#17807,#17808,#17809,#17810,#17811,#17812,#17813,
#17814,#17815,#17816,#17817,#17818,#17819,#17820,#17821,#17822,#17823,#17824,
#17825,#17826,#17827,#17828,#17829,#17830,#17831,#17832,#17833,#17834,#17835,
#17836,#17837,#17838,#17839,#17840,#17841,#17842,#17843,#17844,#17845,#17846,
#17847,#17848,#17849,#17850,#17851,#17852,#17853,#17854,#17855,#17856,#17857,
#17858,#17859,#17860,#17861,#17862,#17863,#17864,#17865,#17866,#17867,#17868,
#17869,#17870,#17871,#17872,#17873,#17874,#17875,#17876,#17877,#17878,#17879,
#17880,#17881,#17882,#17883,#17884,#17885,#17886,#17887,#17888,#17889,#17890,
#17891,#17892,#17893,#17894,#17895,#17896,#17897,#17898,#17899,#17900,#17901,
#17902,#17903,#17904,#17905,#17906,#17907,#17908,#17909,#17910,#17911,#17912,
#17913,#17914,#17915,#17916,#17917,#17918,#17919,#17920,#17921,#17922,#17923,
#17924,#17925,#17926,#17927,#17928,#17929,#17930,#17931,#17932,#17933,#17934,
#17935,#17936,#17937,#17938,#17939,#17940,#17941,#17942,#17943,#17944,#17945,
#17946,#17947),.UNSPECIFIED.,.F.,.F.,(4,3,3,3,3,3,3,3,3,3,3,3,3,3,3,3,3,
3,3,3,3,3,3,3,3,3,3,3,3,3,3,3,3,3,3,3,3,3,3,3,3,3,3,3,3,3,3,3,3,3,3,3,3,
3,3,3,3,4),(-98.3398031281424,-98.2813803576668,-98.1679011806047,-98.0546236880152,
-97.9414582647376,-97.8283601022934,-97.7152844923065,-97.602104925674,
-97.4888738422151,-97.3754290541423,-97.2886391419328,-97.1751599648707,
-97.0618824722813,-96.9487170490037,-96.8356188865595,-96.7225432765726,
-96.6093637099401,-96.4961326264813,-96.3826878384085,-96.2958979261987,
-96.1824187491366,-96.0691412565472,-95.9559758332696,-95.8428776708254,
-95.7298020608385,-95.616622494206,-95.5033914107472,-95.3899466226744,
-95.3031567104647,-95.1896775334027,-95.0764000408133,-94.9632346175357,
-94.8501364550915,-94.7370608451047,-94.6238812784722,-94.5106501950134,
-94.3972054069406,-94.3104154947307,-94.1969363176686,-94.0836588250792,
-93.9704934018016,-93.8573952393575,-93.7443196293706,-93.6311400627381,
-93.5179089792793,-93.4044641912065,-93.3176742789967,-93.2041951019346,
-93.0909176093452,-92.9777521860676,-92.8646540236235,-92.7515784136366,
-92.6383988470042,-92.5251677635454,-92.4117229754726,-92.3249330632627,
-92.182832718097,-92.0566180325444),.UNSPECIFIED.);
#177=B_SPLINE_CURVE_WITH_KNOTS('',3,(#17948,#17949,#17950,#17951,#17952,
#17953,#17954,#17955,#17956,#17957,#17958,#17959,#17960,#17961,#17962,#17963,
#17964,#17965,#17966,#17967,#17968,#17969,#17970,#17971,#17972,#17973,#17974,
#17975,#17976,#17977,#17978,#17979,#17980,#17981,#17982,#17983,#17984,#17985,
#17986,#17987,#17988,#17989,#17990,#17991,#17992,#17993,#17994,#17995,#17996,
#17997,#17998,#17999,#18000,#18001,#18002,#18003,#18004,#18005,#18006,#18007,
#18008,#18009,#18010,#18011,#18012,#18013,#18014,#18015,#18016,#18017,#18018,
#18019,#18020,#18021,#18022,#18023,#18024,#18025,#18026,#18027,#18028,#18029,
#18030,#18031,#18032,#18033,#18034,#18035,#18036,#18037,#18038,#18039,#18040,
#18041,#18042,#18043,#18044,#18045,#18046,#18047,#18048,#18049,#18050,#18051,
#18052,#18053,#18054,#18055,#18056,#18057,#18058,#18059,#18060,#18061,#18062,
#18063,#18064,#18065,#18066,#18067,#18068,#18069,#18070,#18071,#18072,#18073,
#18074,#18075,#18076,#18077,#18078,#18079,#18080,#18081,#18082,#18083,#18084,
#18085,#18086,#18087,#18088,#18089,#18090,#18091,#18092,#18093,#18094,#18095,
#18096,#18097,#18098,#18099,#18100,#18101,#18102,#18103,#18104,#18105,#18106,
#18107,#18108,#18109,#18110,#18111,#18112,#18113,#18114,#18115,#18116,#18117,
#18118,#18119),.UNSPECIFIED.,.F.,.F.,(4,3,3,3,3,3,3,3,3,3,3,3,3,3,3,3,3,
3,3,3,3,3,3,3,3,3,3,3,3,3,3,3,3,3,3,3,3,3,3,3,3,3,3,3,3,3,3,3,3,3,3,3,3,
3,3,3,3,4),(89.0873361076021,89.2312652478392,89.3467094160607,89.4601885931227,
89.5734660857121,89.6866315089897,89.7997296714338,89.9128052814207,90.0259848480531,
90.1392159315119,90.2526607195846,90.3394506317947,90.4529298088568,90.5662073014462,
90.6793727247238,90.792470887168,90.9055464971549,91.0187260637874,91.1319571472462,
91.245401935319,91.3321918475287,91.4456710245907,91.5589485171802,91.6721139404578,
91.7852121029019,91.8982877128888,92.0114672795212,92.12469836298,92.2381431510528,
92.3249330632627,92.4384122403248,92.5516897329142,92.6648551561918,92.777953318636,
92.8910289286228,93.0042084952553,93.1174395787141,93.2308843667869,93.3176742789967,
93.4311534560588,93.5444309486482,93.6575963719258,93.7706945343699,93.8837701443568,
93.9969497109893,94.1101807944481,94.2236255825209,94.3104154947307,94.4238946717928,
94.5371721643822,94.6503375876597,94.7634357501038,94.8765113600907,94.9896909267232,
95.1029220101819,95.2163667982547,95.3031567104647,95.3705214141547),
 .UNSPECIFIED.);
#178=B_SPLINE_CURVE_WITH_KNOTS('',3,(#18124,#18125,#18126,#18127,#18128,
#18129,#18130,#18131,#18132,#18133),.UNSPECIFIED.,.F.,.F.,(4,1,1,1,1,1,
1,4),(-104.622988435322,-104.237827652071,-103.245086436337,-102.252345220603,
-101.259604004869,-100.266862789135,-99.2741215734008,-98.3398097557481),
 .UNSPECIFIED.);
#179=B_SPLINE_CURVE_WITH_KNOTS('',3,(#18134,#18135,#18136,#18137,#18138,
#18139,#18140,#18141,#18142,#18143),.UNSPECIFIED.,.F.,.F.,(4,1,1,1,1,1,
1,4),(95.3705286189736,96.2958979261987,97.2886391419327,98.2813803576667,
99.2741215734008,100.266862789135,101.259604004869,101.653706721334),
 .UNSPECIFIED.);
#180=B_SPLINE_CURVE_WITH_KNOTS('',3,(#18148,#18149,#18150,#18151,#18152,
#18153,#18154,#18155,#18156,#18157),.UNSPECIFIED.,.F.,.F.,(4,1,1,1,1,1,
1,4),(-110.906173742502,-110.194274946475,-109.201533730741,-108.208792515007,
-107.216051299273,-106.223310083539,-105.230568867805,-104.622988435322),
 .UNSPECIFIED.);
#181=B_SPLINE_CURVE_WITH_KNOTS('',3,(#18158,#18159,#18160,#18161,#18162,
#18163,#18164,#18165,#18166,#18167),.UNSPECIFIED.,.F.,.F.,(4,1,1,1,1,1,
1,4),(101.653706721334,102.252345220603,103.245086436337,104.237827652071,
105.230568867805,106.223310083539,107.216051299273,107.936892028514),
 .UNSPECIFIED.);
#182=B_SPLINE_CURVE_WITH_KNOTS('',3,(#18172,#18173,#18174,#18175,#18176,
#18177,#18178,#18179,#18180,#18181,#18182),.UNSPECIFIED.,.F.,.F.,(4,1,1,
1,1,1,1,1,4),(-117.189359049681,-117.143463456613,-116.150722240879,-115.157981025145,
-114.165239809411,-113.172498593677,-112.179757377943,-111.187016162209,
-110.906173742502),.UNSPECIFIED.);
#183=B_SPLINE_CURVE_WITH_KNOTS('',3,(#18183,#18184,#18185,#18186,#18187,
#18188,#18189,#18190,#18191,#18192,#18193,#18194,#18195,#18196,#18197,#18198,
#18199,#18200,#18201,#18202,#18203,#18204,#18205,#18206,#18207,#18208,#18209,
#18210,#18211,#18212,#18213,#18214,#18215,#18216,#18217,#18218,#18219,#18220,
#18221,#18222,#18223,#18224,#18225,#18226,#18227,#18228,#18229,#18230,#18231,
#18232,#18233,#18234,#18235,#18236,#18237,#18238,#18239,#18240,#18241,#18242,
#18243,#18244,#18245,#18246,#18247,#18248,#18249,#18250,#18251,#18252,#18253,
#18254,#18255,#18256,#18257,#18258,#18259,#18260,#18261,#18262,#18263,#18264,
#18265,#18266,#18267,#18268,#18269,#18270,#18271,#18272,#18273,#18274,#18275,
#18276,#18277,#18278,#18279,#18280,#18281,#18282,#18283,#18284,#18285,#18286,
#18287,#18288,#18289,#18290,#18291,#18292,#18293,#18294,#18295,#18296,#18297,
#18298,#18299,#18300,#18301,#18302,#18303,#18304,#18305,#18306,#18307,#18308,
#18309,#18310,#18311,#18312,#18313,#18314,#18315,#18316,#18317,#18318,#18319,
#18320,#18321,#18322,#18323,#18324,#18325,#18326,#18327,#18328,#18329,#18330,
#18331,#18332,#18333,#18334,#18335,#18336,#18337,#18338,#18339,#18340,#18341,
#18342,#18343,#18344,#18345,#18346,#18347,#18348,#18349,#18350,#18351,#18352,
#18353,#18354),.UNSPECIFIED.,.F.,.F.,(4,3,3,3,3,3,3,3,3,3,3,3,3,3,3,3,3,
3,3,3,3,3,3,3,3,3,3,3,3,3,3,3,3,3,3,3,3,3,3,3,3,3,3,3,3,3,3,3,3,3,3,3,3,
3,3,3,3,4),(107.936892258894,108.078296789096,108.208792515007,108.322271691942,
108.435549184406,108.548714607559,108.661812769879,108.774888379744,108.888067946257,
109.001299029598,109.114743817557,109.201533730741,109.315012907634,109.428290400052,
109.541455823156,109.654553985425,109.767629595236,109.880809161693,109.994040244975,
110.107485032873,110.194274946475,110.307754124348,110.421031617749,110.534197041838,
110.647295205093,110.760370815887,110.873550383317,110.986781467567,111.100226256415,
111.187016162209,111.300495338197,111.413772829721,111.526938251939,111.640036413331,
111.753112022276,111.866291587889,111.979522670339,112.092967457434,112.179757377943,
112.293236554304,112.406514046172,112.519679468715,112.632777630414,112.745853239646,
112.859032805516,112.972263888206,113.08570867551,113.172498593677,113.28597777608,
113.399255274024,113.512420702661,113.625518870459,113.738594485786,113.851774057693,
113.965005146398,114.078449939607,114.165239809411,114.220077335693),
 .UNSPECIFIED.);
#184=B_SPLINE_CURVE_WITH_KNOTS('',3,(#18359,#18360,#18361,#18362,#18363,
#18364,#18365,#18366,#18367,#18368,#18369,#18370,#18371,#18372,#18373,#18374,
#18375,#18376,#18377,#18378,#18379,#18380,#18381,#18382,#18383,#18384,#18385,
#18386,#18387,#18388,#18389,#18390,#18391,#18392,#18393,#18394,#18395,#18396,
#18397,#18398,#18399,#18400,#18401,#18402,#18403,#18404,#18405,#18406,#18407,
#18408,#18409,#18410,#18411,#18412,#18413,#18414,#18415,#18416,#18417,#18418,
#18419,#18420,#18421,#18422,#18423,#18424,#18425,#18426,#18427,#18428,#18429,
#18430,#18431,#18432,#18433,#18434,#18435,#18436,#18437,#18438,#18439,#18440,
#18441,#18442,#18443,#18444,#18445,#18446,#18447,#18448,#18449,#18450,#18451,
#18452,#18453,#18454,#18455,#18456,#18457,#18458,#18459,#18460,#18461,#18462,
#18463,#18464,#18465,#18466,#18467,#18468,#18469,#18470,#18471,#18472,#18473,
#18474,#18475,#18476,#18477,#18478,#18479,#18480,#18481,#18482,#18483,#18484,
#18485,#18486,#18487,#18488,#18489,#18490,#18491,#18492,#18493,#18494,#18495,
#18496,#18497,#18498,#18499,#18500,#18501,#18502,#18503,#18504,#18505,#18506,
#18507,#18508,#18509,#18510,#18511,#18512,#18513,#18514,#18515,#18516,#18517,
#18518,#18519,#18520,#18521,#18522,#18523,#18524,#18525,#18526,#18527,#18528,
#18529,#18530),.UNSPECIFIED.,.F.,.F.,(4,3,3,3,3,3,3,3,3,3,3,3,3,3,3,3,3,
3,3,3,3,3,3,3,3,3,3,3,3,3,3,3,3,3,3,3,3,3,3,3,3,3,3,3,3,3,3,3,3,3,3,3,3,
3,3,3,3,4),(-123.472543894631,-123.345471929838,-123.217419424173,-123.099910751017,
-122.986430351432,-122.873151618431,-122.759984944753,-122.646885524206,
-122.533808650684,-122.420627822239,-122.307395475983,-122.193949439312,
-122.107169535283,-121.993690164857,-121.880412467451,-121.767246832498,
-121.654148451904,-121.541072617666,-121.427892819067,-121.314661498998,
-121.2012164696,-121.114428319549,-121.000949591505,-120.887672559457,-120.774507603421,
-120.661409914069,-120.548334782179,-120.435155697601,-120.321925099137,
-120.208480794843,-120.121687103815,-120.008207722219,-119.89493002164,
-119.781764388419,-119.66866601446,-119.555590191769,-119.442410412291,
-119.329179115581,-119.215734116259,-119.128945888081,-119.015466704413,
-118.902189204017,-118.789023772204,-118.675925600509,-118.562849980572,
-118.449670402976,-118.336439307975,-118.222994507545,-118.136204672347,
-118.017848969514,-117.905379929234,-117.793018557627,-117.680718733564,
-117.568434433619,-117.45604635478,-117.343597808392,-117.230956823491,
-117.189359049681),.UNSPECIFIED.);
#185=B_SPLINE_CURVE_WITH_KNOTS('',3,(#18531,#18532,#18533,#18534,#18535,
#18536,#18537,#18538,#18539,#18540,#18541,#18542,#18543,#18544,#18545,#18546,
#18547,#18548,#18549,#18550,#18551,#18552,#18553,#18554,#18555,#18556,#18557,
#18558,#18559,#18560,#18561,#18562,#18563,#18564,#18565,#18566,#18567,#18568,
#18569,#18570,#18571,#18572,#18573,#18574,#18575,#18576,#18577,#18578,#18579,
#18580,#18581,#18582,#18583,#18584,#18585,#18586,#18587,#18588,#18589,#18590,
#18591,#18592,#18593,#18594,#18595,#18596,#18597,#18598,#18599,#18600,#18601,
#18602,#18603,#18604,#18605,#18606,#18607,#18608,#18609,#18610,#18611,#18612,
#18613,#18614,#18615,#18616,#18617,#18618,#18619,#18620,#18621,#18622,#18623,
#18624,#18625,#18626,#18627,#18628,#18629,#18630,#18631,#18632,#18633,#18634,
#18635,#18636,#18637,#18638,#18639,#18640,#18641,#18642,#18643,#18644,#18645,
#18646,#18647,#18648,#18649,#18650,#18651,#18652,#18653,#18654,#18655,#18656,
#18657,#18658,#18659,#18660,#18661,#18662,#18663,#18664,#18665,#18666,#18667,
#18668,#18669,#18670,#18671,#18672,#18673,#18674,#18675,#18676,#18677,#18678,
#18679,#18680,#18681,#18682,#18683,#18684,#18685,#18686,#18687,#18688,#18689,
#18690,#18691,#18692,#18693,#18694,#18695,#18696,#18697,#18698,#18699,#18700,
#18701,#18702),.UNSPECIFIED.,.F.,.F.,(4,3,3,3,3,3,3,3,3,3,3,3,3,3,3,3,3,
3,3,3,3,3,3,3,3,3,3,3,3,3,3,3,3,3,3,3,3,3,3,3,3,3,3,3,3,3,3,3,3,3,3,3,3,
3,3,3,3,4),(114.220077336354,114.337315297453,114.449646955625,114.561876294682,
114.674049601546,114.786213071814,114.898486989919,115.010826666534,115.123361222514,
115.157981025145,115.27146020069,115.384737691613,115.497903113135,115.611001273738,
115.724076881802,115.837256446402,115.950487527766,116.063932313667,116.150722240879,
116.26420145208,116.377478978945,116.490644436556,116.60374263333,116.716818277582,
116.829997878109,116.943228995308,117.056673816448,117.143463456613,117.256942568207,
117.370219995584,117.483385353854,117.596483451607,117.709558997331,117.822738500867,
117.935969521779,118.049414248978,118.136204672347,118.249683861986,118.362961366126,
118.476126800321,118.589224973036,118.702300592636,118.815480167802,118.928711259209,
119.042156054185,119.128945888081,119.24242527583,119.355702980313,119.468868616061,
119.581966991173,119.695042813645,119.808222590789,119.921453883988,120.034898877917,
120.121687103815,120.249019489535,120.376140840035,120.503262190536),
 .UNSPECIFIED.);
#186=B_SPLINE_CURVE_WITH_KNOTS('',3,(#18707,#18708,#18709,#18710,#18711,
#18712,#18713,#18714,#18715,#18716),.UNSPECIFIED.,.F.,.F.,(4,1,1,1,1,1,
1,4),(-129.75572966404,-129.056358045421,-128.063616829687,-127.070875613953,
-126.078134398219,-125.085393182485,-124.092651966751,-123.472544356861),
 .UNSPECIFIED.);
#187=B_SPLINE_CURVE_WITH_KNOTS('',3,(#18717,#18718,#18719,#18720,#18721,
#18722,#18723,#18724,#18725,#18726),.UNSPECIFIED.,.F.,.F.,(4,1,1,1,1,1,
1,4),(120.503262642873,121.114428319549,122.107169535283,123.099910751017,
124.092651966751,125.085393182485,126.078134398219,126.786447950053),
 .UNSPECIFIED.);
#188=B_SPLINE_CURVE_WITH_KNOTS('',3,(#18729,#18730,#18731,#18732,#18733,
#18734,#18735,#18736,#18737),.UNSPECIFIED.,.F.,.F.,(4,1,1,1,1,1,4),(126.786447950053,
127.070875613953,128.063616829687,129.056358045421,130.049099261155,131.041840476889,
131.946449082288),.UNSPECIFIED.);
#189=B_SPLINE_CURVE_WITH_KNOTS('',3,(#18740,#18741,#18742,#18743,#18744,
#18745,#18746,#18747),.UNSPECIFIED.,.F.,.F.,(4,1,1,1,1,4),(-134.020064124091,
-133.027322908357,-132.034581692623,-131.041840476889,-130.049099261155,
-129.75572966404),.UNSPECIFIED.);
#190=B_SPLINE_CURVE_WITH_KNOTS('',3,(#18750,#18751,#18752,#18753,#18754,
#18755,#18756,#18757,#18758,#18759,#18760,#18761,#18762,#18763,#18764,#18765,
#18766,#18767,#18768,#18769,#18770,#18771,#18772,#18773,#18774,#18775,#18776,
#18777,#18778,#18779,#18780,#18781,#18782,#18783,#18784,#18785,#18786,#18787,
#18788,#18789,#18790,#18791,#18792,#18793,#18794,#18795,#18796,#18797,#18798,
#18799,#18800,#18801,#18802,#18803,#18804,#18805,#18806,#18807,#18808,#18809,
#18810,#18811,#18812,#18813,#18814,#18815,#18816,#18817,#18818,#18819,#18820,
#18821,#18822,#18823,#18824,#18825,#18826,#18827,#18828,#18829,#18830,#18831,
#18832,#18833,#18834,#18835,#18836,#18837,#18838,#18839,#18840,#18841,#18842,
#18843,#18844,#18845,#18846,#18847,#18848,#18849,#18850,#18851,#18852,#18853,
#18854,#18855,#18856,#18857,#18858,#18859,#18860,#18861,#18862,#18863,#18864,
#18865,#18866,#18867,#18868,#18869,#18870,#18871,#18872,#18873,#18874,#18875,
#18876,#18877,#18878,#18879,#18880,#18881,#18882,#18883,#18884,#18885,#18886,
#18887,#18888,#18889,#18890,#18891,#18892,#18893,#18894,#18895,#18896,#18897,
#18898,#18899,#18900,#18901,#18902,#18903,#18904,#18905,#18906,#18907,#18908,
#18909,#18910,#18911,#18912,#18913,#18914,#18915,#18916,#18917,#18918,#18919,
#18920,#18921,#18922,#18923,#18924,#18925,#18926,#18927,#18928,#18929,#18930,
#18931,#18932,#18933,#18934,#18935,#18936,#18937,#18938,#18939,#18940,#18941,
#18942,#18943,#18944,#18945,#18946,#18947,#18948,#18949,#18950,#18951,#18952,
#18953,#18954,#18955,#18956,#18957,#18958,#18959,#18960,#18961,#18962,#18963,
#18964,#18965,#18966,#18967,#18968,#18969),.UNSPECIFIED.,.F.,.F.,(4,2,2,
2,2,2,2,2,2,2,2,2,2,2,2,2,2,2,2,2,2,2,2,2,2,2,2,2,2,2,2,2,2,2,2,2,2,2,2,
2,2,2,2,2,2,2,2,2,2,2,2,2,2,2,2,2,2,2,2,2,2,2,2,2,2,2,2,2,2,2,2,2,2,2,2,
2,2,2,2,2,2,2,2,2,2,2,2,2,2,2,2,2,2,2,2,2,2,2,2,2,2,2,2,2,2,2,2,2,2,4),
(0.00177133348906076,0.0332939428224796,0.0446468589001284,0.0476492977162608,
0.0494853420994853,0.0511583358113068,0.0532949673361036,0.0578790368847078,
0.0813213073966685,0.0895856412014572,0.0990580205537023,0.102622914444339,
0.105242464183177,0.106418036567059,0.106425319281184,0.106432688952577,
0.106440148378348,0.106447700458387,0.106455348206415,0.106463094739559,
0.106470943300493,0.106478897255693,0.10648696010216,0.106495135472981,
0.106503427147395,0.106511839057682,0.106520375300179,0.10652904013602,
0.106537838004738,0.106546773541824,0.106555851576764,0.106565077148689,
0.106574455519887,0.106583992185623,0.106593692889877,0.106603563639179,
0.106613610715625,0.106623840698047,0.10663426047506,0.106644877266566,
0.106655698639468,0.106666732539314,0.10667798730311,0.106686051022993,
0.10669489762429,0.106704614123707,0.106715299378267,0.106727066141351,
0.106740043560568,0.106754380232775,0.106770247990901,0.10678784660648,
0.106807409704104,0.106829212253955,0.106853419150707,0.106897105788926,
0.107816294099124,0.109081163064197,0.111910851100339,0.135116451326652,
0.158532048225741,0.162482297374512,0.164503661603351,0.166142589934801,
0.168029653860336,0.17125042402507,0.184976326644695,0.208927063192172,
0.220978798931431,0.222978304221318,0.224059923343987,0.224972713857167,
0.226139316161746,0.228029587104807,0.240500208304931,0.261844348980189,
0.277340634958833,0.280555592843824,0.282408559802314,0.284028276391786,
0.286039067649986,0.289152481512839,0.308939925241119,0.335665513235547,
0.339541664253455,0.340941482759423,0.341887494004219,0.342746628886886,
0.343931091601083,0.346949519411781,0.366240512633496,0.384771895284079,
0.395407454452054,0.398321699095411,0.400120964557772,0.401771292687552,
0.403893311497895,0.408498954083469,0.433359934700143,0.44083891144931,
0.454104461318418,0.456976778935707,0.458230446940733,0.459157967202875,
0.460195667052555,0.461989925851204,0.468838101212243,0.475410570919698,
0.50070097981199,0.500726922102148),.UNSPECIFIED.);
#191=B_SPLINE_CURVE_WITH_KNOTS('',3,(#18973,#18974,#18975,#18976,#18977,
#18978,#18979,#18980,#18981,#18982,#18983,#18984,#18985,#18986,#18987,#18988,
#18989,#18990,#18991,#18992,#18993,#18994,#18995,#18996,#18997),
 .UNSPECIFIED.,.F.,.F.,(4,3,3,3,3,3,3,3,4),(141.371669412113,141.493776626037,
141.615676098753,141.737414642623,141.859038816202,141.980634322619,142.102203953115,
142.223875192913,142.322100278399),.UNSPECIFIED.);
#192=B_SPLINE_CURVE_WITH_KNOTS('',3,(#18998,#18999,#19000,#19001,#19002,
#19003,#19004,#19005,#19006,#19007,#19008,#19009,#19010,#19011,#19012,#19013,
#19014,#19015,#19016,#19017,#19018,#19019,#19020,#19021,#19022,#19023,#19024,
#19025,#19026,#19027,#19028,#19029,#19030,#19031,#19032,#19033,#19034,#19035,
#19036,#19037,#19038,#19039,#19040,#19041,#19042,#19043,#19044,#19045,#19046,
#19047,#19048,#19049,#19050,#19051,#19052,#19053,#19054,#19055,#19056,#19057,
#19058),.UNSPECIFIED.,.F.,.F.,(4,3,3,3,3,3,3,3,3,3,3,3,3,3,3,3,3,3,3,3,
4),(139.325819053623,139.343876631197,139.467969283164,139.587740756953,
139.707395900858,139.826987018576,139.946566302737,140.066267437187,140.186042193601,
140.306031049809,140.336617846931,140.460710498898,140.578991514728,140.697156542209,
140.815260477709,140.933358102547,141.051596289664,141.16991700588,141.288479603891,
141.329359062665,141.371669411541),.UNSPECIFIED.);
#193=B_SPLINE_CURVE_WITH_KNOTS('',3,(#19611,#19612,#19613,#19614,#19615,
#19616,#19617,#19618,#19619,#19620,#19621,#19622,#19623,#19624,#19625,#19626,
#19627,#19628,#19629,#19630,#19631,#19632,#19633,#19634,#19635,#19636,#19637,
#19638,#19639,#19640,#19641,#19642,#19643,#19644,#19645,#19646,#19647,#19648,
#19649,#19650,#19651,#19652,#19653,#19654,#19655,#19656,#19657,#19658,#19659,
#19660,#19661,#19662,#19663,#19664,#19665,#19666,#19667,#19668,#19669,#19670,
#19671,#19672,#19673,#19674,#19675,#19676,#19677,#19678,#19679,#19680,#19681,
#19682,#19683,#19684,#19685,#19686,#19687,#19688,#19689),.UNSPECIFIED.,
 .F.,.F.,(4,3,3,3,3,3,3,3,3,3,3,3,3,3,3,3,3,3,3,3,3,3,3,3,3,3,4),(0.,0.0128630913698734,
0.030173607454054,0.0476766315161026,0.0523696650465307,0.0555715997243662,
0.0588510993424858,0.0758834917292733,0.0926337870888054,0.10745987033467,
0.111898493425318,0.128068424972759,0.144019690384188,0.151482256100753,
0.158624488771535,0.162483307325829,0.16875922376809,0.184724176101981,
0.200705370878488,0.205805249761507,0.211151080047986,0.214604616888512,
0.230111410594562,0.242198197870331,0.246866765408764,0.261749278560737,
0.27663179171271),.UNSPECIFIED.);
#194=B_SPLINE_CURVE_WITH_KNOTS('',3,(#19691,#19692,#19693,#19694,#19695,
#19696,#19697,#19698,#19699,#19700,#19701,#19702,#19703,#19704,#19705,#19706,
#19707,#19708,#19709,#19710,#19711,#19712,#19713,#19714,#19715,#19716,#19717,
#19718,#19719,#19720,#19721,#19722,#19723,#19724,#19725,#19726,#19727,#19728,
#19729,#19730,#19731,#19732,#19733,#19734,#19735,#19736,#19737,#19738,#19739,
#19740,#19741,#19742,#19743,#19744,#19745,#19746,#19747,#19748,#19749,#19750,
#19751,#19752,#19753,#19754,#19755,#19756,#19757,#19758,#19759,#19760,#19761,
#19762,#19763,#19764,#19765,#19766,#19767,#19768,#19769),.UNSPECIFIED.,
 .F.,.F.,(4,3,3,3,3,3,3,3,3,3,3,3,3,3,3,3,3,3,3,3,3,3,3,3,3,3,4),(0.,0.0104682740580808,
0.0251836130964161,0.0388969524160199,0.0444857430892301,0.0491054717138812,
0.0584413971085396,0.0740336439398356,0.0898096170712714,0.0952778368687677,
0.0982274123820461,0.114504809333193,0.130605059063041,0.136378173267175,
0.141969801169779,0.145794135544524,0.148768119797174,0.16481698689922,
0.181420617025118,0.198000402839796,0.201209381411116,0.218350668985889,
0.232526805791533,0.236420955594387,0.242939799192087,0.260349393962725,
0.275362278356888),.UNSPECIFIED.);
#195=B_SPLINE_CURVE_WITH_KNOTS('',3,(#19770,#19771,#19772,#19773),
 .UNSPECIFIED.,.F.,.F.,(4,4),(-0.01194426971835,0.),.UNSPECIFIED.);
#196=B_SPLINE_CURVE_WITH_KNOTS('',3,(#20327,#20328,#20329,#20330,#20331,
#20332,#20333,#20334,#20335,#20336,#20337,#20338,#20339,#20340,#20341,#20342,
#20343,#20344,#20345,#20346,#20347,#20348,#20349,#20350,#20351,#20352,#20353,
#20354,#20355,#20356,#20357,#20358,#20359,#20360,#20361,#20362,#20363,#20364,
#20365,#20366,#20367,#20368,#20369,#20370,#20371,#20372,#20373,#20374,#20375,
#20376,#20377,#20378,#20379,#20380,#20381,#20382,#20383,#20384,#20385,#20386,
#20387,#20388,#20389,#20390,#20391,#20392,#20393,#20394,#20395,#20396,#20397,
#20398,#20399,#20400,#20401,#20402,#20403,#20404,#20405),.UNSPECIFIED.,
 .F.,.F.,(4,3,3,3,3,3,3,3,3,3,3,3,3,3,3,3,3,3,3,3,3,3,3,3,3,3,4),(0.,0.0104682740580829,
0.0250094730845676,0.0400379756695705,0.0464362531658784,0.0494477396468055,
0.0648452005482684,0.0806255921987773,0.0952778402954169,0.0982274132155018,
0.114504810108782,0.130605060062163,0.136378173267178,0.141969800959009,
0.145794134531399,0.148768118134835,0.164776942997393,0.181333154791539,
0.193217549992342,0.198000400400437,0.201209379964382,0.218350667946125,
0.232526805152432,0.236420954197035,0.24018725862019,0.257774768488541,
0.275362278356893),.UNSPECIFIED.);
#197=B_SPLINE_CURVE_WITH_KNOTS('',3,(#20406,#20407,#20408,#20409),
 .UNSPECIFIED.,.F.,.F.,(4,4),(0.,0.0121610650312646),.UNSPECIFIED.);
#198=B_SPLINE_CURVE_WITH_KNOTS('',3,(#20410,#20411,#20412,#20413,#20414,
#20415,#20416,#20417,#20418,#20419,#20420,#20421,#20422,#20423,#20424,#20425,
#20426,#20427,#20428,#20429,#20430,#20431,#20432,#20433,#20434,#20435,#20436,
#20437,#20438,#20439,#20440,#20441,#20442,#20443,#20444,#20445,#20446,#20447,
#20448,#20449,#20450,#20451,#20452,#20453,#20454,#20455,#20456,#20457,#20458,
#20459,#20460,#20461,#20462,#20463,#20464,#20465,#20466,#20467,#20468,#20469,
#20470,#20471,#20472,#20473,#20474,#20475,#20476,#20477,#20478,#20479,#20480,
#20481,#20482),.UNSPECIFIED.,.F.,.F.,(4,3,3,3,3,3,3,3,3,3,3,3,3,3,3,3,3,
3,3,3,3,3,3,3,4),(0.,0.0128630913698816,0.0301736075898532,0.0476766317653969,
0.0523696653091531,0.0557875908672854,0.0588510996533798,0.0758834920598313,
0.0926337883448894,0.107459871004135,0.111898493425658,0.128218441979264,
0.144019692909864,0.151482256100771,0.160181367556473,0.163702575469109,
0.179617427500875,0.195596970381227,0.211151080173894,0.214604616819749,
0.230040863840438,0.242198197759019,0.246866765353746,0.261749278533234,
0.276631791712723),.UNSPECIFIED.);
#199=B_SPLINE_CURVE_WITH_KNOTS('',3,(#20491,#20492,#20493,#20494,#20495,
#20496),.UNSPECIFIED.,.F.,.F.,(4,1,1,4),(30.4992259586856,30.7378583994183,
31.7316740381467,32.725489676875),.UNSPECIFIED.);
#200=B_SPLINE_CURVE_WITH_KNOTS('',3,(#20499,#20500,#20501,#20502,#20503,
#20504,#20505,#20506,#20507,#20508,#20509,#20510,#20511,#20512,#20513,#20514,
#20515,#20516,#20517,#20518,#20519,#20520,#20521,#20522,#20523,#20524,#20525,
#20526,#20527,#20528,#20529,#20530,#20531,#20532,#20533,#20534,#20535,#20536,
#20537,#20538,#20539,#20540,#20541,#20542,#20543,#20544,#20545,#20546,#20547,
#20548,#20549,#20550,#20551,#20552,#20553,#20554,#20555,#20556,#20557,#20558,
#20559,#20560,#20561,#20562,#20563,#20564,#20565,#20566,#20567,#20568,#20569,
#20570,#20571,#20572,#20573,#20574),.UNSPECIFIED.,.F.,.F.,(4,3,3,3,3,3,
3,3,3,3,3,3,3,3,3,3,3,3,3,3,3,3,3,3,3,4),(30.5007265447835,30.6123224488076,
30.7238426226409,30.83533023183,30.949814170211,31.0614387973166,31.1773523913354,
31.2932659853541,31.4054181808839,31.5173715972371,31.6292139644157,31.7409880765415,
31.8527366302182,31.964582347948,32.0764735793981,32.1885741551002,32.2870816240825,
32.3984002763317,32.5095261241697,32.6205455724167,32.7315027540499,32.8424417080743,
32.953484666185,33.0645821004634,33.1758840410784,33.2477856371927),
 .UNSPECIFIED.);
#201=B_SPLINE_CURVE_WITH_KNOTS('',3,(#20580,#20581,#20582,#20583,#20584,
#20585,#20586,#20587,#20588,#20589,#20590,#20591,#20592,#20593,#20594,#20595,
#20596,#20597,#20598,#20599,#20600,#20601,#20602,#20603,#20604,#20605,#20606,
#20607,#20608,#20609,#20610,#20611,#20612,#20613,#20614,#20615,#20616,#20617,
#20618,#20619,#20620,#20621,#20622,#20623,#20624,#20625,#20626,#20627,#20628,
#20629,#20630,#20631,#20632,#20633,#20634,#20635,#20636,#20637,#20638,#20639,
#20640,#20641,#20642,#20643,#20644,#20645,#20646,#20647,#20648,#20649,#20650,
#20651,#20652,#20653,#20654,#20655,#20656,#20657,#20658,#20659,#20660,#20661,
#20662,#20663,#20664,#20665,#20666,#20667,#20668,#20669,#20670,#20671,#20672,
#20673,#20674,#20675,#20676,#20677,#20678,#20679,#20680,#20681,#20682,#20683,
#20684,#20685,#20686,#20687,#20688,#20689,#20690,#20691),.UNSPECIFIED.,
 .F.,.F.,(4,3,3,3,3,3,3,3,3,3,3,3,3,3,3,3,3,3,3,3,3,3,3,3,3,3,3,3,3,3,3,
3,3,3,3,3,3,4),(24.2171454613693,24.328721144631,24.4403944911041,24.5521112223609,
24.6640460242382,24.7749645670481,24.8869276730768,24.9986930187964,25.1103480734547,
25.2219359515843,25.3334996710813,25.445164216606,25.5568760037622,25.6688023337555,
25.7687802057765,25.8807705272124,25.9925629669429,26.1042450229036,26.2158597642098,
26.3274501632448,26.4391408893548,26.5508786252935,26.6628301813545,26.7625958445049,
26.8745738108416,26.9863543659224,27.0980248308916,27.2096282913631,27.3212077365666,
27.4328881016498,27.5446157852499,27.6565579314224,27.7564114832332,27.8730056569828,
27.989278435079,28.1053581204607,28.2212227044162,28.2743338823081),
 .UNSPECIFIED.);
#202=B_SPLINE_CURVE_WITH_KNOTS('',3,(#20692,#20693,#20694,#20695,#20696,
#20697),.UNSPECIFIED.,.F.,.F.,(4,1,1,4),(28.2743353560929,28.7502271219616,
29.74404276069,30.4992259586856),.UNSPECIFIED.);
#203=B_SPLINE_CURVE_WITH_KNOTS('',3,(#20699,#20700,#20701,#20702,#20703,
#20704,#20705,#20706,#20707,#20708,#20709,#20710,#20711,#20712,#20713,#20714,
#20715,#20716,#20717,#20718,#20719,#20720,#20721,#20722,#20723,#20724,#20725,
#20726,#20727,#20728,#20729,#20730,#20731,#20732,#20733,#20734,#20735,#20736,
#20737,#20738,#20739,#20740,#20741,#20742,#20743,#20744,#20745,#20746,#20747,
#20748,#20749,#20750,#20751,#20752,#20753,#20754,#20755,#20756,#20757,#20758,
#20759,#20760,#20761,#20762),.UNSPECIFIED.,.F.,.F.,(4,3,3,3,3,3,3,3,3,3,
3,3,3,3,3,3,3,3,3,3,3,4),(28.2743338823081,28.311819069169,28.4238093895684,
28.5356018282781,28.6472838832279,28.7588986235352,28.8704890215845,28.9821797467369,
29.0939174817321,29.2058690368848,29.3056347078974,29.417612671015,29.5293932228493,
29.6410636845579,29.7526671417604,29.8642465836919,29.9759269455253,30.0876546258826,
30.1995967688657,30.2994503466257,30.4113016433696,30.5007265447835),
 .UNSPECIFIED.);
#204=B_SPLINE_CURVE_WITH_KNOTS('',3,(#20763,#20764,#20765,#20766,#20767,
#20768,#20769,#20770,#20771,#20772,#20773,#20774,#20775,#20776,#20777,#20778,
#20779,#20780,#20781,#20782,#20783,#20784,#20785,#20786,#20787,#20788,#20789,
#20790,#20791,#20792,#20793,#20794,#20795,#20796,#20797,#20798,#20799,#20800,
#20801,#20802,#20803,#20804,#20805,#20806,#20807,#20808,#20809,#20810,#20811,
#20812,#20813,#20814,#20815,#20816,#20817,#20818,#20819,#20820,#20821,#20822,
#20823,#20824,#20825,#20826,#20827,#20828,#20829,#20830,#20831,#20832,#20833,
#20834,#20835,#20836,#20837,#20838,#20839,#20840,#20841,#20842,#20843,#20844,
#20845,#20846,#20847,#20848,#20849,#20850,#20851,#20852,#20853,#20854,#20855,
#20856,#20857,#20858,#20859,#20860,#20861,#20862,#20863,#20864,#20865,#20866,
#20867,#20868,#20869,#20870,#20871,#20872,#20873,#20874,#20875,#20876,#20877),
 .UNSPECIFIED.,.F.,.F.,(4,3,3,3,3,3,3,3,3,3,3,3,3,3,3,3,3,3,3,3,3,3,3,3,
3,3,3,3,3,3,3,3,3,3,3,3,3,3,4),(24.2164750170476,24.3284524197536,24.3365565142555,
24.4485275333045,24.5603007790059,24.6719637201736,24.7835594578674,24.8951309964992,
25.0068032353764,25.1185226592433,25.2304564321671,25.3303721529839,25.4423470704048,
25.5541242241199,25.6657910764357,25.7773907217266,25.8889661577255,26.000642246938,
26.1123655015154,26.2243030228786,26.3241877917123,26.4361623320395,26.5479391606963,
26.659605719745,26.7712051037159,26.8827803105362,26.9944562220728,27.1061793269458,
27.2181167469796,27.3180034304406,27.4292987988986,27.5403976766296,27.6513879633006,
27.7623138516846,27.8732194375054,27.9842247077935,28.0952828235162,28.2065395519308,
28.2743338817731),.UNSPECIFIED.);
#205=B_SPLINE_CURVE_WITH_KNOTS('',3,(#20883,#20884,#20885,#20886,#20887,
#20888,#20889,#20890,#20891,#20892,#20893,#20894,#20895,#20896,#20897,#20898,
#20899,#20900,#20901,#20902,#20903,#20904,#20905,#20906,#20907,#20908,#20909,
#20910,#20911,#20912,#20913,#20914,#20915,#20916,#20917,#20918,#20919,#20920,
#20921,#20922,#20923,#20924,#20925,#20926,#20927,#20928,#20929,#20930,#20931,
#20932,#20933,#20934,#20935,#20936,#20937,#20938,#20939,#20940,#20941,#20942,
#20943),.UNSPECIFIED.,.F.,.F.,(4,3,3,3,3,3,3,3,3,3,3,3,3,3,3,3,3,3,3,3,
4),(15.707963267949,15.8187595067976,15.9295233360101,16.0436503531147,
16.1545574801957,16.2702944423121,16.3860314044286,16.4979936760791,16.6097538040557,
16.7214009788804,16.8329783413831,16.9445289325292,17.0561763685529,17.1678688344864,
17.2797723742714,17.379847043157,17.4919754947928,17.6039188766938,17.7157519036505,
17.8275438837686,17.9335641972525),.UNSPECIFIED.);
#206=B_SPLINE_CURVE_WITH_KNOTS('',3,(#20945,#20946,#20947,#20948,#20949,
#20950,#20951,#20952,#20953,#20954,#20955,#20956,#20957,#20958,#20959,#20960,
#20961,#20962,#20963,#20964,#20965,#20966,#20967,#20968,#20969,#20970,#20971,
#20972,#20973,#20974,#20975,#20976,#20977,#20978,#20979,#20980,#20981),
 .UNSPECIFIED.,.F.,.F.,(4,3,3,3,3,3,3,3,3,3,3,3,4),(14.3984001269719,14.5126517902779,
14.6268360531343,14.7409856972805,14.8551365966922,14.9693246155366,15.0836816294035,
15.1981262282676,15.3128130782455,15.3922157657002,15.5228352705414,15.6520281526537,
15.7079632674506),.UNSPECIFIED.);
#207=B_SPLINE_CURVE_WITH_KNOTS('',3,(#20985,#20986,#20987,#20988,#20989,
#20990,#20991,#20992,#20993,#20994,#20995,#20996,#20997,#20998,#20999,#21000,
#21001,#21002,#21003,#21004,#21005,#21006,#21007,#21008,#21009,#21010,#21011,
#21012,#21013,#21014,#21015,#21016,#21017,#21018,#21019,#21020,#21021,#21022,
#21023,#21024,#21025,#21026,#21027,#21028,#21029,#21030,#21031,#21032,#21033,
#21034,#21035,#21036),.UNSPECIFIED.,.F.,.F.,(4,3,3,3,3,3,3,3,3,3,3,3,3,
3,3,3,3,4),(13.8759341327667,13.9872665954873,14.0984010834278,14.2094259872279,
14.3203854485755,14.4313235110963,14.5423608000363,14.6534498395139,14.7647392915059,
14.8368081797645,14.9473443597248,15.0577306248179,15.1680122762973,15.2782344500762,
15.3885087645923,15.4988033613755,15.6092745562469,15.7079632675072),
 .UNSPECIFIED.);
#208=B_SPLINE_CURVE_WITH_KNOTS('',3,(#21037,#21038,#21039,#21040,#21041,
#21042,#21043,#21044,#21045,#21046,#21047,#21048,#21049,#21050,#21051,#21052,
#21053,#21054,#21055,#21056,#21057,#21058,#21059,#21060,#21061,#21062,#21063,
#21064,#21065,#21066,#21067,#21068,#21069,#21070,#21071,#21072,#21073,#21074,
#21075,#21076,#21077,#21078,#21079,#21080,#21081,#21082,#21083,#21084,#21085,
#21086,#21087,#21088,#21089,#21090,#21091,#21092,#21093,#21094,#21095,#21096,
#21097),.UNSPECIFIED.,.F.,.F.,(4,3,3,3,3,3,3,3,3,3,3,3,3,3,3,3,3,3,3,3,
4),(15.707963267949,15.8306238184928,15.9425134931221,16.0542037235325,
16.1657826907118,16.2772936442665,16.3887797359164,16.5003661757896,16.6119994681162,
16.7238476652717,16.8244394572212,16.9364188879014,17.0482003665379,17.1598714256532,
17.2714751517678,17.3830545346207,17.4947343260332,17.6064611544644,17.7184019844554,
17.8182550959496,17.9342486843494),.UNSPECIFIED.);
#209=B_SPLINE_CURVE_WITH_KNOTS('',3,(#21103,#21104,#21105,#21106,#21107,
#21108,#21109,#21110,#21111,#21112,#21113,#21114,#21115,#21116,#21117,#21118,
#21119,#21120,#21121,#21122,#21123,#21124,#21125,#21126,#21127,#21128,#21129,
#21130,#21131,#21132,#21133,#21134,#21135,#21136,#21137,#21138,#21139,#21140,
#21141,#21142,#21143,#21144,#21145,#21146,#21147,#21148,#21149,#21150,#21151,
#21152,#21153,#21154),.UNSPECIFIED.,.F.,.F.,(4,3,3,3,3,3,3,3,3,3,3,3,3,
3,3,3,3,4),(18.2325677587798,18.3498303574559,18.4670738156485,18.5844332834504,
18.7018559905836,18.8195012614516,18.8824971358389,18.9993814731626,19.1160527382571,
19.2326074989738,19.3490972166108,19.4655732408159,19.5821766235442,19.6988502996544,
19.8157586904299,19.8763127745673,20.0296181157692,20.1591059545013),
 .UNSPECIFIED.);
#210=B_SPLINE_CURVE_WITH_KNOTS('',3,(#21156,#21157,#21158,#21159,#21160,
#21161,#21162,#21163,#21164,#21165,#21166,#21167,#21168,#21169),
 .UNSPECIFIED.,.F.,.F.,(4,2,2,2,2,2,4),(-0.0903144895684469,-0.0692444659278893,
-0.0576954263704227,-0.0451675812950829,-0.0304576276691574,-0.00758134388617478,
0.),.UNSPECIFIED.);
#211=B_SPLINE_CURVE_WITH_KNOTS('',3,(#21172,#21173,#21174,#21175,#21176,
#21177,#21178,#21179,#21180,#21181,#21182,#21183,#21184,#21185,#21186,#21187,
#21188,#21189,#21190,#21191,#21192,#21193,#21194,#21195,#21196,#21197,#21198,
#21199,#21200,#21201,#21202,#21203,#21204,#21205,#21206,#21207,#21208,#21209,
#21210,#21211,#21212,#21213,#21214,#21215,#21216,#21217,#21218,#21219,#21220,
#21221,#21222,#21223,#21224,#21225,#21226,#21227,#21228,#21229,#21230,#21231,
#21232,#21233,#21234,#21235,#21236,#21237,#21238,#21239,#21240,#21241,#21242,
#21243,#21244,#21245,#21246,#21247,#21248,#21249,#21250,#21251),
 .UNSPECIFIED.,.F.,.F.,(4,2,2,2,2,2,2,2,2,2,2,2,2,2,2,2,2,2,2,2,2,2,2,2,
2,2,2,2,2,2,2,2,2,2,2,2,2,2,2,4),(-2.38727423776056,-2.38406272448339,-2.3557931220579,
-2.33755291028634,-2.32704088174431,-2.31484332484773,-2.28541728558956,
-2.27583295603182,-2.26827320890842,-2.26174684622007,-2.23039420085245,
-2.21738636427069,-2.20583957855992,-2.19513154387513,-2.17099129080296,
-2.15495721776536,-2.14472291534183,-2.13868394797197,-2.12944141110975,
-2.10363838951637,-2.09095738686218,-2.07961062057348,-2.06898426027192,
-2.04490653827237,-2.02884653579313,-2.01862053881223,-2.0126050191353,
-2.0034594802115,-1.97766500598942,-1.96487183705672,-1.95344529599827,
-1.94275622036405,-1.92404139176448,-1.9045009960413,-1.89321241694263,
-1.88718106050413,-1.87861020022266,-1.85185187742313,-1.83903298230054,
-1.83671080313269),.UNSPECIFIED.);
#212=B_SPLINE_CURVE_WITH_KNOTS('',3,(#21257,#21258,#21259,#21260,#21261,
#21262,#21263,#21264,#21265,#21266,#21267,#21268,#21269,#21270,#21271,#21272,
#21273,#21274,#21275,#21276,#21277,#21278,#21279,#21280,#21281,#21282,#21283,
#21284,#21285,#21286,#21287,#21288,#21289,#21290,#21291,#21292,#21293,#21294,
#21295,#21296,#21297,#21298,#21299,#21300,#21301,#21302,#21303,#21304,#21305,
#21306,#21307,#21308,#21309,#21310,#21311),.UNSPECIFIED.,.F.,.F.,(4,3,3,
3,3,3,3,3,3,3,3,3,3,3,3,3,3,3,4),(11.9490926668048,12.0704064963878,12.1878478712382,
12.3051825606139,12.4224605559092,12.5397317517184,12.6571250989989,12.7745928009127,
12.8922685579825,12.9196033034688,13.039144609872,13.1559019011595,13.2725441076707,
13.3891225237288,13.5108253314701,13.6275077647654,13.7442638674747,13.8612193036346,
13.8759337546943),.UNSPECIFIED.);
#213=B_SPLINE_CURVE_WITH_KNOTS('',3,(#21312,#21313,#21314,#21315,#21316,
#21317,#21318,#21319,#21320,#21321,#21322,#21323,#21324,#21325,#21326,#21327,
#21328,#21329,#21330,#21331,#21332,#21333,#21334,#21335,#21336,#21337,#21338,
#21339,#21340,#21341,#21342,#21343,#21344,#21345,#21346,#21347,#21348,#21349,
#21350,#21351,#21352,#21353,#21354,#21355,#21356,#21357,#21358,#21359,#21360,
#21361,#21362,#21363,#21364,#21365,#21366,#21367,#21368,#21369,#21370,#21371,
#21372,#21373,#21374,#21375,#21376,#21377,#21378,#21379,#21380,#21381,#21382,
#21383,#21384,#21385,#21386,#21387,#21388,#21389,#21390,#21391,#21392,#21393,
#21394,#21395,#21396,#21397,#21398,#21399,#21400,#21401,#21402,#21403,#21404,
#21405,#21406,#21407,#21408,#21409,#21410,#21411,#21412,#21413,#21414,#21415,
#21416,#21417,#21418,#21419,#21420,#21421,#21422,#21423,#21424,#21425,#21426,
#21427,#21428,#21429,#21430,#21431,#21432),.UNSPECIFIED.,.F.,.F.,(4,3,3,
3,3,3,3,3,3,3,3,3,3,3,3,3,3,3,3,3,3,3,3,3,3,3,3,3,3,3,3,3,3,3,3,3,3,3,3,
3,4),(13.8759337553363,13.9134189421971,14.0311232235957,14.1486125013357,
14.2659834897556,14.3832861820323,14.5005704595919,14.6179686096979,14.7354306420707,
14.853108166008,14.9072345809255,15.0249258745496,15.1424026742923,15.2597615104701,
15.3770523954505,15.4943252302791,15.6117125694428,15.7291641366733,15.8468318409145,
15.9010502196539,16.0186444543146,16.1360236186112,16.2532845471506,16.3704774396887,
16.4876523842386,16.6049427606468,16.7222977569782,16.8398706110872,16.8948658583822,
17.0127402740903,17.1303987141068,17.2479381064766,17.3654081250404,17.4828583308553,
17.6004190050346,17.7180418335406,17.8358756688541,17.8886814971106,18.0063081000976,
18.1237490007858,18.2325677587798),.UNSPECIFIED.);
#214=B_SPLINE_CURVE_WITH_KNOTS('',3,(#21433,#21434,#21435,#21436,#21437,
#21438,#21439,#21440,#21441,#21442,#21443,#21444,#21445,#21446,#21447,#21448,
#21449,#21450,#21451,#21452,#21453,#21454,#21455,#21456,#21457,#21458,#21459,
#21460,#21461,#21462,#21463,#21464,#21465,#21466,#21467,#21468,#21469,#21470,
#21471,#21472,#21473,#21474,#21475,#21476,#21477,#21478,#21479,#21480,#21481,
#21482,#21483,#21484,#21485,#21486,#21487,#21488,#21489,#21490,#21491,#21492,
#21493,#21494,#21495,#21496,#21497,#21498,#21499,#21500,#21501,#21502,#21503,
#21504,#21505,#21506,#21507,#21508,#21509,#21510,#21511,#21512,#21513,#21514,
#21515,#21516,#21517,#21518,#21519,#21520,#21521,#21522,#21523,#21524,#21525,
#21526,#21527,#21528,#21529,#21530,#21531,#21532,#21533,#21534,#21535,#21536,
#21537,#21538,#21539,#21540,#21541,#21542,#21543,#21544,#21545,#21546),
 .UNSPECIFIED.,.F.,.F.,(4,2,2,2,2,2,2,2,2,2,2,2,2,2,2,2,2,2,2,2,2,2,2,2,
2,2,2,2,2,2,2,2,2,2,2,2,2,2,2,2,2,2,2,2,2,2,2,2,2,2,2,2,2,2,2,2,4),(-1.83671080313269,
-1.82759849494319,-1.81692795186113,-1.79563929798103,-1.77779257395854,
-1.76699053250404,-1.76093911515616,-1.75209456774871,-1.72642332328398,
-1.71339291330754,-1.70186211436507,-1.69125802302839,-1.67198737355153,
-1.6525162997874,-1.64426846678166,-1.63741779966473,-1.63057719938065,
-1.61111305684996,-1.58624264998279,-1.575038216497,-1.56423320731616,-1.53294347082481,
-1.51676689755966,-1.51040659458799,-1.5028295689763,-1.47285225044348,
-1.46041985100477,-1.44917306242916,-1.43840209278037,-1.42139887540163,
-1.40094682104524,-1.389416018895,-1.38332969003068,-1.37485962772093,-1.33992511892625,
-1.32670780248308,-1.31643728663368,-1.30152516541418,-1.27648087306842,
-1.26389145275289,-1.2577415241614,-1.249492316077,-1.22423903595011,-1.20491784183702,
-1.19442406440538,-1.1826084706153,-1.16897540982433,-1.14368559895163,
-1.13545766355708,-1.12939283725948,-1.11738157832569,-1.09498355884621,
-1.07799856687676,-1.06762641984851,-1.0553136942615,-1.04059910634095,
-1.04037338208336),.UNSPECIFIED.);
#215=B_SPLINE_CURVE_WITH_KNOTS('',3,(#21552,#21553,#21554,#21555,#21556,
#21557,#21558,#21559,#21560,#21561,#21562,#21563,#21564,#21565,#21566,#21567,
#21568,#21569,#21570,#21571,#21572,#21573,#21574,#21575,#21576,#21577,#21578,
#21579,#21580,#21581,#21582,#21583,#21584,#21585),.UNSPECIFIED.,.F.,.F.,
(4,2,2,2,2,2,2,2,2,2,2,2,2,2,2,2,4),(-0.244154988360166,-0.239251614829434,
-0.206955793200255,-0.193245893310612,-0.183335383234761,-0.17038967951317,
-0.135910395886769,-0.127712618705488,-0.121625554061406,-0.110199764636449,
-0.0909155361461006,-0.0686614677051733,-0.0570683697132675,-0.0439652197544473,
-0.0280399100598725,-0.0077322087934803,-3.42095323259393E-5),
 .UNSPECIFIED.);
#216=B_SPLINE_CURVE_WITH_KNOTS('',3,(#21588,#21589,#21590,#21591,#21592,
#21593,#21594,#21595,#21596,#21597,#21598,#21599,#21600,#21601,#21602,#21603,
#21604,#21605,#21606,#21607,#21608,#21609,#21610,#21611,#21612,#21613,#21614,
#21615,#21616,#21617,#21618,#21619,#21620,#21621,#21622,#21623,#21624,#21625,
#21626,#21627,#21628,#21629,#21630,#21631,#21632,#21633,#21634,#21635,#21636,
#21637,#21638,#21639,#21640,#21641,#21642,#21643,#21644,#21645,#21646,#21647,
#21648,#21649,#21650,#21651,#21652,#21653,#21654,#21655,#21656,#21657,#21658,
#21659,#21660,#21661,#21662,#21663,#21664,#21665,#21666,#21667,#21668,#21669,
#21670,#21671,#21672,#21673,#21674,#21675,#21676,#21677,#21678,#21679,#21680,
#21681,#21682,#21683,#21684,#21685,#21686,#21687),.UNSPECIFIED.,.F.,.F.,
(4,3,3,3,3,3,3,3,3,3,3,3,3,3,3,3,3,3,3,3,3,3,3,3,3,3,3,3,3,3,3,3,3,4),(2.02058687755678,
2.14069438238532,2.2574883425309,2.37416635199786,2.49077964507473,2.61344646285233,
2.73016277784316,2.84695211083585,2.96394200550359,2.9814469161851,3.09930457100341,
3.21695263862805,3.33448562654666,3.45195319760804,3.56940490710038,3.68697299397692,
3.80460662818603,3.92245632155603,3.97526255491346,4.09286106442566,4.21024287633558,
4.32750544285481,4.44469896657569,4.56187353699821,4.67916203298068,4.79651428555477,
4.91408310460292,4.96907819364183,5.08674497378225,5.2042322284644,5.32160189552125,
5.43889690344537,5.55623184519139,5.66526454987602),.UNSPECIFIED.);
#217=B_SPLINE_CURVE_WITH_KNOTS('',3,(#21690,#21691,#21692,#21693,#21694,
#21695,#21696,#21697,#21698,#21699,#21700,#21701,#21702,#21703,#21704,#21705,
#21706,#21707,#21708,#21709,#21710,#21711,#21712,#21713,#21714,#21715,#21716,
#21717,#21718,#21719,#21720,#21721,#21722,#21723,#21724,#21725,#21726,#21727,
#21728,#21729,#21730,#21731,#21732,#21733,#21734,#21735,#21736,#21737,#21738,
#21739,#21740,#21741,#21742,#21743,#21744),.UNSPECIFIED.,.F.,.F.,(4,3,3,
3,3,3,3,3,3,3,3,3,3,3,3,3,3,3,4),(5.66526454987602,5.78270914137197,5.90037195798557,
5.9628938323702,6.08059634138301,6.19808452175179,6.31545483179508,6.4327572635203,
6.55004169773963,6.66744062916035,6.78490380112927,6.90258299960002,6.95670947109856,
7.07493575073346,7.19296502881277,7.31083750640158,7.42861915180826,7.54637977656283,
7.59274844815668),.UNSPECIFIED.);
#218=B_SPLINE_CURVE_WITH_KNOTS('',3,(#21745,#21746,#21747,#21748,#21749,
#21750,#21751,#21752,#21753,#21754,#21755,#21756,#21757,#21758,#21759,#21760,
#21761,#21762,#21763,#21764,#21765,#21766,#21767,#21768,#21769,#21770,#21771,
#21772,#21773,#21774,#21775,#21776,#21777,#21778,#21779,#21780,#21781,#21782,
#21783,#21784,#21785,#21786,#21787,#21788,#21789,#21790,#21791,#21792,#21793,
#21794,#21795,#21796,#21797,#21798,#21799,#21800,#21801,#21802,#21803,#21804,
#21805,#21806,#21807,#21808,#21809,#21810,#21811,#21812,#21813,#21814,#21815,
#21816,#21817,#21818,#21819,#21820,#21821,#21822,#21823,#21824,#21825,#21826,
#21827,#21828,#21829,#21830,#21831,#21832,#21833,#21834,#21835,#21836,#21837,
#21838,#21839,#21840,#21841,#21842,#21843,#21844,#21845,#21846,#21847,#21848,
#21849,#21850,#21851,#21852,#21853,#21854,#21855,#21856,#21857,#21858,#21859,
#21860,#21861,#21862,#21863,#21864,#21865),.UNSPECIFIED.,.F.,.F.,(4,3,3,
3,3,3,3,3,3,3,3,3,3,3,3,3,3,3,3,3,3,3,3,3,3,3,3,3,3,3,3,3,3,3,3,3,3,3,3,
3,4),(7.59274844886418,7.72611340783759,7.86064797894208,7.95052510982693,
8.06821292749181,8.18568587942327,8.30304064157112,8.42032723670827,8.53759557598362,
8.65497815000861,8.77242479148122,8.89008738406618,8.94434074855529,9.06202865632316,
9.17950175858101,9.2968567083081,9.4141435278905,9.53141212813995,9.64879501639168,
9.76624200300912,9.88390498447909,9.93815638728366,10.0558403825393,10.1733094914499,
10.2906604012616,10.4079431422432,10.5252076330259,10.64258639774,10.7600292469684,
10.8776881175203,10.931972026012,11.0496601185419,11.1671333352003,11.2844883556557,
11.4017752024163,11.5190437863578,11.6364265931865,11.753873461037,11.8715362679689,
11.9257876647404,11.9490926668048),.UNSPECIFIED.);
#219=B_SPLINE_CURVE_WITH_KNOTS('',3,(#21866,#21867,#21868,#21869,#21870,
#21871,#21872,#21873,#21874,#21875,#21876,#21877,#21878,#21879,#21880,#21881,
#21882,#21883,#21884,#21885,#21886,#21887,#21888,#21889,#21890,#21891,#21892,
#21893,#21894,#21895,#21896,#21897,#21898,#21899,#21900,#21901,#21902,#21903,
#21904,#21905,#21906,#21907,#21908,#21909,#21910,#21911,#21912,#21913,#21914,
#21915,#21916,#21917,#21918,#21919,#21920,#21921,#21922,#21923,#21924,#21925,
#21926,#21927,#21928,#21929,#21930,#21931,#21932,#21933,#21934,#21935,#21936,
#21937,#21938,#21939,#21940,#21941,#21942,#21943,#21944,#21945,#21946,#21947,
#21948,#21949,#21950,#21951,#21952,#21953,#21954,#21955,#21956,#21957,#21958,
#21959,#21960,#21961,#21962,#21963,#21964,#21965,#21966,#21967,#21968,#21969,
#21970,#21971,#21972,#21973,#21974,#21975,#21976,#21977,#21978,#21979,#21980,
#21981),.UNSPECIFIED.,.F.,.F.,(4,2,2,2,2,2,2,2,2,2,2,2,2,2,2,2,2,2,2,2,
2,2,2,2,2,2,2,2,2,2,2,2,2,2,2,2,2,2,2,2,2,2,2,2,2,2,2,2,2,2,2,2,2,2,2,2,
2,4),(-1.04037338208336,-1.01416486516127,-1.00744323031407,-1.00046946854683,
-0.982039197890212,-0.955050450349102,-0.944205438114775,-0.933083306916604,
-0.920904741459413,-0.89275188124582,-0.884043275220523,-0.877984441360367,
-0.86695472795474,-0.848332082510172,-0.828046102010566,-0.817400977669383,
-0.805932927745472,-0.793039841365782,-0.767332053338507,-0.758341227968803,
-0.752290486521731,-0.741660020946498,-0.724361000924324,-0.702356242192692,
-0.691680270784957,-0.680246589919544,-0.667433930200241,-0.640695271885177,
-0.632132676579121,-0.626083321967545,-0.614911668518366,-0.595773221647233,
-0.576054912027885,-0.565466688275944,-0.554063772130212,-0.541261442307823,
-0.515538966811059,-0.506474430913304,-0.500432128228809,-0.489967423045582,
-0.473230155228666,-0.450247884308502,-0.439529294467034,-0.428019884225815,
-0.415086509727082,-0.389363599518028,-0.380374027295732,-0.374236477857763,
-0.363021236863976,-0.34370408892813,-0.32493567686722,-0.314248850844133,
-0.302594879257175,-0.289393172738,-0.263741215039427,-0.254941422894619,
-0.249100921729546,-0.244154988360166),.UNSPECIFIED.);
#220=B_SPLINE_CURVE_WITH_KNOTS('',3,(#21984,#21985,#21986,#21987,#21988,
#21989,#21990,#21991,#21992,#21993,#21994,#21995,#21996,#21997,#21998,#21999,
#22000,#22001,#22002,#22003,#22004,#22005,#22006,#22007,#22008,#22009,#22010,
#22011,#22012,#22013,#22014,#22015,#22016,#22017,#22018,#22019,#22020,#22021,
#22022,#22023,#22024,#22025,#22026,#22027,#22028,#22029,#22030,#22031,#22032,
#22033,#22034,#22035,#22036,#22037,#22038,#22039,#22040,#22041,#22042,#22043,
#22044,#22045,#22046,#22047,#22048,#22049,#22050,#22051,#22052,#22053,#22054,
#22055,#22056,#22057,#22058,#22059,#22060,#22061,#22062,#22063,#22064,#22065,
#22066,#22067,#22068,#22069,#22070,#22071,#22072,#22073,#22074,#22075,#22076,
#22077,#22078,#22079,#22080,#22081,#22082,#22083,#22084,#22085,#22086,#22087,
#22088,#22089,#22090,#22091,#22092,#22093,#22094,#22095),.UNSPECIFIED.,
 .F.,.F.,(4,3,3,3,3,3,3,3,3,3,3,3,3,3,3,3,3,3,3,3,3,3,3,3,3,3,3,3,3,3,3,
3,3,3,3,3,3,4),(17.9342486843494,18.0460353769573,18.1577136094561,18.2693264455941,
18.3809168546533,18.4926092698599,18.6043503990142,18.7163045388962,18.8120707346779,
18.9240343718639,19.0358000525972,19.1474553228003,19.2590432973348,19.3706069942819,
19.4822713317926,19.5939828088423,19.7059086614885,19.8058863734063,19.9178610297847,
20.0296379318187,20.1413045382507,20.2529039436819,20.3644791460784,20.476155012835,
20.5878780507119,20.6998153673571,20.7997020121347,20.9116767539539,21.023453796993,
21.13512057818,21.2467201917801,21.3582956354648,21.4699717937486,21.5816951511915,
21.6936328307661,21.793517650863,21.9536039852106,21.9911485751285),
 .UNSPECIFIED.);
#221=B_SPLINE_CURVE_WITH_KNOTS('',3,(#22096,#22097,#22098,#22099,#22100,
#22101,#22102,#22103,#22104,#22105,#22106,#22107,#22108,#22109,#22110,#22111,
#22112,#22113,#22114,#22115,#22116,#22117,#22118,#22119,#22120,#22121,#22122,
#22123,#22124,#22125,#22126,#22127,#22128,#22129,#22130,#22131,#22132,#22133,
#22134,#22135,#22136,#22137,#22138,#22139,#22140,#22141,#22142,#22143,#22144,
#22145,#22146,#22147,#22148,#22149,#22150,#22151,#22152,#22153,#22154,#22155,
#22156,#22157,#22158,#22159),.UNSPECIFIED.,.F.,.F.,(4,3,3,3,3,3,3,3,3,3,
3,3,3,3,3,3,3,3,3,3,3,4),(21.9911485755232,22.1013010399507,22.2113543241301,
22.321353793377,22.4313447204739,22.5414427825285,22.6516063753035,22.7619557132656,
22.7873332895914,22.8993082072233,23.011085361148,23.1227522136722,23.2343518591702,
23.3459272953745,23.457603384788,23.5693266395644,23.6812641611206,23.7811489283198,
23.8930847227604,24.0048672469585,24.1165374946164,24.2171454613693),
 .UNSPECIFIED.);
#222=B_SPLINE_CURVE_WITH_KNOTS('',3,(#22161,#22162,#22163,#22164,#22165,
#22166,#22167,#22168,#22169,#22170,#22171,#22172,#22173,#22174,#22175,#22176,
#22177,#22178,#22179,#22180,#22181,#22182,#22183,#22184,#22185,#22186,#22187,
#22188,#22189,#22190,#22191,#22192,#22193,#22194,#22195,#22196,#22197,#22198,
#22199,#22200,#22201,#22202,#22203,#22204,#22205,#22206,#22207,#22208,#22209,
#22210,#22211,#22212,#22213,#22214,#22215,#22216,#22217,#22218,#22219,#22220,
#22221),.UNSPECIFIED.,.F.,.F.,(4,3,3,3,3,3,3,3,3,3,3,3,3,3,3,3,3,3,3,3,
4),(21.9911485755562,22.1180393250501,22.2460227144172,22.3489252367988,
22.460899892698,22.5726767942465,22.6843434001895,22.795942805129,22.9075180070322,
23.0191938732966,23.1309169106812,23.2428542268404,23.3427408755272,23.4546767726727,
23.5664551376927,23.6781192288063,23.7897121490916,23.9013304775244,24.0129558539189,
24.124723624456,24.2164750170476),.UNSPECIFIED.);
#223=B_SPLINE_CURVE_WITH_KNOTS('',3,(#22222,#22223,#22224,#22225,#22226,
#22227,#22228,#22229,#22230,#22231,#22232,#22233,#22234,#22235,#22236,#22237,
#22238,#22239,#22240,#22241,#22242,#22243,#22244,#22245,#22246,#22247,#22248,
#22249,#22250,#22251,#22252,#22253,#22254,#22255,#22256,#22257,#22258,#22259,
#22260,#22261,#22262,#22263,#22264,#22265,#22266,#22267,#22268,#22269,#22270,
#22271,#22272,#22273,#22274,#22275,#22276,#22277,#22278,#22279,#22280,#22281,
#22282,#22283,#22284,#22285,#22286,#22287,#22288,#22289,#22290,#22291,#22292,
#22293,#22294,#22295,#22296,#22297,#22298,#22299,#22300,#22301,#22302,#22303,
#22304,#22305,#22306,#22307,#22308,#22309,#22310,#22311,#22312,#22313,#22314,
#22315,#22316,#22317,#22318,#22319,#22320,#22321,#22322,#22323,#22324,#22325,
#22326,#22327,#22328,#22329,#22330,#22331,#22332,#22333),.UNSPECIFIED.,
 .F.,.F.,(4,3,3,3,3,3,3,3,3,3,3,3,3,3,3,3,3,3,3,3,3,3,3,3,3,3,3,3,3,3,3,
3,3,3,3,3,3,4),(17.9335641972525,18.0454147314152,18.1573118896217,18.2694253463682,
18.3736626818853,18.4855523651012,18.5972426043066,18.708821580402,18.8203325429781,
18.9318186437399,19.0434050927939,19.155038394354,19.2668866007134,19.3674783206137,
19.4794577481211,19.5912392235406,19.7029102794142,19.8145140022681,19.9260933818471,
20.0377731699916,20.1494999951527,20.2614408219124,20.3612939593421,20.4732825933969,
20.5850739685693,20.6967553393691,20.80836977387,20.9199602438703,21.0316516298248,
21.1433903498293,21.2553434208536,21.3551095980704,21.4675965762727,21.5799041453604,
21.6920651091871,21.8041390505535,21.9161934578611,21.9911485751285),
 .UNSPECIFIED.);
#224=B_SPLINE_CURVE_WITH_KNOTS('',3,(#22431,#22432,#22433,#22434,#22435,
#22436,#22437,#22438,#22439,#22440,#22441,#22442,#22443,#22444,#22445,#22446,
#22447,#22448,#22449,#22450,#22451,#22452,#22453,#22454,#22455,#22456,#22457,
#22458,#22459,#22460,#22461,#22462,#22463,#22464,#22465,#22466,#22467,#22468,
#22469,#22470,#22471,#22472,#22473,#22474,#22475,#22476,#22477,#22478,#22479,
#22480,#22481,#22482,#22483,#22484,#22485,#22486,#22487,#22488,#22489,#22490,
#22491,#22492,#22493,#22494,#22495,#22496,#22497,#22498,#22499,#22500,#22501,
#22502,#22503,#22504,#22505,#22506,#22507,#22508,#22509),.UNSPECIFIED.,
 .F.,.F.,(4,3,3,3,3,3,3,3,3,3,3,3,3,3,3,3,3,3,3,3,3,3,3,3,3,3,4),(0.,0.0183580651845695,
0.036716130369139,0.0506017132143072,0.0580120633809709,0.061133863191812,
0.078888287650872,0.0962814561595988,0.113365607257946,0.115724847189734,
0.119100212910273,0.135939557864133,0.147800793130485,0.16459229773457,
0.16938312183736,0.173083969688032,0.189885224893387,0.206611596082267,
0.216904963728089,0.222249975046034,0.226244647397093,0.242353326253545,
0.253193326851421,0.258082573110125,0.273549000401955,0.28213282996317,
0.286347380332243),.UNSPECIFIED.);
#225=B_SPLINE_CURVE_WITH_KNOTS('',3,(#22510,#22511,#22512,#22513,#22514,
#22515,#22516,#22517,#22518,#22519,#22520,#22521,#22522,#22523,#22524,#22525,
#22526,#22527,#22528,#22529,#22530,#22531,#22532,#22533,#22534,#22535,#22536,
#22537,#22538,#22539,#22540,#22541,#22542,#22543,#22544,#22545,#22546,#22547,
#22548,#22549,#22550,#22551,#22552,#22553,#22554,#22555,#22556,#22557,#22558,
#22559,#22560,#22561,#22562,#22563,#22564,#22565,#22566,#22567,#22568,#22569,
#22570,#22571,#22572,#22573,#22574,#22575,#22576,#22577,#22578,#22579,#22580,
#22581,#22582,#22583,#22584,#22585,#22586,#22587,#22588,#22589,#22590,#22591),
 .UNSPECIFIED.,.F.,.F.,(4,3,3,3,3,3,3,3,3,3,3,3,3,3,3,3,3,3,3,3,3,3,3,3,
3,3,3,4),(0.,0.0152191826672047,0.0310202687211212,0.04375636479767,0.0495387926916016,
0.0521713451608324,0.0684720803979817,0.0850884502494136,0.0971737854436662,
0.102033598682943,0.105097613961339,0.122175006430196,0.133459759972985,
0.150102685928275,0.154678331388736,0.158573680555885,0.175808037359126,
0.193042394162367,0.203920050772197,0.209203196649001,0.212511486881768,
0.215892595181776,0.233891080174088,0.246493248602607,0.251402765189765,
0.269591385970374,0.280063647041007,0.285110649527642),.UNSPECIFIED.);
#226=B_SPLINE_CURVE_WITH_KNOTS('',3,(#22592,#22593,#22594,#22595),
 .UNSPECIFIED.,.F.,.F.,(4,4),(-0.0158762351372481,0.),.UNSPECIFIED.);
#227=B_SPLINE_CURVE_WITH_KNOTS('',3,(#22692,#22693,#22694,#22695,#22696,
#22697,#22698,#22699,#22700,#22701,#22702,#22703,#22704,#22705,#22706,#22707,
#22708,#22709,#22710,#22711,#22712,#22713,#22714,#22715,#22716,#22717,#22718,
#22719,#22720,#22721,#22722,#22723,#22724,#22725,#22726,#22727,#22728,#22729,
#22730,#22731,#22732,#22733,#22734,#22735,#22736,#22737,#22738,#22739,#22740,
#22741,#22742,#22743,#22744,#22745,#22746,#22747,#22748,#22749,#22750,#22751,
#22752,#22753,#22754,#22755,#22756,#22757,#22758,#22759,#22760,#22761,#22762,
#22763,#22764,#22765,#22766,#22767,#22768,#22769,#22770,#22771,#22772,#22773),
 .UNSPECIFIED.,.F.,.F.,(4,3,3,3,3,3,3,3,3,3,3,3,3,3,3,3,3,3,3,3,3,3,3,3,
3,3,3,4),(0.,0.0151292672762648,0.0309291876229029,0.0437563608992012,0.0495387785849296,
0.0521713220847718,0.0686327765216655,0.0850784343717207,0.0971737657720376,
0.102033478715591,0.105097599596628,0.122174992255498,0.133459759972988,
0.150102687023667,0.15467833266872,0.158573680648776,0.175475135361472,
0.192932046543207,0.203920052454413,0.209203197488932,0.212511489653267,
0.215892595761394,0.233891634235224,0.246493249744474,0.251402765817797,
0.26959138653037,0.280063647041022,0.285131254558132),.UNSPECIFIED.);
#228=B_SPLINE_CURVE_WITH_KNOTS('',3,(#22774,#22775,#22776,#22777,#22778,
#22779,#22780,#22781,#22782,#22783,#22784,#22785,#22786,#22787,#22788,#22789,
#22790,#22791,#22792,#22793,#22794,#22795,#22796,#22797,#22798,#22799,#22800,
#22801,#22802,#22803,#22804,#22805,#22806,#22807,#22808,#22809,#22810,#22811,
#22812,#22813,#22814,#22815,#22816,#22817,#22818,#22819,#22820,#22821,#22822,
#22823,#22824,#22825,#22826,#22827,#22828,#22829,#22830,#22831,#22832,#22833,
#22834,#22835,#22836,#22837,#22838,#22839,#22840,#22841,#22842,#22843,#22844,
#22845,#22846,#22847,#22848,#22849,#22850,#22851,#22852),.UNSPECIFIED.,
 .F.,.F.,(4,3,3,3,3,3,3,3,3,3,3,3,3,3,3,3,3,3,3,3,3,3,3,3,3,3,4),(0.,0.0178407499527946,
0.0360809481309363,0.0506017130354889,0.0580120628747047,0.0611338628652755,
0.0788642583998809,0.0962814563820097,0.109161290569129,0.115724846961747,
0.119100212712732,0.135939558238763,0.147800793130486,0.164592297734572,
0.169383121808608,0.173083969711458,0.189885224767986,0.206611595947546,
0.2169049630076,0.222249974985313,0.226244647539912,0.242339285647356,0.253193327942412,
0.258082573330392,0.273549001447499,0.282132829963172,0.286347380332245),
 .UNSPECIFIED.);
#229=B_SPLINE_CURVE_WITH_KNOTS('',3,(#22897,#22898,#22899,#22900,#22901,
#22902,#22903,#22904,#22905,#22906,#22907,#22908,#22909,#22910,#22911,#22912,
#22913,#22914,#22915,#22916,#22917,#22918,#22919,#22920,#22921,#22922,#22923,
#22924,#22925,#22926,#22927,#22928,#22929,#22930,#22931,#22932,#22933,#22934,
#22935,#22936,#22937,#22938,#22939,#22940,#22941,#22942,#22943,#22944,#22945,
#22946,#22947,#22948,#22949,#22950,#22951,#22952,#22953,#22954,#22955,#22956,
#22957,#22958,#22959,#22960,#22961,#22962,#22963,#22964,#22965,#22966,#22967,
#22968,#22969,#22970,#22971,#22972,#22973,#22974,#22975,#22976,#22977,#22978,
#22979,#22980,#22981,#22982,#22983,#22984,#22985,#22986,#22987,#22988,#22989,
#22990,#22991,#22992,#22993,#22994,#22995,#22996,#22997,#22998,#22999,#23000,
#23001,#23002,#23003,#23004,#23005,#23006),.UNSPECIFIED.,.F.,.F.,(4,2,2,
2,2,2,2,2,2,2,2,2,2,2,2,2,2,2,2,2,2,2,2,2,2,2,2,2,2,2,2,2,2,2,2,2,2,2,2,
2,2,2,2,2,2,2,2,2,2,2,2,2,2,2,4),(-0.388501056592863,-0.386820572871954,
-0.37137009344835,-0.346422087251238,-0.343921258609954,-0.342711393673856,
-0.3418454804417,-0.340904563019323,-0.33953517948609,-0.335881943037683,
-0.330289052303747,-0.310335625674568,-0.289142186338472,-0.285999939238393,
-0.283978855303575,-0.282356169521994,-0.280505558685679,-0.277309325459776,
-0.262246632946139,-0.247209707985575,-0.243654292750582,-0.228032928473727,
-0.226105223025318,-0.224926585294603,-0.224011568002013,-0.222935252360905,
-0.220965990434522,-0.209786460207454,-0.193816832175384,-0.171678092584887,
-0.168540235746571,-0.166508234742227,-0.164867556447226,-0.162986029098486,
-0.159708544545876,-0.143440725523142,-0.129248288257582,-0.112150650603508,
-0.109143404207764,-0.107951343042863,-0.10701247453129,-0.106034759822587,
-0.10460473073509,-0.102883612375124,-0.0996310274333393,-0.0913975068235331,
-0.0670909053345679,-0.0552672459457108,-0.0521232458976062,-0.0502599305992454,
-0.0487650651937886,-0.0467406787382857,-0.0428350448067549,-0.022839327136288,
-0.00170946157028903),.UNSPECIFIED.);
#230=B_SPLINE_CURVE_WITH_KNOTS('',3,(#23009,#23010,#23011,#23012,#23013,
#23014,#23015,#23016,#23017,#23018,#23019,#23020,#23021,#23022,#23023,#23024,
#23025,#23026,#23027,#23028,#23029,#23030,#23031,#23032,#23033,#23034,#23035,
#23036,#23037,#23038,#23039,#23040,#23041,#23042,#23043,#23044,#23045,#23046,
#23047,#23048,#23049,#23050,#23051,#23052,#23053,#23054,#23055,#23056,#23057,
#23058,#23059,#23060,#23061,#23062,#23063),.UNSPECIFIED.,.F.,.F.,(4,3,3,
3,3,3,3,3,3,3,3,3,3,3,3,3,3,3,4),(11.6159397475004,11.7400323994672,11.8624742267738,
11.9848874271838,12.107314791651,12.2326563345468,12.3553366947763,12.4820088290054,
12.6086809632344,12.7327736152012,12.851232493043,12.9695575437606,13.087803548112,
13.2060251446645,13.3243597220786,13.4427610123004,13.5613799833078,13.6014221789684,
13.6623826713879),.UNSPECIFIED.);
#231=B_SPLINE_CURVE_WITH_KNOTS('',3,(#23068,#23069,#23070,#23071,#23072,
#23073,#23074,#23075,#23076,#23077,#23078,#23079,#23080,#23081,#23082,#23083,
#23084,#23085,#23086,#23087,#23088,#23089,#23090,#23091,#23092,#23093,#23094,
#23095,#23096,#23097,#23098,#23099,#23100,#23101,#23102,#23103,#23104,#23105,
#23106,#23107,#23108,#23109,#23110,#23111,#23112,#23113,#23114,#23115,#23116,
#23117,#23118,#23119,#23120,#23121,#23122,#23123,#23124,#23125,#23126,#23127,
#23128,#23129,#23130,#23131,#23132,#23133,#23134,#23135,#23136,#23137,#23138,
#23139,#23140,#23141,#23142,#23143,#23144,#23145,#23146,#23147,#23148,#23149,
#23150,#23151,#23152,#23153,#23154,#23155,#23156,#23157,#23158,#23159,#23160,
#23161,#23162,#23163,#23164,#23165,#23166,#23167,#23168,#23169,#23170,#23171,
#23172,#23173,#23174,#23175,#23176,#23177,#23178,#23179,#23180,#23181,#23182,
#23183,#23184,#23185,#23186,#23187,#23188,#23189,#23190,#23191,#23192,#23193,
#23194,#23195,#23196,#23197,#23198,#23199,#23200,#23201,#23202,#23203,#23204,
#23205,#23206,#23207,#23208,#23209,#23210,#23211,#23212,#23213,#23214,#23215,
#23216,#23217,#23218,#23219,#23220,#23221,#23222,#23223,#23224,#23225,#23226,
#23227,#23228,#23229,#23230,#23231,#23232,#23233,#23234,#23235,#23236,#23237,
#23238,#23239,#23240,#23241,#23242,#23243,#23244,#23245,#23246,#23247,#23248,
#23249,#23250,#23251,#23252,#23253,#23254,#23255,#23256,#23257,#23258,#23259,
#23260,#23261,#23262,#23263,#23264,#23265,#23266,#23267,#23268,#23269,#23270,
#23271,#23272,#23273,#23274,#23275,#23276,#23277,#23278,#23279,#23280,#23281,
#23282,#23283,#23284,#23285,#23286,#23287),.UNSPECIFIED.,.F.,.F.,(4,2,2,
2,2,2,2,2,2,2,2,2,2,2,2,2,2,2,2,2,2,2,2,2,2,2,2,2,2,2,2,2,2,2,2,2,2,2,2,
2,2,2,2,2,2,2,2,2,2,2,2,2,2,2,2,2,2,2,2,2,2,2,2,2,2,2,2,2,2,2,2,2,2,2,2,
2,2,2,2,2,2,2,2,2,2,2,2,2,2,2,2,2,2,2,2,2,2,2,2,2,2,2,2,2,2,2,2,2,2,4),
(-1.13048491284919,-1.11742794727068,-1.11149198614902,-1.10702303107772,
-1.10490648610305,-1.10326505430796,-1.10145250216885,-1.09846406594016,
-1.08815110668756,-1.05798398520967,-1.0515135693742,-1.0474498029415,-1.04601701513843,
-1.04505926622458,-1.0442035640373,-1.04303259822145,-1.04008464381358,
-1.01887948305155,-1.00106301949291,-0.994659836513761,-0.989922397528697,
-0.98775646149669,-0.986108517098755,-0.984320033889488,-0.981441648574161,
-0.972173535529898,-0.947158676525079,-0.931458748178385,-0.9293662738169,
-0.928265275729413,-0.927350577703114,-0.926200224605055,-0.924377206456902,
-0.913959809977621,-0.90548264528034,-0.891073174472189,-0.875027394424812,
-0.871770045965304,-0.86989889302085,-0.868266713289335,-0.866244654298588,
-0.863121143913001,-0.84044750521824,-0.823088340431133,-0.816896597038623,
-0.81295901391849,-0.811543168567195,-0.810588792820048,-0.809729485834232,
-0.808545655586117,-0.805538298880899,-0.786555979884845,-0.767855788452594,
-0.757176428021775,-0.754262308099518,-0.752465443359327,-0.750818913694456,
-0.748704095477781,-0.744124291351968,-0.718297774601662,-0.703376021766843,
-0.698693728396099,-0.695486861899579,-0.694179963381556,-0.693246576081843,
-0.692363236406221,-0.690821456365581,-0.686300479467658,-0.678568926940036,
-0.66286883858718,-0.640953473960272,-0.637820624313029,-0.635796575481633,
-0.634165461383895,-0.632298477247327,-0.62905608813685,-0.613295493218393,
-0.589814136756139,-0.579623905635116,-0.577810701175702,-0.576663669346368,
-0.575749347912375,-0.574646052487432,-0.57254285101204,-0.556227058731184,
-0.52959774760129,-0.522113265644139,-0.519447865308257,-0.517878872190738,
-0.51622952295596,-0.514059603539153,-0.509304541808945,-0.502870030165085,
-0.484899961486914,-0.463920400614609,-0.460964544886845,-0.459788542767622,
-0.458930651950198,-0.457970143676417,-0.456535809789371,-0.452484206171058,
-0.446046225190043,-0.416260561592314,-0.405752168979231,-0.40274147907261,
-0.400921450622253,-0.399277008347685,-0.397161769427786,-0.392714962238584,
-0.388501056592863),.UNSPECIFIED.);
#232=B_SPLINE_CURVE_WITH_KNOTS('',3,(#23289,#23290,#23291,#23292,#23293,
#23294,#23295,#23296,#23297,#23298,#23299,#23300,#23301,#23302,#23303,#23304,
#23305,#23306,#23307,#23308,#23309,#23310,#23311,#23312,#23313,#23314,#23315,
#23316,#23317,#23318,#23319,#23320,#23321,#23322,#23323,#23324,#23325,#23326,
#23327,#23328,#23329,#23330,#23331,#23332,#23333,#23334,#23335,#23336,#23337,
#23338,#23339,#23340,#23341,#23342,#23343),.UNSPECIFIED.,.F.,.F.,(4,3,3,
3,3,3,3,3,3,3,3,3,3,3,3,3,3,3,4),(13.6623826713879,13.7821802303794,13.9018303726072,
14.021385637802,14.1408984130057,14.2605090576095,14.3801661535387,14.5000537598878,
14.5941633947024,14.7182560466692,14.838042915424,14.957714639234,15.0773235113992,
15.1969217157567,15.3166434180951,15.4364397332535,15.5564514304154,15.5869046104364,
15.7079632679489),.UNSPECIFIED.);
#233=B_SPLINE_CURVE_WITH_KNOTS('',3,(#23344,#23345,#23346,#23347,#23348,
#23349,#23350,#23351,#23352,#23353,#23354,#23355,#23356,#23357,#23358,#23359,
#23360,#23361,#23362,#23363,#23364,#23365,#23366,#23367,#23368,#23369,#23370,
#23371,#23372,#23373,#23374,#23375,#23376,#23377,#23378,#23379,#23380,#23381,
#23382,#23383,#23384,#23385,#23386,#23387,#23388,#23389,#23390,#23391,#23392,
#23393,#23394,#23395,#23396,#23397,#23398,#23399,#23400,#23401,#23402,#23403,
#23404,#23405,#23406,#23407,#23408,#23409,#23410,#23411,#23412,#23413,#23414,
#23415,#23416,#23417,#23418,#23419,#23420,#23421,#23422,#23423,#23424,#23425,
#23426,#23427,#23428,#23429,#23430,#23431,#23432,#23433,#23434,#23435,#23436,
#23437,#23438,#23439,#23440,#23441,#23442,#23443,#23444,#23445,#23446,#23447,
#23448,#23449,#23450,#23451,#23452,#23453,#23454,#23455,#23456,#23457,#23458,
#23459,#23460,#23461,#23462,#23463,#23464,#23465,#23466,#23467,#23468,#23469,
#23470,#23471,#23472,#23473,#23474,#23475,#23476,#23477,#23478,#23479,#23480,
#23481,#23482,#23483),.UNSPECIFIED.,.F.,.F.,(4,2,2,2,2,2,2,2,2,2,2,2,2,
2,2,2,2,2,2,2,2,2,2,2,2,2,2,2,2,2,2,2,2,2,2,2,2,2,2,2,2,2,2,2,2,2,2,2,2,
2,2,2,2,2,2,2,2,2,2,2,2,2,2,2,2,2,2,2,2,4),(-1.48450431841139,-1.4617611277698,
-1.44593454243558,-1.44270146431909,-1.44084323355285,-1.43922191691824,
-1.43721299573973,-1.4341097721629,-1.41163255113375,-1.39460054757425,
-1.38792774329617,-1.38511883993771,-1.38357795582617,-1.38228274348412,
-1.38135413076546,-1.38049548623494,-1.37931282111924,-1.37630565299905,
-1.35709232231919,-1.33852275952823,-1.32787689803448,-1.32496269215979,
-1.3231639751169,-1.32151450789825,-1.31939411267224,-1.31496062846687,
-1.28792632392131,-1.28256676732013,-1.26913107652234,-1.26624202927492,
-1.26498603957276,-1.26405865092523,-1.26302279612381,-1.26123676704593,
-1.25448185427391,-1.22352839734419,-1.2152993451098,-1.20957414247627,
-1.20724074097352,-1.20556474688588,-1.20403794966868,-1.20198652284865,
-1.1979800448179,-1.17021122788282,-1.15122108808407,-1.14876189022007,
-1.14758739428054,-1.14667172596313,-1.14559123102855,-1.1436486425439,
-1.13424769144913,-1.10318744586674,-1.09667715799843,-1.09188003707794,
-1.08970459528864,-1.08805657154721,-1.08649295753002,-1.08384691224912,
-1.07648685911044,-1.04634008698229,-1.03744853444824,-1.03238243373507,
-1.03082950190625,-1.02984645520666,-1.02891019607728,-1.02775551794013,
-1.02491673169677,-1.00161398686935,-0.98519209668673,-0.984038713564579),
 .UNSPECIFIED.);
#234=B_SPLINE_CURVE_WITH_KNOTS('',3,(#23489,#23490,#23491,#23492,#23493,
#23494,#23495,#23496,#23497,#23498,#23499,#23500,#23501,#23502,#23503,#23504,
#23505,#23506,#23507,#23508,#23509,#23510,#23511,#23512,#23513,#23514,#23515,
#23516,#23517,#23518,#23519,#23520,#23521,#23522,#23523,#23524,#23525,#23526,
#23527,#23528,#23529,#23530,#23531,#23532,#23533,#23534,#23535,#23536,#23537,
#23538,#23539,#23540,#23541,#23542,#23543,#23544,#23545,#23546,#23547,#23548,
#23549,#23550,#23551,#23552,#23553,#23554,#23555,#23556,#23557,#23558,#23559,
#23560,#23561,#23562,#23563,#23564,#23565,#23566,#23567,#23568,#23569,#23570,
#23571,#23572,#23573,#23574,#23575,#23576,#23577,#23578,#23579,#23580,#23581,
#23582,#23583,#23584,#23585,#23586,#23587,#23588,#23589,#23590,#23591,#23592,
#23593,#23594,#23595,#23596,#23597,#23598,#23599,#23600,#23601,#23602,#23603,
#23604,#23605,#23606,#23607,#23608,#23609,#23610,#23611,#23612,#23613,#23614,
#23615,#23616,#23617,#23618,#23619,#23620,#23621,#23622,#23623,#23624,#23625,
#23626,#23627,#23628,#23629,#23630,#23631,#23632,#23633,#23634,#23635,#23636,
#23637,#23638),.UNSPECIFIED.,.F.,.F.,(4,2,2,2,2,2,2,2,2,2,2,2,2,2,2,2,2,
2,2,2,2,2,2,2,2,2,2,2,2,2,2,2,2,2,2,2,2,2,2,2,2,2,2,2,2,2,2,2,2,2,2,2,2,
2,2,2,2,2,2,2,2,2,2,2,2,2,2,2,2,2,2,2,2,2,4),(-0.500694290278421,-0.497544488839605,
-0.495661357712548,-0.494492855323991,-0.493577002111409,-0.492490318556005,
-0.490466592203038,-0.477635817997283,-0.450094696254809,-0.440460302827894,
-0.43754182682963,-0.435744348790431,-0.43409863601131,-0.431950875806821,
-0.427314837357559,-0.421089139902201,-0.404126478228909,-0.381615394886978,
-0.378732636295032,-0.377570103137111,-0.376631545134818,-0.375650242287218,
-0.374108812827463,-0.369157227320466,-0.360566245051619,-0.334195806293179,
-0.323454453464546,-0.320412665249448,-0.318588298903664,-0.316949154199797,
-0.314853604473625,-0.310496759497856,-0.29347823375238,-0.274938529477881,
-0.263042839324536,-0.261166737053334,-0.260000367426982,-0.259084697255278,
-0.257996465962969,-0.255965256627442,-0.242880573285268,-0.212774006368426,
-0.205413445051682,-0.202765646017531,-0.20120052361162,-0.199550537622462,
-0.197371856384937,-0.192564705549658,-0.186037725262247,-0.154809411223525,
-0.145559982481404,-0.143624090127548,-0.142544422462605,-0.141627900072442,
-0.140473796262541,-0.138125815294119,-0.134961992463785,-0.127016727340287,
-0.100132859293806,-0.0889853560230274,-0.0859190418261268,-0.0840893010749391,
-0.0824511641418156,-0.0803649250865898,-0.0763578945436618,-0.0593578073915818,
-0.0449503960643063,-0.0286364519733591,-0.0267012887693669,-0.0255173386469702,
-0.0246003609189633,-0.023525195211802,-0.0223774179293482,-0.0205702953880954,
-0.000340360879008273),.UNSPECIFIED.);
#235=B_SPLINE_CURVE_WITH_KNOTS('',3,(#23639,#23640,#23641,#23642,#23643,
#23644,#23645,#23646,#23647,#23648,#23649,#23650,#23651,#23652,#23653,#23654,
#23655,#23656,#23657,#23658,#23659,#23660,#23661,#23662,#23663,#23664,#23665,
#23666,#23667,#23668,#23669,#23670,#23671,#23672,#23673,#23674,#23675,#23676,
#23677,#23678,#23679,#23680,#23681,#23682,#23683,#23684,#23685,#23686,#23687,
#23688,#23689,#23690,#23691,#23692,#23693,#23694,#23695,#23696,#23697,#23698,
#23699,#23700,#23701,#23702,#23703,#23704,#23705,#23706,#23707,#23708),
 .UNSPECIFIED.,.F.,.F.,(4,2,2,2,2,2,2,2,2,2,2,2,2,2,2,2,2,2,2,2,2,2,2,2,
2,2,2,2,2,2,2,2,2,2,4),(-1.37216423938497,-1.34558201548237,-1.34260950380171,
-1.34065849775233,-1.3387901421669,-1.33715832893005,-1.33513403494363,
-1.33200190257198,-1.31147073795144,-1.29387212379872,-1.28648518521141,
-1.28206143489466,-1.28060736088923,-1.27962515542679,-1.27868786372659,
-1.27752915199367,-1.27466699015011,-1.25191396248099,-1.23513446381467,
-1.22894897018639,-1.22437630025068,-1.22221853088604,-1.22057192564277,
-1.21878012495597,-1.21588577042803,-1.2064697950075,-1.1732599746904,-1.16539919001667,
-1.16360574159079,-1.16256895454495,-1.16164494831632,-1.16041970962888,
-1.15761540022164,-1.13307933462838,-1.13048491284919),.UNSPECIFIED.);
#236=B_SPLINE_CURVE_WITH_KNOTS('',3,(#23709,#23710,#23711,#23712,#23713,
#23714,#23715,#23716,#23717,#23718,#23719,#23720,#23721,#23722,#23723,#23724,
#23725,#23726,#23727,#23728,#23729,#23730,#23731,#23732,#23733,#23734,#23735,
#23736,#23737,#23738,#23739,#23740,#23741,#23742,#23743,#23744,#23745,#23746,
#23747,#23748,#23749,#23750,#23751,#23752,#23753,#23754,#23755,#23756,#23757,
#23758,#23759,#23760,#23761,#23762,#23763,#23764,#23765,#23766,#23767,#23768,
#23769,#23770,#23771,#23772,#23773,#23774,#23775,#23776,#23777,#23778,#23779,
#23780,#23781,#23782,#23783,#23784,#23785,#23786,#23787,#23788,#23789,#23790,
#23791,#23792,#23793,#23794,#23795,#23796,#23797,#23798,#23799,#23800,#23801,
#23802,#23803,#23804,#23805,#23806,#23807,#23808,#23809,#23810,#23811,#23812,
#23813,#23814,#23815,#23816,#23817,#23818,#23819,#23820,#23821,#23822,#23823,
#23824,#23825,#23826,#23827,#23828,#23829,#23830,#23831,#23832,#23833,#23834,
#23835,#23836,#23837,#23838,#23839,#23840,#23841,#23842,#23843,#23844,#23845,
#23846,#23847,#23848,#23849,#23850,#23851,#23852,#23853,#23854,#23855,#23856,
#23857,#23858,#23859,#23860,#23861,#23862,#23863,#23864,#23865,#23866,#23867,
#23868,#23869,#23870,#23871,#23872,#23873,#23874,#23875,#23876,#23877,#23878,
#23879,#23880,#23881,#23882,#23883,#23884,#23885,#23886,#23887,#23888,#23889,
#23890,#23891,#23892,#23893,#23894,#23895,#23896,#23897,#23898,#23899,#23900,
#23901,#23902,#23903,#23904,#23905,#23906,#23907,#23908,#23909,#23910,#23911,
#23912,#23913,#23914,#23915,#23916,#23917,#23918,#23919,#23920,#23921,#23922,
#23923,#23924,#23925,#23926,#23927,#23928,#23929,#23930),.UNSPECIFIED.,
 .F.,.F.,(4,2,2,2,2,2,2,2,2,2,2,2,2,2,2,2,2,2,2,2,2,2,2,2,2,2,2,2,2,2,2,
2,2,2,2,2,2,2,2,2,2,2,2,2,2,2,2,2,2,2,2,2,2,2,2,2,2,2,2,2,2,2,2,2,2,2,2,
2,2,2,2,2,2,2,2,2,2,2,2,2,2,2,2,2,2,2,2,2,2,2,2,2,2,2,2,2,2,2,2,2,2,2,2,
2,2,2,2,2,2,2,4),(-0.984038713564579,-0.979083382711775,-0.974514099266456,
-0.972378596647122,-0.970734461382103,-0.968930924076269,-0.965984892455485,
-0.956098893355456,-0.925490060350384,-0.918990582003603,-0.914913565602765,
-0.913478647123477,-0.912520177593105,-0.91166455259397,-0.910494325266551,
-0.90756634072051,-0.885984481222971,-0.868427902102175,-0.862078145649561,
-0.85737107091966,-0.855210580551665,-0.853563346040641,-0.851772278206197,
-0.848882273227625,-0.83950605601909,-0.814580008746206,-0.798913810932696,
-0.796821968301805,-0.795721125298328,-0.794806497580885,-0.79365615630539,
-0.791832943797292,-0.781406775136773,-0.772907111549027,-0.758429812593337,
-0.742480952275819,-0.739266899751719,-0.73738678374001,-0.735755776528335,
-0.733746710750133,-0.729829470622148,-0.724816977305916,-0.712860409646348,
-0.686724098553468,-0.68097019727523,-0.67928147801539,-0.678267767573056,
-0.677335980504339,-0.676038873637747,-0.672891576102773,-0.668325410868035,
-0.654043869396371,-0.627323133288759,-0.622797020398668,-0.620692447181739,
-0.619047800270467,-0.617246812812998,-0.614312051983835,-0.603382569448011,
-0.583879586004667,-0.565949166224158,-0.562936220062179,-0.561751739518097,
-0.560892520958884,-0.559938663596384,-0.558524818253106,-0.554600845578626,
-0.548439397457055,-0.531060002397481,-0.508378260428437,-0.505254989872259,
-0.503233037796786,-0.501600929657233,-0.499729844535093,-0.496472590770214,
-0.480430109939549,-0.466004582749208,-0.457518477831262,-0.44709677731593,
-0.445273444648482,-0.444122985930252,-0.443208241569681,-0.44210722014929,
-0.440014868547358,-0.424318411758726,-0.399308757887973,-0.390051168297601,
-0.387173762806587,-0.385385385252243,-0.383737198902599,-0.381570448161397,
-0.376829213981716,-0.370418754607422,-0.352568521687281,-0.331382310924339,
-0.328434538393741,-0.327262119328129,-0.326405992467733,-0.325448625648796,
-0.324017745883825,-0.319968283024939,-0.31353063342149,-0.29646643982214,
-0.273914165564096,-0.270788890007936,-0.268766344126854,-0.267134213645697,
-0.265263603785942,-0.262008475192572,-0.246010855207923,-0.242048471304312),
 .UNSPECIFIED.);
#237=B_SPLINE_CURVE_WITH_KNOTS('',3,(#23935,#23936,#23937,#23938,#23939,
#23940,#23941,#23942,#23943,#23944,#23945,#23946,#23947,#23948,#23949,#23950,
#23951,#23952,#23953,#23954,#23955,#23956,#23957,#23958,#23959,#23960,#23961,
#23962,#23963,#23964,#23965,#23966,#23967,#23968,#23969,#23970,#23971,#23972,
#23973,#23974,#23975,#23976,#23977,#23978,#23979,#23980,#23981,#23982,#23983,
#23984,#23985,#23986,#23987,#23988,#23989,#23990,#23991,#23992,#23993,#23994,
#23995,#23996,#23997,#23998,#23999,#24000,#24001,#24002,#24003,#24004,#24005,
#24006,#24007,#24008,#24009,#24010,#24011,#24012,#24013,#24014,#24015,#24016,
#24017,#24018,#24019,#24020,#24021,#24022,#24023,#24024,#24025,#24026,#24027,
#24028,#24029,#24030,#24031,#24032,#24033,#24034,#24035,#24036,#24037,#24038,
#24039,#24040,#24041,#24042,#24043,#24044,#24045,#24046,#24047,#24048,#24049,
#24050,#24051,#24052,#24053,#24054,#24055,#24056,#24057,#24058,#24059,#24060,
#24061,#24062,#24063,#24064,#24065,#24066,#24067,#24068,#24069,#24070,#24071,
#24072,#24073,#24074,#24075,#24076,#24077,#24078,#24079,#24080,#24081,#24082,
#24083,#24084,#24085,#24086,#24087,#24088,#24089,#24090,#24091,#24092,#24093,
#24094,#24095,#24096,#24097,#24098,#24099,#24100,#24101,#24102,#24103,#24104,
#24105,#24106,#24107,#24108,#24109,#24110,#24111,#24112,#24113,#24114,#24115,
#24116,#24117,#24118,#24119,#24120,#24121,#24122,#24123,#24124,#24125,#24126,
#24127,#24128,#24129,#24130,#24131,#24132,#24133,#24134,#24135,#24136,#24137,
#24138,#24139,#24140,#24141,#24142,#24143,#24144,#24145,#24146,#24147,#24148,
#24149,#24150,#24151,#24152),.UNSPECIFIED.,.F.,.F.,(4,2,2,2,2,2,2,2,2,2,
2,2,2,2,2,2,2,2,2,2,2,2,2,2,2,2,2,2,2,2,2,2,2,2,2,2,2,2,2,2,2,2,2,2,2,2,
2,2,2,2,2,2,2,2,2,2,2,2,2,2,2,2,2,2,2,2,2,2,2,2,2,2,2,2,2,2,2,2,2,2,2,2,
2,2,2,2,2,2,2,2,2,2,2,2,2,2,2,2,2,2,2,2,2,2,2,2,2,2,4),(-1.24281229412899,
-1.23823517134402,-1.21326017462496,-1.20489355448001,-1.20161975505772,
-1.19917814953849,-1.19800670320905,-1.19709060012867,-1.19600605128283,
-1.19404865521973,-1.18439141630898,-1.1604026271728,-1.14459122506566,
-1.1413445968791,-1.13947562613542,-1.13784301643643,-1.13581739756981,
-1.13268256535286,-1.11075412422281,-1.09502376403645,-1.08731420511488,
-1.08421321765552,-1.08187219128653,-1.08072043993349,-1.07989379286338,
-1.07883095317678,-1.07696947794716,-1.06894493296442,-1.06570174440512,
-1.05580034931728,-1.03732650538379,-1.02671796824432,-1.02381022009547,
-1.02201497047597,-1.02036840220475,-1.01825143614163,-1.01365851637043,
-0.988116047308891,-0.980509398572667,-0.967698761402144,-0.964877747211214,
-0.963636087701755,-0.962712599632508,-0.961672609248068,-0.959865471854731,
-0.952856005846949,-0.922129837401915,-0.91391540297594,-0.908197236100503,
-0.905864975208061,-0.904189237779933,-0.902662294837823,-0.90061010470269,
-0.896600383778468,-0.868905630287747,-0.8631419111951,-0.853652468501447,
-0.848360579796169,-0.846782285555594,-0.845792842470934,-0.844859427491579,
-0.84350187851855,-0.8409452467313,-0.816629540370137,-0.793814173284251,
-0.789989022974813,-0.787998307344609,-0.786367896299053,-0.784472366170217,
-0.781191641684948,-0.766110879440994,-0.742234622183565,-0.731906789792124,
-0.730087015630132,-0.728937518353579,-0.728022648202676,-0.726920394841888,
-0.724822741433705,-0.708844487496945,-0.683102623152255,-0.67467362275887,
-0.671889283589293,-0.670120906513703,-0.668465042154335,-0.666248908353811,
-0.661230650335449,-0.654325642225997,-0.633871752346058,-0.626179165452878,
-0.621584363691984,-0.614328384973159,-0.612522137548843,-0.611471950014313,
-0.610643292927963,-0.609473280095078,-0.607038889750075,-0.603777845190063,
-0.595460792427168,-0.570731071267607,-0.558184323631155,-0.555014160625655,
-0.553161801401082,-0.55169075703668,-0.549718453910335,-0.545983019762226,
-0.541265092616273,-0.530362481310411,-0.509637148706452,-0.500694290278421),
 .UNSPECIFIED.);
#238=B_SPLINE_CURVE_WITH_KNOTS('',3,(#24154,#24155,#24156,#24157,#24158,
#24159,#24160,#24161,#24162,#24163,#24164,#24165,#24166,#24167,#24168,#24169,
#24170,#24171,#24172,#24173,#24174,#24175,#24176,#24177,#24178,#24179,#24180,
#24181,#24182,#24183,#24184,#24185,#24186,#24187,#24188,#24189,#24190,#24191,
#24192,#24193,#24194,#24195,#24196,#24197,#24198,#24199,#24200,#24201,#24202,
#24203,#24204,#24205,#24206,#24207,#24208,#24209,#24210,#24211,#24212,#24213,
#24214,#24215,#24216,#24217,#24218,#24219,#24220,#24221,#24222,#24223,#24224,
#24225),.UNSPECIFIED.,.F.,.F.,(4,2,2,2,2,2,2,2,2,2,2,2,2,2,2,2,2,2,2,2,
2,2,2,2,2,2,2,2,2,2,2,2,2,2,2,4),(-0.242048471304312,-0.231554403723091,
-0.223053577267517,-0.212631651068731,-0.210808319157637,-0.209657860609199,
-0.208743118845369,-0.207642101892112,-0.205549745632317,-0.189851934316851,
-0.16484173116906,-0.155586910339118,-0.152709821721549,-0.15092152683397,
-0.149273339846562,-0.147106475332604,-0.142481241995114,-0.136206643895549,
-0.119012139413158,-0.0968518603501121,-0.0939519885653981,-0.0927866177273898,
-0.0918473914480129,-0.0908673859660855,-0.0894237017264087,-0.0851053334230332,
-0.0779574720188684,-0.0596249657259443,-0.0394613817161886,-0.0363332063582247,
-0.0343098187854399,-0.0326776805504764,-0.030807797978331,-0.0288547148409675,
-0.0258775913530729,-0.000340687906700261),.UNSPECIFIED.);
#239=B_SPLINE_CURVE_WITH_KNOTS('',3,(#24226,#24227,#24228,#24229,#24230,
#24231,#24232,#24233,#24234,#24235,#24236,#24237,#24238,#24239,#24240,#24241,
#24242,#24243,#24244,#24245,#24246,#24247,#24248,#24249,#24250,#24251,#24252,
#24253,#24254,#24255,#24256,#24257,#24258,#24259,#24260,#24261,#24262,#24263,
#24264,#24265,#24266,#24267,#24268,#24269,#24270,#24271,#24272,#24273,#24274,
#24275,#24276,#24277,#24278,#24279,#24280,#24281,#24282,#24283,#24284,#24285,
#24286,#24287,#24288,#24289,#24290,#24291,#24292,#24293,#24294,#24295,#24296,
#24297,#24298,#24299,#24300,#24301,#24302,#24303,#24304,#24305,#24306,#24307,
#24308,#24309,#24310,#24311,#24312,#24313,#24314,#24315,#24316,#24317,#24318,
#24319,#24320,#24321,#24322,#24323,#24324,#24325,#24326,#24327,#24328,#24329,
#24330,#24331,#24332,#24333,#24334,#24335,#24336,#24337,#24338,#24339,#24340,
#24341,#24342,#24343,#24344,#24345,#24346,#24347,#24348,#24349,#24350,#24351,
#24352,#24353,#24354,#24355,#24356,#24357,#24358,#24359,#24360,#24361,#24362,
#24363,#24364,#24365,#24366,#24367,#24368,#24369,#24370,#24371,#24372,#24373,
#24374,#24375,#24376,#24377,#24378,#24379,#24380,#24381,#24382,#24383),
 .UNSPECIFIED.,.F.,.F.,(4,2,2,2,2,2,2,2,2,2,2,2,2,2,2,2,2,2,2,2,2,2,2,2,
2,2,2,2,2,2,2,2,2,2,2,2,2,2,2,2,2,2,2,2,2,2,2,2,2,2,2,2,2,2,2,2,2,2,2,2,
2,2,2,2,2,2,2,2,2,2,2,2,2,2,2,2,2,2,4),(-1.48430386926941,-1.46653245415301,
-1.46301191802203,-1.46120515283548,-1.46005760821234,-1.45898269395285,
-1.45806588602968,-1.45688211279949,-1.45494716502168,-1.43810227494753,
-1.42412050259781,-1.40892041175522,-1.40379176762196,-1.40150491354494,
-1.3998375533479,-1.39830145062393,-1.39580812106899,-1.389499567781,-1.36287288999797,
-1.35051814156449,-1.34632668246337,-1.34340389296128,-1.34219418040405,
-1.34125847686484,-1.34037823588219,-1.33885441978669,-1.33640354760787,
-1.31523334121925,-1.29739251665676,-1.2909842242855,-1.28624381416137,
-1.28407724377567,-1.28242910837973,-1.28064070118657,-1.27776306416874,
-1.26850336685781,-1.24347938907165,-1.2277755788542,-1.22568290448192,
-1.22458181519565,-1.2236670691561,-1.22251668071253,-1.22069361090505,
-1.21027565538499,-1.20179862028053,-1.18738686595642,-1.17134688157405,
-1.16808991815495,-1.16621890295608,-1.16458679605956,-1.16256476834823,
-1.15944120328641,-1.13674977937359,-1.11936166223676,-1.11319450290552,
-1.10926827941543,-1.10785412865197,-1.10690022479071,-1.1060411299623,
-1.10485699149948,-1.10184581706413,-1.08306963647165,-1.06420424858992,
-1.05709344646599,-1.05196173420385,-1.0497261710511,-1.0480673441908,-1.04630655482708,
-1.043556703316,-1.03541377996334,-1.00616470818863,-0.997347043696302,
-0.992308073499113,-0.990756958282208,-0.989773540814691,-0.988836442150449,
-0.987679389918078,-0.984828314075721,-0.984009904944126),.UNSPECIFIED.);
#240=B_SPLINE_CURVE_WITH_KNOTS('',3,(#24389,#24390,#24391,#24392,#24393,
#24394,#24395,#24396,#24397,#24398,#24399,#24400,#24401,#24402,#24403,#24404,
#24405,#24406,#24407,#24408,#24409,#24410,#24411,#24412,#24413,#24414,#24415,
#24416,#24417,#24418,#24419,#24420,#24421,#24422,#24423,#24424,#24425,#24426,
#24427,#24428,#24429,#24430,#24431,#24432,#24433,#24434,#24435,#24436,#24437,
#24438,#24439,#24440,#24441,#24442,#24443,#24444,#24445,#24446,#24447,#24448,
#24449,#24450,#24451,#24452,#24453,#24454,#24455,#24456,#24457,#24458,#24459,
#24460,#24461,#24462,#24463,#24464,#24465,#24466,#24467,#24468,#24469,#24470,
#24471,#24472,#24473,#24474,#24475,#24476,#24477,#24478,#24479,#24480,#24481,
#24482,#24483,#24484,#24485,#24486,#24487,#24488,#24489,#24490,#24491,#24492,
#24493,#24494,#24495,#24496,#24497,#24498,#24499,#24500,#24501,#24502,#24503,
#24504,#24505,#24506,#24507,#24508,#24509,#24510,#24511,#24512,#24513,#24514,
#24515,#24516,#24517,#24518,#24519,#24520,#24521,#24522,#24523,#24524,#24525,
#24526,#24527,#24528,#24529,#24530,#24531,#24532,#24533,#24534,#24535,#24536,
#24537,#24538,#24539,#24540,#24541,#24542,#24543,#24544),.UNSPECIFIED.,
 .F.,.F.,(4,2,2,2,2,2,2,2,2,2,2,2,2,2,2,2,2,2,2,2,2,2,2,2,2,2,2,2,2,2,2,
2,2,2,2,2,2,2,2,2,2,2,2,2,2,2,2,2,2,2,2,2,2,2,2,2,2,2,2,2,2,2,2,2,2,2,2,
2,2,2,2,2,2,2,2,2,2,4),(-0.500918874538835,-0.493729283290626,-0.481227039374831,
-0.478096659133442,-0.476235156695093,-0.474617166932814,-0.472588241309173,
-0.468574202577156,-0.463403476454992,-0.450860905284672,-0.431807810733804,
-0.427786646560088,-0.420183640185763,-0.418351148640682,-0.41729488808885,
-0.416467182695655,-0.415305960627832,-0.41291704794769,-0.409734480839948,
-0.401718598209421,-0.378190358497151,-0.364163038685052,-0.360935707274224,
-0.359052161850098,-0.357420774093964,-0.355414543566555,-0.35151354127568,
-0.328585937674148,-0.304510491538616,-0.301652902497553,-0.300528471513784,
-0.299599538386361,-0.29860167729446,-0.296985630064722,-0.291321263688311,
-0.280790039047186,-0.256675361679246,-0.24637393203707,-0.243385967550815,
-0.241573128394394,-0.23993106781524,-0.237813195361913,-0.233339498974164,
-0.227395350281804,-0.211711913427668,-0.187188907166548,-0.184372544429671,
-0.183144933029173,-0.182220313064407,-0.181184136788051,-0.179394684184911,
-0.171600372616162,-0.139234087204213,-0.129060581538441,-0.126084741605259,
-0.124274614667218,-0.122664708414234,-0.120738536918804,-0.118540543195545,
-0.114967194231283,-0.107719961407809,-0.0881813356869555,-0.0702913549404585,
-0.0672782632698932,-0.0660936630632054,-0.0652343393737278,-0.0642802943988998,
-0.062866129214121,-0.0589410146506339,-0.0527774767385878,-0.0183603635020737,
-0.0110828695650004,-0.00844907915857034,-0.00688652083307198,-0.00531417154097046,
-0.00371122492596661,-0.00203843401347154,-0.000340248170157266),
 .UNSPECIFIED.);
#241=B_SPLINE_CURVE_WITH_KNOTS('',3,(#24545,#24546,#24547,#24548,#24549,
#24550,#24551,#24552,#24553,#24554,#24555,#24556,#24557,#24558,#24559,#24560,
#24561,#24562,#24563,#24564,#24565,#24566,#24567,#24568,#24569,#24570,#24571,
#24572,#24573,#24574,#24575,#24576,#24577,#24578,#24579,#24580,#24581,#24582,
#24583,#24584,#24585,#24586,#24587,#24588,#24589,#24590,#24591,#24592,#24593,
#24594,#24595,#24596,#24597,#24598,#24599,#24600,#24601,#24602,#24603,#24604,
#24605,#24606,#24607,#24608,#24609,#24610,#24611,#24612,#24613,#24614,#24615,
#24616,#24617,#24618,#24619,#24620,#24621,#24622,#24623,#24624),
 .UNSPECIFIED.,.F.,.F.,(4,2,2,2,2,2,2,2,2,2,2,2,2,2,2,2,2,2,2,2,2,2,2,2,
2,2,2,2,2,2,2,2,2,2,2,2,2,2,2,4),(-1.484428834093,-1.48054199923031,-1.44819876680698,
-1.43954244786739,-1.43456582256332,-1.433021565382,-1.4320396319046,-1.43110147473606,
-1.42994050820837,-1.42706690860662,-1.40446331814616,-1.3827964218617,
-1.37896070958198,-1.37665631910656,-1.37465654399446,-1.37462546049038,
-1.37459299209241,-1.37455895845735,-1.37298760352077,-1.37120341845313,
-1.36834614543548,-1.35928455012788,-1.33113078566982,-1.32234322774752,
-1.31896227105564,-1.31645911480328,-1.31527586076659,-1.31435886885517,
-1.31328303482637,-1.31136429422616,-1.3024234939432,-1.27852599892734,
-1.26749043433603,-1.26273424659767,-1.25897468290425,-1.2569973714755,
-1.25552581078917,-1.25367702645904,-1.25052352740852,-1.24281229412899),
 .UNSPECIFIED.);
#242=B_SPLINE_CURVE_WITH_KNOTS('',3,(#24625,#24626,#24627,#24628,#24629,
#24630,#24631,#24632,#24633,#24634,#24635,#24636,#24637,#24638,#24639,#24640,
#24641,#24642,#24643,#24644,#24645,#24646,#24647,#24648,#24649,#24650,#24651,
#24652,#24653,#24654,#24655,#24656,#24657,#24658,#24659,#24660,#24661,#24662,
#24663,#24664,#24665,#24666,#24667,#24668,#24669,#24670,#24671,#24672,#24673,
#24674,#24675,#24676,#24677,#24678,#24679,#24680,#24681,#24682,#24683,#24684,
#24685,#24686,#24687,#24688,#24689,#24690,#24691,#24692,#24693,#24694,#24695,
#24696,#24697,#24698,#24699,#24700,#24701,#24702,#24703,#24704,#24705,#24706,
#24707,#24708,#24709,#24710,#24711,#24712,#24713,#24714,#24715,#24716,#24717,
#24718,#24719,#24720,#24721,#24722,#24723,#24724,#24725,#24726,#24727,#24728,
#24729,#24730,#24731,#24732,#24733,#24734,#24735,#24736,#24737,#24738,#24739,
#24740,#24741,#24742,#24743,#24744,#24745,#24746,#24747,#24748,#24749,#24750,
#24751,#24752,#24753,#24754,#24755,#24756,#24757,#24758,#24759,#24760,#24761,
#24762,#24763,#24764,#24765,#24766,#24767,#24768,#24769,#24770,#24771,#24772,
#24773,#24774,#24775,#24776,#24777,#24778,#24779,#24780,#24781,#24782,#24783,
#24784,#24785,#24786,#24787,#24788,#24789,#24790,#24791,#24792,#24793,#24794,
#24795,#24796,#24797,#24798,#24799,#24800,#24801,#24802,#24803,#24804,#24805,
#24806,#24807,#24808,#24809,#24810,#24811,#24812,#24813,#24814,#24815,#24816,
#24817,#24818,#24819,#24820,#24821,#24822,#24823,#24824,#24825,#24826,#24827,
#24828,#24829,#24830,#24831,#24832,#24833,#24834),.UNSPECIFIED.,.F.,.F.,
(4,2,2,2,2,2,2,2,2,2,2,2,2,2,2,2,2,2,2,2,2,2,2,2,2,2,2,2,2,2,2,2,2,2,2,
2,2,2,2,2,2,2,2,2,2,2,2,2,2,2,2,2,2,2,2,2,2,2,2,2,2,2,2,2,2,2,2,2,2,2,2,
2,2,2,2,2,2,2,2,2,2,2,2,2,2,2,2,2,2,2,2,2,2,2,2,2,2,2,2,2,2,2,2,2,4),(-0.984009904944126,
-0.961823534427199,-0.945195306252899,-0.939041443571138,-0.934446193655206,
-0.932305920577051,-0.930661196563781,-0.928860089942887,-0.925925060339749,
-0.916138104967741,-0.91207595714914,-0.887983807976547,-0.87979473307276,
-0.876566997483682,-0.874152070093205,-0.872985846154686,-0.872157654540614,
-0.871104997304057,-0.869287951302992,-0.861891600062579,-0.828857887531441,
-0.822194217371007,-0.817309812771511,-0.815117350561738,-0.813465295773428,
-0.811687780770774,-0.80886067874769,-0.80006226638829,-0.774632035453004,
-0.759364241953133,-0.756898528797663,-0.755722523075203,-0.754806198822679,
-0.753725331435031,-0.751783946388736,-0.742429814717131,-0.728395940025744,
-0.7045998991639,-0.69994722095481,-0.697819598376388,-0.696171664681408,
-0.694381864280427,-0.691498409294805,-0.681164420729508,-0.66101064452863,
-0.643045424406669,-0.640020575434316,-0.638834112941866,-0.637974400631664,
-0.637021087375945,-0.635609991488778,-0.631706152056529,-0.625588603678782,
-0.608092311262583,-0.585454202895747,-0.582330758723305,-0.580308698757551,
-0.578676506552808,-0.576805328229851,-0.573547919673089,-0.557504716755464,
-0.543078998107933,-0.534593194621034,-0.524170828774063,-0.522347387900391,
-0.52119685886378,-0.520282056713186,-0.519180961569566,-0.517088456235864,
-0.50138952306028,-0.476374215858401,-0.467121382497707,-0.464244364526069,
-0.462456000152752,-0.460807673144654,-0.45864051313973,-0.453897457069288,
-0.447483899476263,-0.429619180084874,-0.408452204479977,-0.40549510076717,
-0.404325496014753,-0.403470035376363,-0.40251172713355,-0.401076501375177,
-0.396994837311345,-0.39048558233509,-0.359714952843162,-0.349966969742027,
-0.347036448951131,-0.345236468629042,-0.343591695099338,-0.34144981021662,
-0.336844991260212,-0.330673547526229,-0.313962880636645,-0.291059627270006,
-0.288203554379225,-0.287045692396799,-0.286108440409246,-0.285125466761232,
-0.283576124848773,-0.278552309547939,-0.269774735303037,-0.241902829928485),
 .UNSPECIFIED.);
#243=B_SPLINE_CURVE_WITH_KNOTS('',3,(#24839,#24840,#24841,#24842,#24843,
#24844,#24845,#24846,#24847,#24848,#24849,#24850,#24851,#24852,#24853,#24854,
#24855,#24856,#24857,#24858,#24859,#24860,#24861,#24862,#24863,#24864,#24865,
#24866,#24867,#24868,#24869,#24870,#24871,#24872,#24873,#24874,#24875,#24876,
#24877,#24878,#24879,#24880,#24881,#24882,#24883,#24884,#24885,#24886,#24887,
#24888,#24889,#24890,#24891,#24892,#24893,#24894,#24895,#24896,#24897,#24898,
#24899,#24900,#24901,#24902,#24903,#24904,#24905,#24906,#24907,#24908,#24909,
#24910,#24911,#24912,#24913,#24914,#24915,#24916,#24917,#24918,#24919,#24920,
#24921,#24922,#24923,#24924,#24925,#24926,#24927,#24928,#24929,#24930,#24931,
#24932,#24933,#24934,#24935,#24936,#24937,#24938,#24939,#24940,#24941,#24942,
#24943,#24944,#24945,#24946,#24947,#24948,#24949,#24950,#24951,#24952,#24953,
#24954,#24955,#24956,#24957,#24958,#24959,#24960,#24961,#24962,#24963,#24964,
#24965,#24966,#24967,#24968,#24969,#24970,#24971,#24972,#24973,#24974,#24975,
#24976,#24977,#24978,#24979,#24980,#24981,#24982,#24983,#24984,#24985,#24986,
#24987,#24988,#24989,#24990,#24991,#24992,#24993,#24994,#24995,#24996,#24997,
#24998,#24999,#25000,#25001,#25002,#25003,#25004,#25005,#25006,#25007,#25008,
#25009,#25010,#25011,#25012,#25013,#25014,#25015,#25016,#25017,#25018,#25019,
#25020,#25021,#25022,#25023,#25024,#25025,#25026,#25027,#25028,#25029,#25030,
#25031,#25032,#25033,#25034,#25035,#25036,#25037,#25038,#25039,#25040,#25041,
#25042,#25043,#25044,#25045,#25046,#25047,#25048,#25049,#25050,#25051,#25052,
#25053,#25054,#25055,#25056,#25057,#25058),.UNSPECIFIED.,.F.,.F.,(4,2,2,
2,2,2,2,2,2,2,2,2,2,2,2,2,2,2,2,2,2,2,2,2,2,2,2,2,2,2,2,2,2,2,2,2,2,2,2,
2,2,2,2,2,2,2,2,2,2,2,2,2,2,2,2,2,2,2,2,2,2,2,2,2,2,2,2,2,2,2,2,2,2,2,2,
2,2,2,2,2,2,2,2,2,2,2,2,2,2,2,2,2,2,2,2,2,2,2,2,2,2,2,2,2,2,2,2,2,2,4),
(-1.24300538673529,-1.2401076602996,-1.23867315968935,-1.23771505767543,
-1.23685955737713,-1.23568962472891,-1.2327301582961,-1.21164802544438,
-1.19374966498115,-1.18732972550532,-1.18258269622164,-1.18041489176712,
-1.17876653800613,-1.17697859281537,-1.17410324096957,-1.16486562072408,
-1.13982471522782,-1.12411473949377,-1.12202192607441,-1.12092078744097,
-1.1200060120584,-1.11885559365772,-1.11703248430546,-1.10661411685994,
-1.09814086903657,-1.08373365899801,-1.06768956408412,-1.06443236880306,
-1.06256126807125,-1.06092911219803,-1.05890705464857,-1.05578349675363,
-1.03309324686783,-1.01570512165146,-1.00953932273506,-1.00561371817511,
-1.00419962769855,-1.00324571576042,-1.00238657163031,-1.00120230670449,
-0.998190493157122,-0.980337453497084,-0.963307904897578,-0.950166593197001,
-0.947069094429297,-0.945232612494161,-0.943595782504044,-0.941521204963318,
-0.93727350782546,-0.907678649802125,-0.904497804750764,-0.894309621728063,
-0.888765802241242,-0.88716180508812,-0.886166715910977,-0.885236563944614,
-0.884106736499347,-0.881214145464196,-0.857669174478239,-0.841401721951798,
-0.835326901869917,-0.830777208047939,-0.828645339272115,-0.827001691523599,
-0.825196388889853,-0.822242235297532,-0.812287196951743,-0.781724872283551,
-0.775226734626685,-0.771150258077749,-0.769715565673442,-0.768757261567959,
-0.767901523645287,-0.766731194434354,-0.763770341694089,-0.742696147585277,
-0.718172832549207,-0.713540651441771,-0.711416562028089,-0.70976896300983,
-0.707977117835005,-0.705085003227308,-0.694656226705977,-0.674156662841869,
-0.666059795982463,-0.662822546383895,-0.654774240561229,-0.652911108557263,
-0.651847885413859,-0.651021272715207,-0.649870012407224,-0.647531515250833,
-0.629198984754756,-0.600476933631467,-0.596129941273214,-0.59403620395498,
-0.592397186911814,-0.590571632870533,-0.587524702010141,-0.575135247469739,
-0.544630197788277,-0.537381444353269,-0.535575649839366,-0.534525498983972,
-0.533696726951843,-0.532526364007551,-0.530090548346005,-0.526827138453678,
-0.518501390079531,-0.500918874538835),.UNSPECIFIED.);
#244=B_SPLINE_CURVE_WITH_KNOTS('',3,(#25060,#25061,#25062,#25063,#25064,
#25065,#25066,#25067,#25068,#25069,#25070,#25071,#25072,#25073,#25074,#25075,
#25076,#25077,#25078,#25079,#25080,#25081,#25082,#25083,#25084,#25085,#25086,
#25087,#25088,#25089,#25090,#25091,#25092,#25093,#25094,#25095,#25096,#25097,
#25098,#25099,#25100,#25101,#25102,#25103,#25104,#25105,#25106,#25107,#25108,
#25109,#25110,#25111,#25112,#25113,#25114,#25115,#25116,#25117,#25118,#25119,
#25120,#25121,#25122,#25123,#25124,#25125,#25126,#25127,#25128,#25129,#25130,
#25131,#25132,#25133,#25134,#25135,#25136,#25137,#25138,#25139,#25140,#25141,
#25142,#25143,#25144,#25145,#25146,#25147,#25148,#25149,#25150,#25151,#25152,
#25153,#25154,#25155,#25156,#25157,#25158,#25159,#25160,#25161,#25162,#25163),
 .UNSPECIFIED.,.F.,.F.,(4,2,2,2,2,2,2,2,2,2,2,2,2,2,2,2,2,2,2,2,2,2,2,2,
2,2,2,2,2,2,2,2,2,2,2,2,2,2,2,2,2,2,2,2,2,2,2,2,2,2,2,4),(-0.241902829928485,
-0.241235095552837,-0.232498724410631,-0.229678875365911,-0.227903015268497,
-0.226250506802044,-0.224054461234132,-0.219149343198562,-0.212447672973761,
-0.193108617620372,-0.174036634756401,-0.171029143259472,-0.169845638469247,
-0.168986729277969,-0.168032690142907,-0.166617766914246,-0.162685611602245,
-0.156506198619109,-0.139146666803432,-0.116485689341663,-0.11335724721356,
-0.111333768510963,-0.1097420786436,-0.109666710484884,-0.10962984118605,
-0.10956028055288,-0.109498224048938,-0.109442381974887,-0.109391752542218,
-0.109345544019743,-0.109303121300336,-0.109263968090822,-0.109227659854679,
-0.109193843831824,-0.109162224164724,-0.109132550654296,-0.109104610058547,
-0.109078219341809,-0.107077758985253,-0.104796295575755,-0.101016965016604,
-0.0804882390455822,-0.0564855802506454,-0.0536229642185044,-0.0524979140069384,
-0.0515690019114021,-0.0505718399758018,-0.0489581966699216,-0.0433156083799494,
-0.0328459798865186,-0.0193890757200365,-0.000340612923464106),
 .UNSPECIFIED.);
#245=B_SPLINE_CURVE_WITH_KNOTS('',3,(#25164,#25165,#25166,#25167,#25168,
#25169,#25170,#25171,#25172,#25173,#25174,#25175,#25176,#25177,#25178,#25179,
#25180,#25181,#25182,#25183,#25184,#25185,#25186,#25187,#25188,#25189,#25190,
#25191,#25192,#25193,#25194,#25195,#25196,#25197,#25198,#25199,#25200,#25201,
#25202,#25203,#25204,#25205,#25206,#25207,#25208,#25209,#25210,#25211,#25212,
#25213,#25214,#25215,#25216,#25217,#25218,#25219,#25220,#25221,#25222,#25223,
#25224,#25225,#25226,#25227,#25228,#25229,#25230,#25231,#25232,#25233,#25234,
#25235,#25236,#25237,#25238,#25239,#25240,#25241,#25242,#25243,#25244,#25245,
#25246,#25247,#25248,#25249,#25250,#25251,#25252,#25253,#25254,#25255,#25256,
#25257,#25258,#25259,#25260,#25261,#25262,#25263,#25264,#25265,#25266,#25267,
#25268,#25269,#25270,#25271,#25272,#25273,#25274,#25275,#25276,#25277,#25278,
#25279,#25280,#25281,#25282,#25283,#25284,#25285,#25286,#25287,#25288,#25289,
#25290,#25291,#25292,#25293,#25294,#25295,#25296,#25297,#25298,#25299,#25300,
#25301,#25302,#25303,#25304,#25305,#25306,#25307,#25308,#25309,#25310,#25311,
#25312,#25313,#25314,#25315,#25316,#25317),.UNSPECIFIED.,.F.,.F.,(4,2,2,
2,2,2,2,2,2,2,2,2,2,2,2,2,2,2,2,2,2,2,2,2,2,2,2,2,2,2,2,2,2,2,2,2,2,2,2,
2,2,2,2,2,2,2,2,2,2,2,2,2,2,2,2,2,2,2,2,2,2,2,2,2,2,2,2,2,2,2,2,2,2,2,2,
2,4),(-1.48429374019444,-1.48208298361065,-1.48001002368649,-1.47838838880993,
-1.47683260671731,-1.47508675568846,-1.47240399049729,-1.46475589808267,
-1.43473308594258,-1.42602539635362,-1.42102958109654,-1.4194836706342,
-1.41850168443352,-1.41756434191149,-1.41640529833117,-1.41354098980554,
-1.39083238707803,-1.36928321980456,-1.36544568595439,-1.36314092235335,
-1.3610670934118,-1.35945246340073,-1.35766389759325,-1.35478391861388,
-1.34549655724287,-1.31421128218915,-1.30766835496553,-1.30357236516067,
-1.30213549942183,-1.30117705255872,-1.30032220070988,-1.29915435582538,
-1.29620696254842,-1.27485328121104,-1.25714433572781,-1.25076353626861,
-1.24603895611784,-1.24387551427642,-1.24222809398535,-1.24043883945829,
-1.23755623786655,-1.22824582883302,-1.20327245215956,-1.1875894250323,
-1.18549749419664,-1.18439669399194,-1.1834821290127,-1.18233189379625,
-1.18050893065373,-1.17008659443793,-1.16159109665915,-1.14712713329275,
-1.13116630040875,-1.12791351583137,-1.12604363844312,-1.12441178456757,
-1.12238911242253,-1.11926271092811,-1.09671372620601,-1.07964247930974,
-1.07319747557486,-1.06914528578361,-1.06771419487868,-1.06675690837535,
-1.06590100850812,-1.0647291199385,-1.06178171411255,-1.04061416071021,
-1.022775200704,-1.01636762878247,-1.01162776298925,-1.00946145181498,-1.00781351781457,
-1.00602533325033,-1.00314806349783,-0.993889634336018,-0.983954477832344),
 .UNSPECIFIED.);
#246=B_SPLINE_CURVE_WITH_KNOTS('',3,(#25323,#25324,#25325,#25326,#25327,
#25328,#25329,#25330,#25331,#25332,#25333,#25334,#25335,#25336,#25337,#25338,
#25339,#25340,#25341,#25342,#25343,#25344,#25345,#25346,#25347,#25348,#25349,
#25350,#25351,#25352,#25353,#25354,#25355,#25356,#25357,#25358,#25359,#25360,
#25361,#25362,#25363,#25364,#25365,#25366,#25367,#25368,#25369,#25370,#25371,
#25372,#25373,#25374,#25375,#25376,#25377,#25378,#25379,#25380,#25381,#25382,
#25383,#25384,#25385,#25386,#25387,#25388,#25389,#25390,#25391,#25392,#25393,
#25394,#25395,#25396,#25397,#25398,#25399,#25400,#25401,#25402,#25403,#25404,
#25405,#25406,#25407,#25408,#25409,#25410,#25411,#25412,#25413,#25414,#25415,
#25416,#25417,#25418,#25419,#25420,#25421,#25422,#25423,#25424,#25425,#25426,
#25427,#25428,#25429,#25430,#25431,#25432,#25433,#25434,#25435,#25436,#25437,
#25438,#25439,#25440,#25441,#25442,#25443,#25444,#25445,#25446,#25447,#25448,
#25449,#25450,#25451,#25452,#25453,#25454,#25455,#25456,#25457,#25458,#25459,
#25460,#25461,#25462,#25463,#25464,#25465,#25466),.UNSPECIFIED.,.F.,.F.,
(4,2,2,2,2,2,2,2,2,2,2,2,2,2,2,2,2,2,2,2,2,2,2,2,2,2,2,2,2,2,2,2,2,2,2,
2,2,2,2,2,2,2,2,2,2,2,2,2,2,2,2,2,2,2,2,2,2,2,2,2,2,2,2,2,2,2,2,2,2,2,2,
4),(-0.500810674765781,-0.493763997975324,-0.479343838874954,-0.470862672363058,
-0.46044030020236,-0.458616925055466,-0.457466435887697,-0.456551662356445,
-0.455450590638109,-0.453358092466655,-0.437654725138245,-0.412625980248117,
-0.403393575844477,-0.400518790032286,-0.398730949720771,-0.397082524951323,
-0.394914382057417,-0.390165635960305,-0.38374194195318,-0.365826223518783,
-0.344741174014523,-0.341781252562763,-0.340610762999099,-0.339755101282576,
-0.338797108669497,-0.33736328374844,-0.333291885928938,-0.326805381007299,
-0.296372437889619,-0.28632500980634,-0.28336056594681,-0.28155321931724,
-0.279910459444584,-0.277783648842673,-0.27325999921489,-0.267229219376008,
-0.251158195752625,-0.227285441490762,-0.224413386411133,-0.223286872301924,
-0.222357626374446,-0.22136120073813,-0.219750780971,-0.214140555211819,
-0.203763530308994,-0.180283500567982,-0.169277718806919,-0.166221296568094,
-0.164393867620123,-0.162755553573591,-0.160666000833089,-0.156339841161414,
-0.139563400149093,-0.112879349242939,-0.107947730715232,-0.106352596766125,
-0.105359514347856,-0.104436295556282,-0.103187085909334,-0.101715303326176,
-0.0990955069060905,-0.093086120761574,-0.0684081952874672,-0.0525792148884451,
-0.0492653612654853,-0.0473624791550844,-0.0457482525158989,-0.0437738540592276,
-0.0400276938112811,-0.0352924223120453,-0.0243287202206848,-0.000340767018293399),
 .UNSPECIFIED.);
#247=B_SPLINE_CURVE_WITH_KNOTS('',3,(#25467,#25468,#25469,#25470,#25471,
#25472,#25473,#25474,#25475,#25476,#25477,#25478,#25479,#25480,#25481,#25482,
#25483,#25484,#25485,#25486,#25487,#25488,#25489,#25490,#25491,#25492,#25493,
#25494,#25495,#25496,#25497,#25498,#25499,#25500,#25501,#25502,#25503,#25504,
#25505,#25506,#25507,#25508,#25509,#25510,#25511,#25512,#25513,#25514,#25515,
#25516,#25517,#25518,#25519,#25520,#25521,#25522,#25523,#25524,#25525,#25526,
#25527,#25528,#25529,#25530,#25531,#25532,#25533,#25534,#25535,#25536,#25537,
#25538,#25539,#25540,#25541,#25542,#25543,#25544,#25545,#25546,#25547,#25548,
#25549,#25550,#25551,#25552,#25553,#25554,#25555,#25556,#25557,#25558,#25559,
#25560,#25561,#25562,#25563,#25564,#25565,#25566,#25567,#25568,#25569,#25570,
#25571,#25572,#25573,#25574,#25575,#25576,#25577,#25578,#25579,#25580,#25581,
#25582,#25583,#25584,#25585,#25586,#25587,#25588,#25589,#25590,#25591,#25592,
#25593,#25594,#25595,#25596,#25597,#25598,#25599,#25600,#25601,#25602,#25603,
#25604,#25605,#25606,#25607,#25608,#25609,#25610,#25611,#25612,#25613,#25614,
#25615,#25616,#25617,#25618,#25619,#25620,#25621,#25622,#25623,#25624,#25625,
#25626,#25627,#25628,#25629,#25630,#25631,#25632,#25633,#25634,#25635,#25636,
#25637,#25638,#25639,#25640,#25641,#25642,#25643,#25644,#25645,#25646,#25647,
#25648,#25649,#25650,#25651,#25652,#25653,#25654),.UNSPECIFIED.,.F.,.F.,
(4,2,2,2,2,2,2,2,2,2,2,2,2,2,2,2,2,2,2,2,2,2,2,2,2,2,2,2,2,2,2,2,2,2,2,
2,2,2,2,2,2,2,2,2,2,2,2,2,2,2,2,2,2,2,2,2,2,2,2,2,2,2,2,2,2,2,2,2,2,2,2,
2,2,2,2,2,2,2,2,2,2,2,2,2,2,2,2,2,2,2,2,2,2,4),(-1.48452413958049,-1.4784429304074,
-1.47512352499763,-1.47386473256755,-1.47293655958983,-1.472065482934,-1.47106651165108,
-1.46944417051658,-1.46428483722046,-1.45654241215069,-1.42936559743042,
-1.41871316119289,-1.41580239765065,-1.41400693704685,-1.41236126653133,
-1.41024697066382,-1.40583133784541,-1.37839802722197,-1.37242614775626,
-1.36926311670616,-1.36189881745768,-1.35889177242019,-1.35662511794588,
-1.35550052783905,-1.3554962227811,-1.35549187782454,-1.35548749258201,
-1.35548306638497,-1.35547859880842,-1.3554740893391,-1.35546953748773,
-1.35546494273987,-1.35546030464082,-1.3554556226107,-1.35545089611522,
-1.35544612456033,-1.35544130745021,-1.35543644423668,-1.35543153422422,
-1.35542657678914,-1.35542157148871,-1.35541651780225,-1.3554114149066,
-1.35540626230105,-1.35540105939099,-1.35539580552704,-1.35539049999029,
-1.35538514219486,-1.35537973157735,-1.35537426737185,-1.35536874884142,
-1.35536317543888,-1.35535754641141,-1.35535186095732,-1.35534611835286,
-1.35534115712002,-1.35533596964344,-1.35533054543398,-1.35532487328584,
-1.35531894164037,-1.35531273827813,-1.35530625042951,-1.35529946469499,
-1.35529236709083,-1.35528494287048,-1.35527717642616,-1.35526905161778,
-1.35526055144018,-1.35525165799427,-1.3552423525241,-1.35523261549278,
-1.35522242639285,-1.35521176363457,-1.3552006046248,-1.35518953070745,
-1.35517596990946,-1.35515936733245,-1.3551390467402,-1.35509835217385,
-1.35416888884173,-1.35304120289169,-1.35016118296104,-1.32671771010661,
-1.3103745565863,-1.30428365799597,-1.29972493834902,-1.29759171330962,
-1.29594822591923,-1.2941443039396,-1.29119516593943,-1.28127912217326,
-1.25068358274672,-1.24418434366141,-1.24300538673529),.UNSPECIFIED.);
#248=B_SPLINE_CURVE_WITH_KNOTS('',3,(#25655,#25656,#25657,#25658,#25659,
#25660,#25661,#25662,#25663,#25664,#25665,#25666,#25667,#25668,#25669,#25670,
#25671,#25672,#25673,#25674,#25675,#25676,#25677,#25678,#25679,#25680,#25681,
#25682,#25683,#25684,#25685,#25686,#25687,#25688,#25689,#25690,#25691,#25692,
#25693,#25694,#25695,#25696,#25697,#25698,#25699,#25700,#25701,#25702,#25703,
#25704,#25705,#25706,#25707,#25708,#25709,#25710,#25711,#25712,#25713,#25714,
#25715,#25716,#25717,#25718,#25719,#25720,#25721,#25722,#25723,#25724,#25725,
#25726,#25727,#25728,#25729,#25730,#25731,#25732,#25733,#25734,#25735,#25736,
#25737,#25738,#25739,#25740,#25741,#25742,#25743,#25744,#25745,#25746,#25747,
#25748,#25749,#25750,#25751,#25752,#25753,#25754,#25755,#25756,#25757,#25758,
#25759,#25760,#25761,#25762,#25763,#25764,#25765,#25766,#25767,#25768,#25769,
#25770,#25771,#25772,#25773,#25774,#25775,#25776,#25777,#25778,#25779,#25780,
#25781,#25782,#25783,#25784,#25785,#25786,#25787,#25788,#25789,#25790,#25791,
#25792,#25793,#25794,#25795,#25796,#25797,#25798,#25799,#25800,#25801,#25802,
#25803,#25804,#25805,#25806,#25807,#25808,#25809,#25810,#25811,#25812,#25813,
#25814,#25815,#25816,#25817,#25818,#25819,#25820,#25821,#25822,#25823,#25824,
#25825,#25826,#25827,#25828,#25829,#25830,#25831,#25832,#25833,#25834,#25835,
#25836,#25837,#25838,#25839,#25840,#25841,#25842,#25843,#25844,#25845,#25846,
#25847,#25848,#25849,#25850,#25851,#25852,#25853,#25854,#25855,#25856,#25857,
#25858,#25859,#25860,#25861,#25862,#25863,#25864,#25865,#25866,#25867,#25868,
#25869,#25870,#25871,#25872),.UNSPECIFIED.,.F.,.F.,(4,2,2,2,2,2,2,2,2,2,
2,2,2,2,2,2,2,2,2,2,2,2,2,2,2,2,2,2,2,2,2,2,2,2,2,2,2,2,2,2,2,2,2,2,2,2,
2,2,2,2,2,2,2,2,2,2,2,2,2,2,2,2,2,2,2,2,2,2,2,2,2,2,2,2,2,2,2,2,2,2,2,2,
2,2,2,2,2,2,2,2,2,2,2,2,2,2,2,2,2,2,2,2,2,2,2,2,2,2,4),(-0.983954477832344,
-0.968868638508017,-0.953166724759176,-0.951074306613063,-0.949973352227744,
-0.9490587183943,-0.947908471159131,-0.946085625100627,-0.935668945765655,
-0.927192952418088,-0.912782957367132,-0.896744966698653,-0.893488404504935,
-0.891617619380803,-0.889985712932694,-0.887963933233468,-0.884840750664748,
-0.862147866182155,-0.84475358069355,-0.838595020900477,-0.834672877626706,
-0.833259396390993,-0.832305711720418,-0.831446632176123,-0.830262283477115,
-0.827249331906869,-0.809126776339629,-0.789105104974024,-0.77880841300617,
-0.775928644710211,-0.774139827322274,-0.772491923622991,-0.770363109984292,
-0.76570277250765,-0.742272925841974,-0.720060305264201,-0.717159747474094,
-0.715994277868525,-0.715055042395106,-0.714075114170517,-0.712539453835846,
-0.707637798195469,-0.699173761350993,-0.673644462929149,-0.662005878491625,
-0.658897513439,-0.657058832256574,-0.655586296554883,-0.653595917379173,
-0.649771107742804,-0.624664531686292,-0.602847498623458,-0.599923513817372,
-0.598754034219578,-0.597898645370193,-0.596940393384362,-0.595505210046815,
-0.591423382144515,-0.584913573523478,-0.554129466025904,-0.544396415059281,
-0.541467651588219,-0.539668138414914,-0.538023389948223,-0.535880960189099,
-0.531272674746425,-0.525095062817244,-0.508354966292686,-0.485499830618691,
-0.482641648942825,-0.481483470251986,-0.480546180320971,-0.479563436227032,
-0.478014927172715,-0.472998013858148,-0.464238030225078,-0.435992997289897,
-0.427000993123812,-0.424151303747702,-0.422369041321594,-0.420718985637325,
-0.418538696411346,-0.413721658821508,-0.407176917836962,-0.37572818820882,
-0.366709973772506,-0.364787014616994,-0.36371034223593,-0.3627936263392,
-0.361612027954384,-0.359116905559313,-0.355750165659295,-0.347018754400621,
-0.319215201911636,-0.309821128283198,-0.306928982634031,-0.305137385784263,
-0.303490193216075,-0.301330529042793,-0.296628438329255,-0.290286876090216,
-0.272772109346323,-0.251090592894792,-0.24816705740505,-0.246997640327601,
-0.246142255360121,-0.245183956516744,-0.243748614346413,-0.241908569806093),
 .UNSPECIFIED.);
#249=B_SPLINE_CURVE_WITH_KNOTS('',3,(#25877,#25878,#25879,#25880,#25881,
#25882,#25883,#25884,#25885,#25886,#25887,#25888,#25889,#25890,#25891,#25892,
#25893,#25894,#25895,#25896,#25897,#25898,#25899,#25900,#25901,#25902,#25903,
#25904,#25905,#25906,#25907,#25908,#25909,#25910,#25911,#25912,#25913,#25914,
#25915,#25916,#25917,#25918,#25919,#25920,#25921,#25922,#25923,#25924,#25925,
#25926,#25927,#25928,#25929,#25930,#25931,#25932,#25933,#25934,#25935,#25936,
#25937,#25938,#25939,#25940,#25941,#25942,#25943,#25944,#25945,#25946,#25947,
#25948,#25949,#25950,#25951,#25952,#25953,#25954,#25955,#25956,#25957,#25958,
#25959,#25960,#25961,#25962,#25963,#25964,#25965,#25966,#25967,#25968,#25969,
#25970,#25971,#25972,#25973,#25974,#25975,#25976,#25977,#25978,#25979,#25980,
#25981,#25982,#25983,#25984,#25985,#25986,#25987,#25988,#25989,#25990,#25991,
#25992,#25993,#25994,#25995,#25996,#25997,#25998,#25999,#26000,#26001,#26002,
#26003,#26004,#26005,#26006,#26007,#26008,#26009,#26010,#26011,#26012,#26013,
#26014,#26015,#26016,#26017,#26018,#26019,#26020,#26021,#26022,#26023,#26024,
#26025,#26026,#26027,#26028,#26029,#26030,#26031,#26032,#26033,#26034,#26035,
#26036,#26037,#26038,#26039,#26040,#26041,#26042,#26043,#26044,#26045,#26046,
#26047,#26048,#26049,#26050,#26051,#26052,#26053,#26054,#26055,#26056,#26057,
#26058,#26059,#26060,#26061,#26062,#26063,#26064,#26065,#26066,#26067,#26068,
#26069,#26070,#26071,#26072,#26073,#26074,#26075,#26076,#26077,#26078,#26079,
#26080,#26081,#26082,#26083,#26084,#26085,#26086,#26087,#26088,#26089,#26090,
#26091,#26092,#26093,#26094,#26095,#26096),.UNSPECIFIED.,.F.,.F.,(4,2,2,
2,2,2,2,2,2,2,2,2,2,2,2,2,2,2,2,2,2,2,2,2,2,2,2,2,2,2,2,2,2,2,2,2,2,2,2,
2,2,2,2,2,2,2,2,2,2,2,2,2,2,2,2,2,2,2,2,2,2,2,2,2,2,2,2,2,2,2,2,2,2,2,2,
2,2,2,2,2,2,2,2,2,2,2,2,2,2,2,2,2,2,2,2,2,2,2,2,2,2,2,2,2,2,2,2,2,2,4),
(-1.24277962970854,-1.23412966373543,-1.22741005871783,-1.22249463988393,
-1.22029694619587,-1.21864434600835,-1.21708539526387,-1.21446904165843,
-1.20733392187946,-1.17702478227368,-1.16805907342439,-1.16296381083007,
-1.16140672726362,-1.16042211146713,-1.15948607423148,-1.15833263541782,
-1.15550168011246,-1.13203242805169,-1.11572196681001,-1.10963814963226,
-1.105083467593,-1.10295092969087,-1.10130746684272,-1.09950306753541,-1.09655199534884,
-1.08662009767472,-1.06218433081072,-1.05156119895492,-1.04586622071375,
-1.04424751512979,-1.04324927653661,-1.04232100142987,-1.04119842094369,
-1.03835110454978,-1.01419358187509,-0.998316397697683,-0.99232906098506,
-0.987830186697089,-0.985707990865551,-0.984065803704339,-0.982256076084012,
-0.97928077859667,-0.969108557526195,-0.942126827523083,-0.933463181284425,
-0.928483897929747,-0.926939460140422,-0.925957561489534,-0.925019566806886,
-0.92385893726383,-0.920986845991631,-0.898370413946775,-0.881493997925063,
-0.875286990624912,-0.870661321910824,-0.868515555929468,-0.866870202539996,
-0.865071960955131,-0.862149640011554,-0.852478469822047,-0.827812479964596,
-0.812247343682553,-0.8101571160069,-0.809056484770628,-0.808141636065454,
-0.806990502179923,-0.805165120257801,-0.794691935011586,-0.767279905622326,
-0.755348955916304,-0.752335519454585,-0.750517393691155,-0.748877024456409,
-0.74677039987178,-0.742354853180554,-0.724861715068614,-0.706506740457486,
-0.701560154790389,-0.694522194070815,-0.692712817320951,-0.691672440540991,
-0.690749232647188,-0.68950881276234,-0.686694124094588,-0.673941764204985,
-0.667390994497136,-0.640653917426471,-0.636129384357236,-0.634025143437769,
-0.632380586052915,-0.630579522932804,-0.627644243225624,-0.616707739600309,
-0.597181227651071,-0.579283183877282,-0.576270569478968,-0.575086175082451,
-0.574227006930266,-0.573273142164785,-0.571859256917569,-0.567935001968803,
-0.561772895381529,-0.544395779055861,-0.521716350416832,-0.518593117598922,
-0.516571157791766,-0.514939020119211,-0.513067873366136,-0.5098104327551,
-0.500810674765781),.UNSPECIFIED.);
#250=B_SPLINE_CURVE_WITH_KNOTS('',3,(#26098,#26099,#26100,#26101,#26102,
#26103,#26104,#26105,#26106,#26107,#26108,#26109,#26110,#26111,#26112,#26113,
#26114,#26115,#26116,#26117,#26118,#26119,#26120,#26121,#26122,#26123,#26124,
#26125,#26126,#26127,#26128,#26129,#26130,#26131,#26132,#26133,#26134,#26135,
#26136,#26137,#26138,#26139,#26140,#26141,#26142,#26143,#26144,#26145,#26146,
#26147,#26148,#26149,#26150,#26151,#26152,#26153,#26154,#26155,#26156,#26157,
#26158,#26159,#26160,#26161,#26162,#26163,#26164,#26165,#26166,#26167,#26168,
#26169,#26170,#26171,#26172,#26173,#26174,#26175),.UNSPECIFIED.,.F.,.F.,
(4,2,2,2,2,2,2,2,2,2,2,2,2,2,2,2,2,2,2,2,2,2,2,2,2,2,2,2,2,2,2,2,2,2,2,
2,2,2,4),(-0.241908569806093,-0.239665731678708,-0.233153621010589,-0.202335542846139,
-0.192632530864902,-0.189706977527231,-0.187908141035259,-0.186263159733702,
-0.184119201847845,-0.179502753495191,-0.173310959974035,-0.156505251655551,
-0.133750872788444,-0.130886135550159,-0.129726810989271,-0.128789205314897,
-0.127826604430165,-0.126336873585595,-0.124561298104256,-0.121127754815419,
-0.112129159235787,-0.0817443573993051,-0.0747175042380305,-0.0721163544391079,
-0.0705602358057474,-0.0689060117117186,-0.0666982153744462,-0.061725774537956,
-0.054903011115217,-0.025924018582589,-0.0183732371213993,-0.0141208835930925,
-0.0126150873274648,-0.0117383796533788,-0.0108668402608708,-0.00993909372422445,
-0.00868160291576745,-0.00563143718800878,-0.000340074931059168),
 .UNSPECIFIED.);
#251=B_SPLINE_CURVE_WITH_KNOTS('',3,(#26176,#26177,#26178,#26179,#26180,
#26181,#26182,#26183,#26184,#26185,#26186,#26187,#26188,#26189,#26190,#26191,
#26192,#26193,#26194,#26195,#26196,#26197,#26198,#26199,#26200,#26201,#26202,
#26203,#26204,#26205,#26206,#26207,#26208,#26209,#26210,#26211,#26212,#26213,
#26214,#26215,#26216,#26217,#26218,#26219,#26220,#26221,#26222,#26223,#26224,
#26225,#26226,#26227,#26228,#26229,#26230,#26231,#26232,#26233,#26234,#26235,
#26236,#26237,#26238,#26239,#26240,#26241,#26242,#26243,#26244,#26245,#26246,
#26247,#26248,#26249,#26250,#26251,#26252,#26253,#26254,#26255,#26256,#26257,
#26258,#26259,#26260,#26261,#26262,#26263,#26264,#26265,#26266,#26267,#26268,
#26269,#26270,#26271,#26272,#26273,#26274,#26275,#26276,#26277,#26278,#26279,
#26280,#26281,#26282,#26283,#26284,#26285,#26286,#26287,#26288,#26289,#26290,
#26291,#26292,#26293,#26294,#26295,#26296,#26297,#26298,#26299,#26300,#26301,
#26302,#26303,#26304,#26305,#26306,#26307,#26308,#26309,#26310,#26311,#26312,
#26313,#26314,#26315,#26316,#26317,#26318,#26319,#26320,#26321),
 .UNSPECIFIED.,.F.,.F.,(4,2,2,2,2,2,2,2,2,2,2,2,2,2,2,2,2,2,2,2,2,2,2,2,
2,2,2,2,2,2,2,2,2,2,2,2,2,2,2,2,2,2,2,2,2,2,2,2,2,2,2,2,2,2,2,2,2,2,2,2,
2,2,2,2,2,2,2,2,2,2,2,2,4),(-1.48451778638364,-1.46066201472305,-1.44895628021111,
-1.44401265830151,-1.4401374685125,-1.43813699952084,-1.43650661364363,
-1.43462010883433,-1.43137749338801,-1.41705735181162,-1.3922953247286,
-1.38529004156106,-1.38238243621184,-1.38080094696952,-1.37947675470059,
-1.37853757846013,-1.37768257102024,-1.37651429016597,-1.37356487970255,
-1.35221184560742,-1.33450158186885,-1.32812028024024,-1.32339532208566,
-1.32123170151447,-1.31958414283739,-1.31779473577959,-1.31491188349838,
-1.30560061704466,-1.28062519729804,-1.26494087202525,-1.26284876524312,
-1.26174787231249,-1.26083323021122,-1.25968289789646,-1.2578597806812,
-1.24743655671786,-1.23894033381647,-1.2244751106091,-1.2085129859683,-1.20525992963476,
-1.20338989512212,-1.20175790359319,-1.19973506014053,-1.19660839254029,
-1.17405755413047,-1.15698487328093,-1.15053929559783,-1.14648675040522,
-1.14505553698962,-1.14409816938358,-1.14324219765871,-1.14207021152182,
-1.13912255359797,-1.11795321845521,-1.10011275218442,-1.09370463955401,
-1.08896437385642,-1.08679787997681,-1.0851498070183,-1.08336147169593,
-1.0804839594233,-1.07122475044398,-1.04620164413103,-1.03049840612559,
-1.02840581154371,-1.02730476432478,-1.02639005336872,-1.02523970914546,
-1.02341670938952,-1.01299915182339,-1.00452216175146,-0.990110426008559,
-0.984125170450909),.UNSPECIFIED.);
#252=B_SPLINE_CURVE_WITH_KNOTS('',3,(#26327,#26328,#26329,#26330,#26331,
#26332,#26333,#26334,#26335,#26336,#26337,#26338,#26339,#26340,#26341,#26342,
#26343,#26344,#26345,#26346,#26347,#26348,#26349,#26350,#26351,#26352,#26353,
#26354,#26355,#26356,#26357,#26358,#26359,#26360,#26361,#26362,#26363,#26364,
#26365,#26366,#26367,#26368,#26369,#26370,#26371,#26372,#26373,#26374,#26375,
#26376,#26377,#26378,#26379,#26380,#26381,#26382,#26383,#26384,#26385,#26386,
#26387,#26388,#26389,#26390,#26391,#26392,#26393,#26394,#26395,#26396,#26397,
#26398,#26399,#26400,#26401,#26402,#26403,#26404,#26405,#26406,#26407,#26408,
#26409,#26410,#26411,#26412,#26413,#26414,#26415,#26416,#26417,#26418,#26419,
#26420,#26421,#26422,#26423,#26424,#26425,#26426,#26427,#26428,#26429,#26430,
#26431,#26432,#26433,#26434,#26435,#26436,#26437,#26438,#26439,#26440,#26441,
#26442,#26443,#26444,#26445,#26446,#26447,#26448,#26449,#26450,#26451,#26452,
#26453,#26454,#26455,#26456,#26457,#26458,#26459,#26460,#26461,#26462,#26463,
#26464,#26465,#26466,#26467,#26468,#26469,#26470,#26471,#26472,#26473,#26474,
#26475,#26476,#26477,#26478,#26479,#26480),.UNSPECIFIED.,.F.,.F.,(4,2,2,
2,2,2,2,2,2,2,2,2,2,2,2,2,2,2,2,2,2,2,2,2,2,2,2,2,2,2,2,2,2,2,2,2,2,2,2,
2,2,2,2,2,2,2,2,2,2,2,2,2,2,2,2,2,2,2,2,2,2,2,2,2,2,2,2,2,2,2,2,2,2,2,2,
2,4),(-0.500647391340917,-0.499639498486703,-0.49800539474486,-0.497003639325043,
-0.496066234440156,-0.494737354861665,-0.49139217980479,-0.486437587803248,
-0.46991231738142,-0.446301415675732,-0.441644678250074,-0.439516225225528,
-0.437868064843415,-0.436078432509876,-0.433196162657974,-0.422876997138652,
-0.402777235394939,-0.384734007803615,-0.38171425531961,-0.380528603712869,
-0.379669054522658,-0.378715406522772,-0.377302930974548,-0.373389589300195,
-0.367251506663444,-0.349846300274575,-0.327151004569,-0.324027407598899,
-0.322005219126954,-0.320372901475535,-0.318501553434403,-0.31524377551086,
-0.299196030475438,-0.284773965386116,-0.276291664139459,-0.265868172486806,
-0.264044597858373,-0.262893982468024,-0.261979108326631,-0.260877915210355,
-0.258785185523965,-0.243080017238911,-0.218048328667486,-0.208815128571274,
-0.205940049704668,-0.204152017778155,-0.202503410059391,-0.200335017329256,
-0.195585686059944,-0.189161174619783,-0.171242939055352,-0.150156380747205,
-0.147205541538612,-0.146031415904382,-0.145174786298885,-0.144217770601365,
-0.142860930542293,-0.139161761110379,-0.133430805034786,-0.11551471264295,
-0.092674529818609,-0.0895504613273472,-0.087528158531183,-0.0858958725695207,
-0.0840246968858895,-0.0810395411596259,-0.0678015620629751,-0.0503895066295616,
-0.0418844031631154,-0.0313964545750801,-0.0295703216737137,-0.0284189473413277,
-0.0275040594930109,-0.0264035584067737,-0.0252196469170199,-0.0233239747058074,
-0.000340432792623708),.UNSPECIFIED.);
#253=B_SPLINE_CURVE_WITH_KNOTS('',3,(#26481,#26482,#26483,#26484,#26485,
#26486,#26487,#26488,#26489,#26490,#26491,#26492,#26493,#26494,#26495,#26496,
#26497,#26498,#26499,#26500,#26501,#26502,#26503,#26504,#26505,#26506,#26507,
#26508,#26509,#26510,#26511,#26512,#26513,#26514,#26515,#26516,#26517,#26518,
#26519,#26520,#26521,#26522,#26523,#26524,#26525,#26526,#26527,#26528,#26529,
#26530,#26531,#26532,#26533,#26534,#26535,#26536,#26537,#26538,#26539,#26540,
#26541,#26542,#26543,#26544,#26545,#26546,#26547,#26548,#26549,#26550,#26551,
#26552),.UNSPECIFIED.,.F.,.F.,(4,2,2,2,2,2,2,2,2,2,2,2,2,2,2,2,2,2,2,2,
2,2,2,2,2,2,2,2,2,2,2,2,2,2,2,4),(-1.48443446178175,-1.46089065681018,-1.45788661713376,
-1.45592251976316,-1.45404488572894,-1.45241367689662,-1.45040133918318,
-1.44730909539555,-1.42950435627513,-1.41442207851342,-1.40338697946608,
-1.39813471340563,-1.39623049618969,-1.39514680960526,-1.39423097514338,
-1.39305929255334,-1.39116495026636,-1.37877035124615,-1.35307080871119,
-1.34176281806496,-1.33869030069849,-1.33681960244217,-1.33518779769318,
-1.33316617520752,-1.33004328948931,-1.30735913496712,-1.2899771230153,
-1.28381041051754,-1.27988462302829,-1.27847069523388,-1.27751695939325,
-1.27665802588238,-1.27547411727258,-1.27246356423765,-1.25356928446698,
-1.24277962970854),.UNSPECIFIED.);
#254=B_SPLINE_CURVE_WITH_KNOTS('',3,(#26553,#26554,#26555,#26556,#26557,
#26558,#26559,#26560,#26561,#26562,#26563,#26564,#26565,#26566,#26567,#26568,
#26569,#26570,#26571,#26572,#26573,#26574,#26575,#26576,#26577,#26578,#26579,
#26580,#26581,#26582,#26583,#26584,#26585,#26586,#26587,#26588,#26589,#26590,
#26591,#26592,#26593,#26594,#26595,#26596,#26597,#26598,#26599,#26600,#26601,
#26602,#26603,#26604,#26605,#26606,#26607,#26608,#26609,#26610,#26611,#26612,
#26613,#26614,#26615,#26616,#26617,#26618,#26619,#26620,#26621,#26622,#26623,
#26624,#26625,#26626,#26627,#26628,#26629,#26630,#26631,#26632,#26633,#26634,
#26635,#26636,#26637,#26638,#26639,#26640,#26641,#26642,#26643,#26644,#26645,
#26646,#26647,#26648,#26649,#26650,#26651,#26652,#26653,#26654,#26655,#26656,
#26657,#26658,#26659,#26660,#26661,#26662,#26663,#26664,#26665,#26666,#26667,
#26668,#26669,#26670,#26671,#26672,#26673,#26674,#26675,#26676,#26677,#26678,
#26679,#26680,#26681,#26682,#26683,#26684,#26685,#26686,#26687,#26688,#26689,
#26690,#26691,#26692,#26693,#26694,#26695,#26696,#26697,#26698,#26699,#26700,
#26701,#26702,#26703,#26704,#26705,#26706,#26707,#26708,#26709,#26710,#26711,
#26712,#26713,#26714,#26715,#26716,#26717,#26718,#26719,#26720,#26721,#26722,
#26723,#26724,#26725,#26726,#26727,#26728,#26729,#26730,#26731,#26732,#26733,
#26734,#26735,#26736,#26737,#26738,#26739,#26740,#26741,#26742,#26743,#26744,
#26745,#26746,#26747,#26748,#26749,#26750,#26751,#26752,#26753,#26754,#26755,
#26756,#26757,#26758,#26759,#26760,#26761,#26762,#26763,#26764,#26765,#26766,
#26767,#26768,#26769,#26770,#26771,#26772),.UNSPECIFIED.,.F.,.F.,(4,2,2,
2,2,2,2,2,2,2,2,2,2,2,2,2,2,2,2,2,2,2,2,2,2,2,2,2,2,2,2,2,2,2,2,2,2,2,2,
2,2,2,2,2,2,2,2,2,2,2,2,2,2,2,2,2,2,2,2,2,2,2,2,2,2,2,2,2,2,2,2,2,2,2,2,
2,2,2,2,2,2,2,2,2,2,2,2,2,2,2,2,2,2,2,2,2,2,2,2,2,2,2,2,2,2,2,2,2,2,4),
(-0.984125170450909,-0.97407182850143,-0.970815026141635,-0.968944090705639,
-0.96731204591619,-0.965290085476164,-0.962166605751026,-0.939512479383253,
-0.92199453602018,-0.915886379681188,-0.911987317587578,-0.910576952629664,
-0.909623851686047,-0.908764104586927,-0.90757731833726,-0.90455023494979,
-0.886650923156437,-0.866473158707528,-0.856132910536406,-0.853249088092647,
-0.851459290146421,-0.849811510631094,-0.847684298960911,-0.843033436833498,
-0.819125754082017,-0.80515467357207,-0.798799627098277,-0.794787830999968,
-0.793362028861912,-0.792405734577381,-0.791548744173856,-0.790372873751615,
-0.787411093245368,-0.76659029702288,-0.742556196047015,-0.737544994545705,
-0.735496907400908,-0.733971130726448,-0.732294820393593,-0.729958311495741,
-0.724211841866047,-0.715941008890753,-0.684524884674582,-0.678168947510021,
-0.67642009919006,-0.675393000118325,-0.674465942141049,-0.673198840031539,
-0.67023100924564,-0.666007197355681,-0.653494958947578,-0.623980232755666,
-0.619724831776662,-0.617648791607647,-0.616011836412843,-0.614176292059367,
-0.611083009889578,-0.598007766065222,-0.581159515513287,-0.563022814900155,
-0.560008464887938,-0.558823773800337,-0.557964523288482,-0.557010731664748,
-0.555597242480497,-0.551675954767237,-0.545520405511775,-0.528133871327585,
-0.505447855231891,-0.502324474460695,-0.500302455058573,-0.498670295283407,
-0.496799153795069,-0.493541808469324,-0.477498892960424,-0.463073482991047,
-0.454587861537948,-0.44416570118901,-0.442342296453984,-0.441191790235998,
-0.440277006243833,-0.439175932973491,-0.437083469240241,-0.421384850782953,
-0.396370048037415,-0.387117389551859,-0.384240427773661,-0.382452098706696,
-0.380803804493003,-0.378636687975238,-0.373893728598252,-0.367480302789346,
-0.349615959939549,-0.328449372292195,-0.325492328793118,-0.324322747544248,
-0.323467303960574,-0.322509014660337,-0.321073816989163,-0.316992230873438,
-0.310483098222279,-0.279712973462818,-0.269965280240216,-0.26703482812587,
-0.265234885836784,-0.263590144338347,-0.261448297256017,-0.256843544035796,
-0.250672178107061,-0.242054869217963),.UNSPECIFIED.);
#255=B_SPLINE_CURVE_WITH_KNOTS('',3,(#26777,#26778,#26779,#26780,#26781,
#26782,#26783,#26784,#26785,#26786,#26787,#26788,#26789,#26790,#26791,#26792,
#26793,#26794,#26795,#26796,#26797,#26798,#26799,#26800,#26801,#26802,#26803,
#26804,#26805,#26806,#26807,#26808,#26809,#26810,#26811,#26812,#26813,#26814,
#26815,#26816,#26817,#26818,#26819,#26820,#26821,#26822,#26823,#26824,#26825,
#26826,#26827,#26828,#26829,#26830,#26831,#26832,#26833,#26834,#26835,#26836,
#26837,#26838,#26839,#26840,#26841,#26842,#26843,#26844,#26845,#26846,#26847,
#26848,#26849,#26850,#26851,#26852,#26853,#26854,#26855,#26856,#26857,#26858,
#26859,#26860,#26861,#26862,#26863,#26864,#26865,#26866,#26867,#26868,#26869,
#26870,#26871,#26872,#26873,#26874,#26875,#26876,#26877,#26878,#26879,#26880,
#26881,#26882,#26883,#26884,#26885,#26886,#26887,#26888,#26889,#26890,#26891,
#26892,#26893,#26894,#26895,#26896,#26897,#26898,#26899,#26900,#26901,#26902,
#26903,#26904,#26905,#26906,#26907,#26908,#26909,#26910,#26911,#26912,#26913,
#26914,#26915,#26916,#26917,#26918,#26919,#26920,#26921,#26922,#26923,#26924,
#26925,#26926,#26927,#26928,#26929,#26930,#26931,#26932,#26933,#26934,#26935,
#26936,#26937,#26938,#26939,#26940,#26941,#26942,#26943,#26944,#26945,#26946,
#26947,#26948,#26949,#26950,#26951,#26952,#26953,#26954,#26955,#26956,#26957,
#26958,#26959,#26960,#26961,#26962,#26963,#26964,#26965,#26966,#26967,#26968,
#26969,#26970,#26971,#26972,#26973,#26974,#26975,#26976,#26977,#26978,#26979,
#26980,#26981,#26982,#26983,#26984),.UNSPECIFIED.,.F.,.F.,(4,2,2,2,2,2,
2,2,2,2,2,2,2,2,2,2,2,2,2,2,2,2,2,2,2,2,2,2,2,2,2,2,2,2,2,2,2,2,2,2,2,2,
2,2,2,2,2,2,2,2,2,2,2,2,2,2,2,2,2,2,2,2,2,2,2,2,2,2,2,2,2,2,2,2,2,2,2,2,
2,2,2,2,2,2,2,2,2,2,2,2,2,2,2,2,2,2,2,2,2,2,2,2,2,4),(-1.24263702846597,
-1.21318204125405,-1.20668394162792,-1.2026079522997,-1.20117368459524,
-1.20021573497816,-1.19936036831268,-1.19819061535303,-1.19523158708895,
-1.17415333775118,-1.15625741807759,-1.14983841312723,-1.14509208811516,
-1.14292461731375,-1.14127652211616,-1.1394888621142,-1.13661397937199,
-1.12737796729563,-1.10234087453071,-1.08663332268865,-1.08454083805351,
-1.08343987270461,-1.0825252414519,-1.08137500452467,-1.07955218315156,
-1.06913547580294,-1.06066302248118,-1.04625712501536,-1.03021692183133,
-1.02696030267285,-1.0250895103207,-1.02345761023854,-1.02143585249069,
-1.01831272488349,-0.995673761011148,-0.978176214080962,-0.972051717356255,
-0.968145257884437,-0.966733947595452,-0.965780711316288,-0.96492123366464,
-0.963735312041772,-0.960712907556075,-0.942754067174463,-0.923307836845784,
-0.912396341343931,-0.909463460698849,-0.907663068389353,-0.906018596350264,
-0.90391373711316,-0.899385000741499,-0.872697190659421,-0.866911669328857,
-0.856828816303559,-0.85132266614208,-0.849722645100682,-0.84872855869881,
-0.84779814828582,-0.846666767923126,-0.843878943672105,-0.819468487625621,
-0.80374533106142,-0.797792922152787,-0.7933143730306,-0.791196025174085,
-0.789554368042603,-0.787742753837772,-0.784758625013523,-0.774491004888847,
-0.742217401027794,-0.734556201747298,-0.73271976552013,-0.731662714385639,
-0.730835309910871,-0.729675702444195,-0.727294411249541,-0.724124765209694,
-0.716157177941159,-0.69265620664322,-0.678546369365,-0.675314852353816,
-0.67343055937763,-0.671962655776449,-0.670030086160236,-0.666484890115924,
-0.641390254293036,-0.619048416234183,-0.6161506160245,-0.614985507410493,
-0.61404626461817,-0.613065956967291,-0.611529052542682,-0.606617777449525,
-0.598129789399926,-0.572459425364615,-0.560963779758772,-0.557870980775725,
-0.556035496943811,-0.554562180195069,-0.552566357253889,-0.548715797012864,
-0.527532513346686,-0.504896939276271,-0.500647391340917),.UNSPECIFIED.);
#256=B_SPLINE_CURVE_WITH_KNOTS('',3,(#26986,#26987,#26988,#26989,#26990,
#26991,#26992,#26993,#26994,#26995,#26996,#26997,#26998,#26999,#27000,#27001,
#27002,#27003,#27004,#27005,#27006,#27007,#27008,#27009,#27010,#27011,#27012,
#27013,#27014,#27015,#27016,#27017,#27018,#27019,#27020,#27021,#27022,#27023,
#27024,#27025,#27026,#27027,#27028,#27029,#27030,#27031,#27032,#27033,#27034,
#27035,#27036,#27037,#27038,#27039,#27040,#27041,#27042,#27043,#27044,#27045,
#27046,#27047,#27048,#27049,#27050,#27051,#27052,#27053,#27054,#27055,#27056,
#27057),.UNSPECIFIED.,.F.,.F.,(4,2,2,2,2,2,2,2,2,2,2,2,2,2,2,2,2,2,2,2,
2,2,2,2,2,2,2,2,2,2,2,2,2,2,2,4),(-0.242054869217963,-0.233961635944292,
-0.211059150468313,-0.208203119345212,-0.207045277770996,-0.206108043714239,
-0.205125090610733,-0.2035757841274,-0.198552110910142,-0.189774820774933,
-0.16214525028512,-0.152668588143719,-0.149765271130868,-0.147971264397082,
-0.146324848842791,-0.144296933346305,-0.139974595621538,-0.134225302276008,
-0.119377292428596,-0.0979828763116323,-0.0918935951311966,-0.0901705991383185,
-0.0891492783533216,-0.0882204133828071,-0.0869410689661844,-0.0840209540877586,
-0.0719012620377772,-0.0544965872382285,-0.036441255927238,-0.0333421070009472,
-0.0313275138753943,-0.0296959552808848,-0.0278195547636938,-0.0258572145078923,
-0.0228576454510606,-0.000340382138819982),.UNSPECIFIED.);
#257=B_SPLINE_CURVE_WITH_KNOTS('',3,(#27058,#27059,#27060,#27061,#27062,
#27063,#27064,#27065,#27066,#27067,#27068,#27069,#27070,#27071,#27072,#27073,
#27074,#27075,#27076,#27077,#27078,#27079,#27080,#27081,#27082,#27083,#27084,
#27085,#27086,#27087,#27088,#27089,#27090,#27091,#27092,#27093,#27094,#27095,
#27096,#27097,#27098,#27099,#27100,#27101,#27102,#27103,#27104,#27105,#27106,
#27107,#27108,#27109,#27110,#27111,#27112,#27113,#27114,#27115,#27116,#27117,
#27118,#27119,#27120,#27121,#27122,#27123,#27124,#27125,#27126,#27127,#27128,
#27129,#27130,#27131,#27132,#27133,#27134,#27135,#27136,#27137,#27138,#27139,
#27140,#27141,#27142,#27143,#27144,#27145,#27146,#27147,#27148,#27149,#27150,
#27151,#27152,#27153,#27154,#27155,#27156,#27157,#27158,#27159,#27160,#27161,
#27162,#27163,#27164,#27165,#27166,#27167,#27168,#27169,#27170,#27171,#27172,
#27173,#27174,#27175,#27176,#27177,#27178,#27179,#27180,#27181,#27182,#27183,
#27184,#27185,#27186,#27187,#27188,#27189,#27190,#27191,#27192,#27193,#27194,
#27195,#27196,#27197,#27198,#27199,#27200,#27201,#27202,#27203,#27204,#27205,
#27206,#27207,#27208,#27209,#27210,#27211),.UNSPECIFIED.,.F.,.F.,(4,2,2,
2,2,2,2,2,2,2,2,2,2,2,2,2,2,2,2,2,2,2,2,2,2,2,2,2,2,2,2,2,2,2,2,2,2,2,2,
2,2,2,2,2,2,2,2,2,2,2,2,2,2,2,2,2,2,2,2,2,2,2,2,2,2,2,2,2,2,2,2,2,2,2,2,
2,4),(-1.48458759282926,-1.46058697544366,-1.45866771350882,-1.45747422433994,
-1.45636704735927,-1.45545247293161,-1.45430884437518,-1.45250830884724,
-1.44255926386911,-1.43962645768021,-1.4331831010642,-1.41717709970874,
-1.40296091072758,-1.39991153561542,-1.39834225269685,-1.3967251338865,
-1.39485812141508,-1.39170288973667,-1.37881620306246,-1.35128299416862,
-1.34501066975361,-1.34105977743947,-1.33962819745971,-1.33867058345057,
-1.33781439048956,-1.33664210027279,-1.33369368708015,-1.31251888695154,
-1.29467382174839,-1.28826405676497,-1.28352256866965,-1.28135551600932,
-1.27970701794204,-1.27791822129416,-1.27503996664619,-1.26577836806808,
-1.24074880814399,-1.22504151992479,-1.22294838556946,-1.22184705434025,
-1.22093210743715,-1.21978146648348,-1.21795799648213,-1.20753775159071,
-1.19905887010152,-1.18464396698514,-1.16860045217859,-1.16534277370507,
-1.16347134788721,-1.16183888288917,-1.15981641163107,-1.15669216159334,
-1.13399890515511,-1.11661311965169,-1.11043880635247,-1.10650906136972,
-1.10509423407258,-1.10414004559071,-1.10328082915723,-1.10209669380087,
-1.0990864434082,-1.08014901481529,-1.06139257796928,-1.05069311927257,
-1.04777743005807,-1.04598038395088,-1.04433422133456,-1.04222062911883,
-1.03764662189543,-1.01169550990352,-0.996854830014449,-0.992186646215384,
-0.988986906274839,-0.987681081609704,-0.986747645672439,-0.98573699111287,
-0.984187833277004),.UNSPECIFIED.);
#258=B_SPLINE_CURVE_WITH_KNOTS('',3,(#27217,#27218,#27219,#27220,#27221,
#27222,#27223,#27224,#27225,#27226,#27227,#27228,#27229,#27230,#27231,#27232,
#27233,#27234,#27235,#27236,#27237,#27238,#27239,#27240,#27241,#27242,#27243,
#27244,#27245,#27246,#27247,#27248,#27249,#27250,#27251,#27252,#27253,#27254,
#27255,#27256,#27257,#27258,#27259,#27260,#27261,#27262,#27263,#27264,#27265,
#27266,#27267,#27268,#27269,#27270,#27271,#27272,#27273,#27274,#27275,#27276,
#27277,#27278,#27279,#27280,#27281,#27282,#27283,#27284,#27285,#27286,#27287,
#27288,#27289,#27290,#27291,#27292,#27293,#27294,#27295,#27296,#27297,#27298,
#27299,#27300,#27301,#27302,#27303,#27304,#27305,#27306,#27307,#27308,#27309,
#27310,#27311,#27312,#27313,#27314,#27315,#27316,#27317,#27318,#27319,#27320,
#27321,#27322,#27323,#27324,#27325,#27326,#27327,#27328,#27329,#27330,#27331,
#27332,#27333,#27334,#27335,#27336,#27337,#27338,#27339,#27340,#27341,#27342,
#27343,#27344,#27345,#27346,#27347,#27348,#27349,#27350,#27351,#27352,#27353,
#27354,#27355,#27356,#27357,#27358,#27359,#27360,#27361,#27362,#27363,#27364,
#27365,#27366,#27367,#27368,#27369,#27370,#27371,#27372),.UNSPECIFIED.,
 .F.,.F.,(4,2,2,2,2,2,2,2,2,2,2,2,2,2,2,2,2,2,2,2,2,2,2,2,2,2,2,2,2,2,2,
2,2,2,2,2,2,2,2,2,2,2,2,2,2,2,2,2,2,2,2,2,2,2,2,2,2,2,2,2,2,2,2,2,2,2,2,
2,2,2,2,2,2,2,2,2,2,4),(-0.500904416667459,-0.488914936864186,-0.482753931044674,
-0.480282045965134,-0.478749662876254,-0.477078835279314,-0.474773500539124,
-0.469223350727045,-0.448226833297894,-0.424766938789263,-0.421933650815843,
-0.42077966519421,-0.419843357066977,-0.418858654971897,-0.41730180004511,
-0.412210393844688,-0.403256835821251,-0.372993911786864,-0.365820246994291,
-0.363198158870924,-0.361637886018321,-0.359985417112075,-0.357790528858627,
-0.352892711957206,-0.346204284411774,-0.312830303232384,-0.305749199823953,
-0.303936007185761,-0.302894683371461,-0.301971508569885,-0.300732312691038,
-0.297925247255231,-0.285246569714141,-0.281204120939117,-0.251379284141169,
-0.247161814559687,-0.245092965453389,-0.243456571176483,-0.241616284144362,
-0.238501868889925,-0.225100708636843,-0.208788184800751,-0.190471595618797,
-0.187462636303479,-0.186278755528788,-0.185419642396299,-0.184465455524613,
-0.183050439980223,-0.179118832938403,-0.172941019127285,-0.155577318348858,
-0.132903586014866,-0.129779571939499,-0.127757229975083,-0.126202956225671,
-0.124401598177523,-0.122500883026045,-0.119651487100752,-0.114420828537869,
-0.10165075677646,-0.0830288291128392,-0.0787527746289728,-0.0713027843680808,
-0.0694816105326993,-0.0684279823263795,-0.067599904919146,-0.0664349943354398,
-0.0640269665966417,-0.0608114600192663,-0.0526697262820125,-0.0229582393288504,
-0.0143963324163041,-0.0115986933566161,-0.00982746605347513,-0.00825927673259034,
-0.00665175994948807,-0.00386382252695999,-0.000340186971329014),
 .UNSPECIFIED.);
#259=B_SPLINE_CURVE_WITH_KNOTS('',3,(#27373,#27374,#27375,#27376,#27377,
#27378,#27379,#27380,#27381,#27382,#27383,#27384,#27385,#27386,#27387,#27388,
#27389,#27390,#27391,#27392,#27393,#27394,#27395,#27396,#27397,#27398,#27399,
#27400,#27401,#27402,#27403,#27404,#27405,#27406,#27407,#27408,#27409,#27410,
#27411,#27412,#27413,#27414,#27415,#27416,#27417,#27418,#27419,#27420,#27421,
#27422,#27423,#27424,#27425,#27426,#27427,#27428,#27429,#27430,#27431,#27432,
#27433,#27434,#27435,#27436,#27437,#27438,#27439,#27440,#27441,#27442,#27443,
#27444),.UNSPECIFIED.,.F.,.F.,(4,2,2,2,2,2,2,2,2,2,2,2,2,2,2,2,2,2,2,2,
2,2,2,2,2,2,2,2,2,2,2,2,2,2,2,4),(-1.48415219493652,-1.45250665935878,-1.43944929105978,
-1.43660293167591,-1.43535716127721,-1.43443347557021,-1.43339645273249,
-1.43160142939977,-1.42472731610342,-1.39388168211648,-1.38566028126054,
-1.3817626330946,-1.3794336443774,-1.37740835295126,-1.37581764842499,-1.37406145438945,
-1.37133086339452,-1.3633397768778,-1.33411460502419,-1.32516815228624,
-1.32008057132548,-1.31852452873993,-1.31754027375196,-1.31660432588514,
-1.31545073133081,-1.31261810310143,-1.28919955682737,-1.2728623832405,
-1.26677319357932,-1.26221562455362,-1.26008281571874,-1.25843959769232,
-1.25663592016143,-1.25368706467827,-1.24377101569511,-1.24263702846597),
 .UNSPECIFIED.);
#260=B_SPLINE_CURVE_WITH_KNOTS('',3,(#27445,#27446,#27447,#27448,#27449,
#27450,#27451,#27452,#27453,#27454,#27455,#27456,#27457,#27458,#27459,#27460,
#27461,#27462,#27463,#27464,#27465,#27466,#27467,#27468,#27469,#27470,#27471,
#27472,#27473,#27474,#27475,#27476,#27477,#27478,#27479,#27480,#27481,#27482,
#27483,#27484,#27485,#27486,#27487,#27488,#27489,#27490,#27491,#27492,#27493,
#27494,#27495,#27496,#27497,#27498,#27499,#27500,#27501,#27502,#27503,#27504,
#27505,#27506,#27507,#27508,#27509,#27510,#27511,#27512,#27513,#27514,#27515,
#27516,#27517,#27518,#27519,#27520,#27521,#27522,#27523,#27524,#27525,#27526,
#27527,#27528,#27529,#27530,#27531,#27532,#27533,#27534,#27535,#27536,#27537,
#27538,#27539,#27540,#27541,#27542,#27543,#27544,#27545,#27546,#27547,#27548,
#27549,#27550,#27551,#27552,#27553,#27554,#27555,#27556,#27557,#27558,#27559,
#27560,#27561,#27562,#27563,#27564,#27565,#27566,#27567,#27568,#27569,#27570,
#27571,#27572,#27573,#27574,#27575,#27576,#27577,#27578,#27579,#27580,#27581,
#27582,#27583,#27584,#27585,#27586,#27587,#27588,#27589,#27590,#27591,#27592,
#27593,#27594,#27595,#27596,#27597,#27598,#27599,#27600,#27601,#27602,#27603,
#27604,#27605,#27606,#27607,#27608,#27609,#27610,#27611,#27612,#27613,#27614,
#27615,#27616,#27617,#27618,#27619,#27620,#27621,#27622,#27623,#27624,#27625,
#27626,#27627,#27628,#27629,#27630,#27631,#27632,#27633,#27634,#27635,#27636,
#27637,#27638,#27639,#27640,#27641,#27642,#27643,#27644,#27645,#27646,#27647,
#27648,#27649,#27650,#27651,#27652),.UNSPECIFIED.,.F.,.F.,(4,2,2,2,2,2,
2,2,2,2,2,2,2,2,2,2,2,2,2,2,2,2,2,2,2,2,2,2,2,2,2,2,2,2,2,2,2,2,2,2,2,2,
2,2,2,2,2,2,2,2,2,2,2,2,2,2,2,2,2,2,2,2,2,2,2,2,2,2,2,2,2,2,2,2,2,2,2,2,
2,2,2,2,2,2,2,2,2,2,2,2,2,2,2,2,2,2,2,2,2,2,2,2,2,4),(-0.984187833277004,
-0.984063074238169,-0.978450970218995,-0.946255889702368,-0.933671315699779,
-0.930610757768473,-0.928782191797354,-0.927143696133262,-0.925055065774211,
-0.920735070982084,-0.891741437880094,-0.873935118102472,-0.871384090055669,
-0.870191716335036,-0.869282132623342,-0.868215878699228,-0.866339583889734,
-0.858088985999228,-0.837676606763139,-0.820197434904205,-0.814744510263714,
-0.812454814896139,-0.810786564171258,-0.809250462259531,-0.807161527518278,
-0.803003906840926,-0.77798118750282,-0.77051401785999,-0.757155451106151,
-0.754276937838385,-0.753025141909919,-0.752100220133899,-0.75106540712829,
-0.749281982408049,-0.742548236253123,-0.728171352650195,-0.7015813823746,
-0.697045603661932,-0.694939064384009,-0.693293943636355,-0.691493518778946,
-0.688562133239908,-0.677676895975676,-0.658323046831343,-0.64018079092848,
-0.637166050881948,-0.635981179168268,-0.635121788266104,-0.634167829492333,
-0.632754073338513,-0.628831920967881,-0.622674892176426,-0.605285878494386,
-0.58259625897793,-0.579472349815046,-0.577449988229246,-0.575817552172951,
-0.573946093869864,-0.570688196814293,-0.55464255837595,-0.54021471160418,
-0.53172765678937,-0.52130373187606,-0.519480018465419,-0.518329317488355,
-0.517414378642223,-0.516313118986224,-0.514220301059465,-0.498519026007381,
-0.473499990978974,-0.464245763688528,-0.461368314635313,-0.459579682783899,
-0.457931109566543,-0.455763626331094,-0.451019864790236,-0.444605354592505,
-0.426737993928148,-0.405567813974401,-0.402610270336967,-0.401440491180134,
-0.4005849028065,-0.399626451261733,-0.398191010520867,-0.394108732576942,
-0.387598496056274,-0.356823131798161,-0.347073816342459,-0.344142871193565,
-0.342342624871686,-0.340697604766851,-0.338555393741221,-0.333949853585836,
-0.327777430014588,-0.311063999139821,-0.288157727357864,-0.285301208436593,
-0.284143170112735,-0.283205777201962,-0.282222657999818,-0.28067309059857,
-0.275648579221517,-0.266869835047864,-0.24195210917092),.UNSPECIFIED.);
#261=B_SPLINE_CURVE_WITH_KNOTS('',3,(#27657,#27658,#27659,#27660,#27661,
#27662,#27663,#27664,#27665,#27666,#27667,#27668,#27669,#27670,#27671,#27672,
#27673,#27674,#27675,#27676,#27677,#27678,#27679,#27680,#27681,#27682,#27683,
#27684,#27685,#27686,#27687,#27688,#27689,#27690,#27691,#27692,#27693,#27694,
#27695,#27696,#27697,#27698,#27699,#27700,#27701,#27702,#27703,#27704,#27705,
#27706,#27707,#27708,#27709,#27710,#27711,#27712,#27713,#27714,#27715,#27716,
#27717,#27718,#27719,#27720,#27721,#27722,#27723,#27724,#27725,#27726,#27727,
#27728,#27729,#27730,#27731,#27732,#27733,#27734,#27735,#27736,#27737,#27738,
#27739,#27740,#27741,#27742,#27743,#27744,#27745,#27746,#27747,#27748,#27749,
#27750,#27751,#27752,#27753,#27754,#27755,#27756,#27757,#27758,#27759,#27760,
#27761,#27762,#27763,#27764,#27765,#27766,#27767,#27768,#27769,#27770,#27771,
#27772,#27773,#27774,#27775,#27776,#27777,#27778,#27779,#27780,#27781,#27782,
#27783,#27784,#27785,#27786,#27787,#27788,#27789,#27790,#27791,#27792,#27793,
#27794,#27795,#27796,#27797,#27798,#27799,#27800,#27801,#27802,#27803,#27804,
#27805,#27806,#27807,#27808,#27809,#27810,#27811,#27812,#27813,#27814,#27815,
#27816,#27817,#27818,#27819,#27820,#27821,#27822,#27823,#27824,#27825,#27826,
#27827,#27828,#27829,#27830,#27831,#27832,#27833,#27834,#27835,#27836,#27837,
#27838,#27839,#27840,#27841,#27842,#27843,#27844,#27845,#27846,#27847,#27848,
#27849,#27850,#27851,#27852,#27853,#27854,#27855,#27856,#27857,#27858,#27859,
#27860,#27861,#27862,#27863,#27864,#27865,#27866,#27867,#27868,#27869,#27870,
#27871,#27872,#27873,#27874,#27875,#27876),.UNSPECIFIED.,.F.,.F.,(4,2,2,
2,2,2,2,2,2,2,2,2,2,2,2,2,2,2,2,2,2,2,2,2,2,2,2,2,2,2,2,2,2,2,2,2,2,2,2,
2,2,2,2,2,2,2,2,2,2,2,2,2,2,2,2,2,2,2,2,2,2,2,2,2,2,2,2,2,2,2,2,2,2,2,2,
2,2,2,2,2,2,2,2,2,2,2,2,2,2,2,2,2,2,2,2,2,2,2,2,2,2,2,2,2,2,2,2,2,2,4),
(-1.24297521476333,-1.24178430330719,-1.2407892377459,-1.2398594153016,
-1.23873030622846,-1.23584128673268,-1.21225132719135,-1.19602034423567,
-1.18995416829667,-1.18540971178841,-1.1832791163697,-1.18163595351687,
-1.17983068646783,-1.176875451765,-1.16690786539197,-1.136369321897,-1.12987381025455,
-1.12579878310798,-1.12436449258101,-1.12340642663823,-1.12255087799421,
-1.12138077834746,-1.11845314324577,-1.09686490306256,-1.07931013273746,
-1.07296052444913,-1.06825343285418,-1.06609284780836,-1.06444550374562,
-1.06265427832567,-1.05976392697298,-1.05038554422044,-1.01919080192893,
-1.0126523011671,-1.00855791829819,-1.00712096149052,-1.00616227001806,
-1.00530705435517,-1.00413852527222,-1.00118876385751,-0.979881373816018,
-0.970179038659431,-0.959040382489031,-0.9542549889917,-0.95047733223311,
-0.948496383874068,-0.947024558171151,-0.945178625829668,-0.942037900888435,
-0.929941866463692,-0.904800335910472,-0.896402661586025,-0.893120935736141,
-0.890674791609677,-0.889502513112402,-0.888586405601287,-0.887502614532241,
-0.885548408230798,-0.875951478474062,-0.847727392713301,-0.835664287092581,
-0.832641003931838,-0.830820673514944,-0.829180684903721,-0.827077848656834,
-0.82268265679223,-0.794400138325365,-0.789120013035911,-0.779642858053847,
-0.77435557114362,-0.772777799555301,-0.771788497314846,-0.770855059290487,
-0.769497243191671,-0.766939491179242,-0.742639181609929,-0.719225679507449,
-0.716092905355166,-0.714067982967697,-0.71243553693369,-0.710566318056714,
-0.707318141091196,-0.6914732664365,-0.667192625678609,-0.657814376218448,
-0.655871527380021,-0.654790284353407,-0.653873914277331,-0.652698202928157,
-0.650234293968244,-0.646922062453605,-0.638405858242854,-0.612559902350962,
-0.601252591386285,-0.598173839350377,-0.596341369014647,-0.594867498273093,
-0.592867005260843,-0.588993687962437,-0.584053049682493,-0.572359328853213,
-0.550729594376325,-0.540644767981708,-0.538834996304174,-0.537688545525651,
-0.536773825614432,-0.535669009110655,-0.533558934009499,-0.516791755470417,
-0.500904416667459),.UNSPECIFIED.);
#262=B_SPLINE_CURVE_WITH_KNOTS('',3,(#27878,#27879,#27880,#27881,#27882,
#27883,#27884,#27885,#27886,#27887,#27888,#27889,#27890,#27891,#27892,#27893,
#27894,#27895,#27896,#27897,#27898,#27899,#27900,#27901,#27902,#27903,#27904,
#27905,#27906,#27907,#27908,#27909,#27910,#27911,#27912,#27913,#27914,#27915,
#27916,#27917,#27918,#27919,#27920,#27921,#27922,#27923,#27924,#27925,#27926,
#27927,#27928,#27929,#27930,#27931,#27932,#27933,#27934,#27935,#27936,#27937,
#27938,#27939,#27940,#27941,#27942,#27943,#27944,#27945,#27946,#27947,#27948,
#27949,#27950,#27951,#27952,#27953,#27954,#27955,#27956,#27957,#27958,#27959,
#27960,#27961,#27962,#27963,#27964,#27965,#27966,#27967,#27968,#27969,#27970,
#27971,#27972,#27973),.UNSPECIFIED.,.F.,.F.,(4,2,2,2,2,2,2,2,2,2,2,2,2,
2,2,2,2,2,2,2,2,2,2,2,2,2,2,2,2,2,2,2,2,2,2,2,2,2,2,2,2,2,2,2,2,2,2,4),
(-0.24195210917092,-0.238328488327181,-0.229588572179531,-0.226768044860348,
-0.224991863617181,-0.223339128956458,-0.221142891645517,-0.216237812400091,
-0.209536522718923,-0.190201936325325,-0.17111711888477,-0.168109251654614,
-0.166925582219484,-0.166066547761138,-0.165112362510809,-0.163697210693321,
-0.159764343264134,-0.153583735231869,-0.127098530275104,-0.113201832761435,
-0.109963132552584,-0.108077153460812,-0.106515775731751,-0.106468973102604,
-0.106426895041746,-0.106388872976778,-0.106354360927049,-0.106322908301707,
-0.106294139580394,-0.106267739191376,-0.106243439735482,-0.106221013094132,
-0.106200263406243,-0.106181021379253,-0.104140310014139,-0.10185746950122,
-0.0980749726181405,-0.0902054561595218,-0.0762115215929237,-0.0536776523592188,
-0.0507964390220819,-0.0496341658065563,-0.0486956722841141,-0.0477142621794448,
-0.0461723714497,-0.0412167655535401,-0.0326156466268484,-0.000340676557468298),
 .UNSPECIFIED.);
#263=B_SPLINE_CURVE_WITH_KNOTS('',3,(#27974,#27975,#27976,#27977,#27978,
#27979,#27980,#27981,#27982,#27983,#27984,#27985,#27986,#27987,#27988,#27989,
#27990,#27991,#27992,#27993,#27994,#27995,#27996,#27997,#27998,#27999,#28000,
#28001,#28002,#28003,#28004,#28005,#28006,#28007,#28008,#28009,#28010,#28011,
#28012,#28013,#28014,#28015,#28016,#28017,#28018,#28019,#28020,#28021,#28022,
#28023,#28024,#28025,#28026,#28027,#28028,#28029,#28030,#28031,#28032,#28033,
#28034,#28035,#28036,#28037,#28038,#28039,#28040,#28041,#28042,#28043,#28044,
#28045,#28046,#28047,#28048,#28049,#28050,#28051,#28052,#28053,#28054,#28055,
#28056,#28057,#28058,#28059,#28060,#28061,#28062,#28063,#28064,#28065,#28066,
#28067,#28068,#28069,#28070,#28071,#28072,#28073,#28074,#28075,#28076,#28077,
#28078,#28079,#28080,#28081,#28082,#28083,#28084,#28085,#28086,#28087,#28088,
#28089,#28090,#28091,#28092,#28093,#28094,#28095,#28096,#28097,#28098,#28099,
#28100,#28101,#28102,#28103,#28104,#28105,#28106,#28107,#28108,#28109,#28110,
#28111,#28112,#28113,#28114,#28115,#28116,#28117,#28118,#28119,#28120,#28121,
#28122,#28123,#28124,#28125,#28126,#28127,#28128,#28129,#28130,#28131),
 .UNSPECIFIED.,.F.,.F.,(4,2,2,2,2,2,2,2,2,2,2,2,2,2,2,2,2,2,2,2,2,2,2,2,
2,2,2,2,2,2,2,2,2,2,2,2,2,2,2,2,2,2,2,2,2,2,2,2,2,2,2,2,2,2,2,2,2,2,2,2,
2,2,2,2,2,2,2,2,2,2,2,2,2,2,2,2,2,2,4),(-1.48414639998802,-1.47879596711116,
-1.47672811482419,-1.47513078917331,-1.47355491489769,-1.47176712386732,
-1.46889001650299,-1.45962481974856,-1.4303154511884,-1.42248294561508,
-1.4193496963634,-1.4169900760554,-1.41583505940126,-1.4150084929214,-1.41394912438853,
-1.41210121870852,-1.40426639083598,-1.38357072828186,-1.36965356907349,
-1.36413094592819,-1.3611725882687,-1.35922749315818,-1.35785980986077,
-1.3562535279143,-1.35443282884722,-1.35140522134449,-1.34081341629944,
-1.31097581125902,-1.30452929211255,-1.3004765952843,-1.29904557068101,
-1.2980883975217,-1.29723265241524,-1.29606104276559,-1.29312323915568,
-1.27179471894925,-1.25407071477623,-1.24768703116408,-1.24296089283786,
-1.24079726407342,-1.23914991497618,-1.23736094604149,-1.23447926685457,
-1.22517629163125,-1.20019888619625,-1.18451474018673,-1.18242292043329,
-1.18132219180586,-1.18040769389663,-1.17925755260603,-1.177434755803,-1.16701401108436,
-1.15852001135506,-1.14406096663784,-1.12809609592202,-1.12484330607293,
-1.12297351262465,-1.12134178294259,-1.11931933073128,-1.11619339605062,
-1.09364164715054,-1.07657104027939,-1.0701293754927,-1.066078771608,-1.06464795804046,
-1.06369077751449,-1.0628349108017,-1.06166299032605,-1.05871614006145,
-1.03754977192699,-1.01971235405795,-1.01330529838588,-1.00856580598276,
-1.00639965774219,-1.0047518445645,-1.00296378806579,-1.00008671764343,
-0.990828864930486,-0.983855788104838),.UNSPECIFIED.);
#264=B_SPLINE_CURVE_WITH_KNOTS('',3,(#28137,#28138,#28139,#28140,#28141,
#28142,#28143,#28144,#28145,#28146,#28147,#28148,#28149,#28150,#28151,#28152,
#28153,#28154,#28155,#28156,#28157,#28158,#28159,#28160,#28161,#28162,#28163,
#28164,#28165,#28166,#28167,#28168,#28169,#28170,#28171,#28172,#28173,#28174,
#28175,#28176,#28177,#28178,#28179,#28180,#28181,#28182,#28183,#28184,#28185,
#28186,#28187,#28188,#28189,#28190,#28191,#28192,#28193,#28194,#28195,#28196,
#28197,#28198,#28199,#28200,#28201,#28202,#28203,#28204,#28205,#28206,#28207,
#28208,#28209,#28210,#28211,#28212,#28213,#28214,#28215,#28216,#28217,#28218,
#28219,#28220,#28221,#28222,#28223,#28224,#28225,#28226,#28227,#28228,#28229,
#28230,#28231,#28232,#28233,#28234,#28235,#28236,#28237,#28238,#28239,#28240,
#28241,#28242,#28243,#28244,#28245,#28246,#28247,#28248,#28249,#28250,#28251,
#28252,#28253,#28254,#28255,#28256,#28257,#28258,#28259,#28260,#28261,#28262,
#28263,#28264,#28265,#28266,#28267,#28268,#28269,#28270,#28271,#28272,#28273,
#28274,#28275,#28276,#28277,#28278,#28279,#28280,#28281,#28282,#28283,#28284,
#28285,#28286,#28287,#28288,#28289,#28290,#28291,#28292,#28293,#28294,#28295,
#28296,#28297,#28298,#28299,#28300,#28301,#28302,#28303,#28304,#28305,#28306,
#28307,#28308,#28309,#28310,#28311,#28312),.UNSPECIFIED.,.F.,.F.,(4,2,2,
2,2,2,2,2,2,2,2,2,2,2,2,2,2,2,2,2,2,2,2,2,2,2,2,2,2,2,2,2,2,2,2,2,2,2,2,
2,2,2,2,2,2,2,2,2,2,2,2,2,2,2,2,2,2,2,2,2,2,2,2,2,2,2,2,2,2,2,2,2,2,2,2,
2,2,2,2,2,2,2,2,2,2,2,2,4),(-0.500748493306363,-0.49428692095435,-0.484922197772312,
-0.464917275796128,-0.461933188638434,-0.460753645807397,-0.459895791679644,
-0.458940716612863,-0.457520474447514,-0.453548867408227,-0.447282813202204,
-0.433688506878275,-0.409274829434102,-0.404640682058993,-0.402516634232706,
-0.400869454990949,-0.399078454711964,-0.396188568931295,-0.385778132769649,
-0.365340749507521,-0.35778139146162,-0.352681271788409,-0.34574068117324,
-0.343939730573339,-0.342901304730169,-0.341977787907235,-0.340734188676198,
-0.337900836587531,-0.324970390781765,-0.31596860700133,-0.292093305837505,
-0.287443722188799,-0.285316879102415,-0.283669285805314,-0.281879589823099,
-0.27899570893954,-0.268653041192708,-0.248463825045924,-0.23054057302486,
-0.227528186485945,-0.226343923968489,-0.225484866009631,-0.224531141102751,
-0.223117492994218,-0.219194088543173,-0.213033507100442,-0.195658058721139,
-0.172981378241405,-0.169858574019207,-0.167836891831768,-0.166204978352811,
-0.164334088730973,-0.161077096032481,-0.145032875160836,-0.121429840704774,
-0.111647275020201,-0.109678777977246,-0.108591909625912,-0.107704495495276,
-0.107698414936022,-0.107692449169858,-0.107686594814106,-0.107680848348299,
-0.107675206756756,-0.107669666820321,-0.107664225280265,-0.107658879427332,
-0.107653626655327,-0.107648464394768,-0.107643389723269,-0.107638399987156,
-0.107633493353716,-0.10762866745188,-0.10762391987864,-0.107619248728151,
-0.106453069992474,-0.105145280717095,-0.102942585751177,-0.0982663456840263,
-0.0833750968508959,-0.0575424237070847,-0.0529662632000266,-0.0508527080196141,
-0.0492069928625414,-0.0474108571577775,-0.0444975950420383,-0.0338192939406861,
-0.0003407532546169),.UNSPECIFIED.);
#265=B_SPLINE_CURVE_WITH_KNOTS('',3,(#28313,#28314,#28315,#28316,#28317,
#28318,#28319,#28320,#28321,#28322,#28323,#28324,#28325,#28326,#28327,#28328,
#28329,#28330,#28331,#28332,#28333,#28334,#28335,#28336,#28337,#28338,#28339,
#28340,#28341,#28342,#28343,#28344,#28345,#28346,#28347,#28348,#28349,#28350,
#28351,#28352,#28353,#28354,#28355,#28356,#28357,#28358,#28359,#28360,#28361,
#28362,#28363,#28364,#28365,#28366,#28367,#28368,#28369,#28370,#28371,#28372,
#28373,#28374,#28375,#28376,#28377,#28378,#28379,#28380,#28381,#28382,#28383,
#28384,#28385,#28386,#28387,#28388,#28389,#28390),.UNSPECIFIED.,.F.,.F.,
(4,2,2,2,2,2,2,2,2,2,2,2,2,2,2,2,2,2,2,2,2,2,2,2,2,2,2,2,2,2,2,2,2,2,2,
2,2,2,4),(-1.4845396710087,-1.47825139841739,-1.47693547624366,-1.47598577733424,
-1.47512798895945,-1.4742724086583,-1.47310213361687,-1.47014318743695,
-1.46279099408039,-1.43184755347238,-1.42158280980162,-1.41870593319078,
-1.41691775279343,-1.41526965765706,-1.41313950038778,-1.40847165261581,
-1.38564972473863,-1.36850507613455,-1.36345178115162,-1.3611272845425,
-1.35977109015024,-1.35856925747271,-1.35766369141969,-1.35662573750668,
-1.35482701010589,-1.34791232985656,-1.31710109178158,-1.30888142439269,
-1.30316099809011,-1.30082880731301,-1.29915345656426,-1.29762709434516,
-1.29557602800734,-1.29054642150204,-1.26148084161633,-1.2591535564171,
-1.24894087425676,-1.24338887098085,-1.24297521476333),.UNSPECIFIED.);
#266=B_SPLINE_CURVE_WITH_KNOTS('',3,(#28391,#28392,#28393,#28394,#28395,
#28396,#28397,#28398,#28399,#28400,#28401,#28402,#28403,#28404,#28405,#28406,
#28407,#28408,#28409,#28410,#28411,#28412,#28413,#28414,#28415,#28416,#28417,
#28418,#28419,#28420,#28421,#28422,#28423,#28424,#28425,#28426,#28427,#28428,
#28429,#28430,#28431,#28432,#28433,#28434,#28435,#28436,#28437,#28438,#28439,
#28440,#28441,#28442,#28443,#28444,#28445,#28446,#28447,#28448,#28449,#28450,
#28451,#28452,#28453,#28454,#28455,#28456,#28457,#28458,#28459,#28460,#28461,
#28462,#28463,#28464,#28465,#28466,#28467,#28468,#28469,#28470,#28471,#28472,
#28473,#28474,#28475,#28476,#28477,#28478,#28479,#28480,#28481,#28482,#28483,
#28484,#28485,#28486,#28487,#28488,#28489,#28490,#28491,#28492,#28493,#28494,
#28495,#28496,#28497,#28498,#28499,#28500,#28501,#28502,#28503,#28504,#28505,
#28506,#28507,#28508,#28509,#28510,#28511,#28512,#28513,#28514,#28515,#28516,
#28517,#28518,#28519,#28520,#28521,#28522,#28523,#28524,#28525,#28526,#28527,
#28528,#28529,#28530,#28531,#28532,#28533,#28534,#28535,#28536,#28537,#28538,
#28539,#28540,#28541,#28542,#28543,#28544,#28545,#28546,#28547,#28548,#28549,
#28550,#28551,#28552,#28553,#28554,#28555,#28556,#28557,#28558,#28559,#28560,
#28561,#28562,#28563,#28564,#28565,#28566,#28567,#28568,#28569,#28570,#28571,
#28572,#28573,#28574,#28575,#28576,#28577,#28578,#28579,#28580,#28581,#28582,
#28583,#28584,#28585,#28586,#28587,#28588,#28589,#28590,#28591,#28592,#28593,
#28594,#28595,#28596,#28597,#28598,#28599,#28600,#28601,#28602,#28603,#28604,
#28605,#28606),.UNSPECIFIED.,.F.,.F.,(4,2,2,2,2,2,2,2,2,2,2,2,2,2,2,2,2,
2,2,2,2,2,2,2,2,2,2,2,2,2,2,2,2,2,2,2,2,2,2,2,2,2,2,2,2,2,2,2,2,2,2,2,2,
2,2,2,2,2,2,2,2,2,2,2,2,2,2,2,2,2,2,2,2,2,2,2,2,2,2,2,2,2,2,2,2,2,2,2,2,
2,2,2,2,2,2,2,2,2,2,2,2,2,2,2,2,2,2,4),(-0.983855788104838,-0.965809777789558,
-0.950109041312935,-0.948016776262846,-0.946915902240519,-0.946001335059476,
-0.944851171507917,-0.943028457812708,-0.932612525586969,-0.924135814794796,
-0.903475602414132,-0.896535907110599,-0.891498414251561,-0.889279396724808,
-0.887623518238953,-0.886070729696273,-0.883486783921482,-0.876579308626038,
-0.846070805215775,-0.837035067306361,-0.833592482985266,-0.831054356812462,
-0.829864673453913,-0.828947366190847,-0.827876601616018,-0.825979424848689,
-0.817387058739746,-0.792773610314513,-0.776467420910509,-0.773198765935964,
-0.771325413425742,-0.769693821747222,-0.76767573005686,-0.764564561227109,
-0.742158727986369,-0.718372188321029,-0.714458202767508,-0.713001840444135,
-0.712134793876668,-0.711189080498951,-0.709815355129405,-0.706172999867635,
-0.700611864858019,-0.680893449506599,-0.659613177578876,-0.656474670260101,
-0.654448205543137,-0.652815917961458,-0.650948414851934,-0.647707187672623,
-0.631999140297674,-0.608990551083149,-0.598315311597118,-0.596481949013811,
-0.595328493033816,-0.594413654402313,-0.593315262268302,-0.591235337667744,
-0.576174440874272,-0.552773189977835,-0.541623316051212,-0.538557176063239,
-0.53672768106786,-0.535089855039159,-0.533004139294621,-0.528697725471281,
-0.512076598720576,-0.506718548796849,-0.482318524299208,-0.479768087862753,
-0.478412319073975,-0.477479380395934,-0.476489669375229,-0.474909575517582,
-0.469598277720327,-0.4600563960465,-0.45254867384428,-0.426917611851322,
-0.422331241682865,-0.420215792150934,-0.418569775819305,-0.416774497920194,
-0.41386529928985,-0.403235032277134,-0.384690536708838,-0.365441217666579,
-0.362436574851348,-0.361253558961388,-0.360394786799302,-0.359440636924612,
-0.358025101151982,-0.354088342340681,-0.347898825130568,-0.330550558740069,
-0.307885384806987,-0.304762317169975,-0.302740494935786,-0.301108490709808,
-0.299237523593117,-0.295980471554556,-0.279938725486797,-0.265514938704909,
-0.257030275753172,-0.246609090184405,-0.244785858177224,-0.243635461160612,
-0.24272076414252,-0.241877241928533),.UNSPECIFIED.);
#267=B_SPLINE_CURVE_WITH_KNOTS('',3,(#28611,#28612,#28613,#28614,#28615,
#28616,#28617,#28618,#28619,#28620,#28621,#28622,#28623,#28624,#28625,#28626,
#28627,#28628,#28629,#28630,#28631,#28632,#28633,#28634,#28635,#28636,#28637,
#28638,#28639,#28640,#28641,#28642,#28643,#28644,#28645,#28646,#28647,#28648,
#28649,#28650,#28651,#28652,#28653,#28654,#28655,#28656,#28657,#28658,#28659,
#28660,#28661,#28662,#28663,#28664,#28665,#28666,#28667,#28668,#28669,#28670,
#28671,#28672,#28673,#28674,#28675,#28676,#28677,#28678,#28679,#28680,#28681,
#28682,#28683,#28684,#28685,#28686,#28687,#28688,#28689,#28690,#28691,#28692,
#28693,#28694,#28695,#28696,#28697,#28698,#28699,#28700,#28701,#28702,#28703,
#28704,#28705,#28706,#28707,#28708,#28709,#28710,#28711,#28712,#28713,#28714,
#28715,#28716,#28717,#28718,#28719,#28720,#28721,#28722,#28723,#28724,#28725,
#28726,#28727,#28728,#28729,#28730,#28731,#28732,#28733,#28734,#28735,#28736,
#28737,#28738,#28739,#28740,#28741,#28742,#28743,#28744,#28745,#28746,#28747,
#28748,#28749,#28750,#28751,#28752,#28753,#28754,#28755,#28756,#28757,#28758,
#28759,#28760,#28761,#28762,#28763,#28764,#28765,#28766,#28767,#28768,#28769,
#28770,#28771,#28772,#28773,#28774,#28775,#28776,#28777,#28778,#28779,#28780,
#28781,#28782,#28783,#28784,#28785,#28786,#28787,#28788,#28789,#28790,#28791,
#28792,#28793,#28794,#28795,#28796,#28797,#28798,#28799,#28800,#28801,#28802,
#28803,#28804,#28805,#28806,#28807,#28808,#28809,#28810,#28811,#28812,#28813,
#28814,#28815,#28816,#28817,#28818,#28819,#28820,#28821,#28822,#28823,#28824,
#28825,#28826,#28827,#28828,#28829,#28830,#28831,#28832,#28833,#28834),
 .UNSPECIFIED.,.F.,.F.,(4,2,2,2,2,2,2,2,2,2,2,2,2,2,2,2,2,2,2,2,2,2,2,2,
2,2,2,2,2,2,2,2,2,2,2,2,2,2,2,2,2,2,2,2,2,2,2,2,2,2,2,2,2,2,2,2,2,2,2,2,
2,2,2,2,2,2,2,2,2,2,2,2,2,2,2,2,2,2,2,2,2,2,2,2,2,2,2,2,2,2,2,2,2,2,2,2,
2,2,2,2,2,2,2,2,2,2,2,2,2,2,2,4),(-1.24268594727471,-1.22755581692661,-1.22432347418344,
-1.22245781579084,-1.22082520574043,-1.21879581845494,-1.21564787247119,
-1.19369863506161,-1.17787628935238,-1.16660182088411,-1.16463204259183,
-1.16355693602476,-1.16264004536171,-1.16145626216942,-1.15952148159293,
-1.14290544250946,-1.14031384061548,-1.12004351463544,-1.10967801598931,
-1.10679191268082,-1.10500158874819,-1.10335391673355,-1.10122767071859,
-1.0965823204256,-1.07247287634745,-1.05864564918267,-1.05232390861533,
-1.04832720624053,-1.04690342782924,-1.04594753729696,-1.04509016260734,
-1.04391281937489,-1.04094236936503,-1.02037193114212,-0.994354415997967,
-0.990382185316445,-0.988361935933999,-0.986730011197086,-0.984857825740183,
-0.981679223001586,-0.968458238618318,-0.944298963011325,-0.936096468314974,
-0.932865405007933,-0.93044862619079,-0.929282131400289,-0.928453995807091,
-0.927401744395747,-0.925586114114291,-0.918206194702676,-0.892477557667124,
-0.881499054283819,-0.876759459693661,-0.873010372474889,-0.871035447096061,
-0.869564357328636,-0.86771445549058,-0.864554783621135,-0.85216491102753,
-0.829563440267243,-0.816313274741673,-0.813446397677439,-0.812196827591933,
-0.811272410555561,-0.810236887632161,-0.808449483398962,-0.801666860940497,
-0.795091525755241,-0.776105621024928,-0.762036472673339,-0.756652062138215,
-0.754373994147937,-0.752708071502994,-0.751169820092415,-0.74866514730882,
-0.742273599084137,-0.732454671033082,-0.717256136422843,-0.716267613065891,
-0.709836627486398,-0.697899151248068,-0.696021774109766,-0.694855094029024,
-0.693939502098999,-0.692851745128487,-0.690822416681446,-0.67779529566062,
-0.647806365400008,-0.640312943408168,-0.637647327979162,-0.636078917953427,
-0.634430700929729,-0.632263147368133,-0.627516995138471,-0.621097697146585,
-0.603202373629714,-0.58209146851319,-0.5791423891782,-0.577968838660747,
-0.577112466532503,-0.576155540932334,-0.574726524667804,-0.570690395294082,
-0.564282073127849,-0.534962743979483,-0.523876297780399,-0.52081292074943,
-0.518984087625428,-0.517346235808414,-0.515259636324544,-0.510948267202939,
-0.500748493306363),.UNSPECIFIED.);
#268=B_SPLINE_CURVE_WITH_KNOTS('',3,(#28836,#28837,#28838,#28839,#28840,
#28841,#28842,#28843,#28844,#28845,#28846,#28847,#28848,#28849,#28850,#28851,
#28852,#28853,#28854,#28855,#28856,#28857,#28858,#28859,#28860,#28861,#28862,
#28863,#28864,#28865,#28866,#28867,#28868,#28869,#28870,#28871,#28872,#28873,
#28874,#28875,#28876,#28877,#28878,#28879,#28880,#28881,#28882,#28883,#28884,
#28885,#28886,#28887,#28888,#28889,#28890,#28891,#28892,#28893,#28894,#28895,
#28896,#28897,#28898,#28899,#28900,#28901,#28902,#28903,#28904,#28905,#28906,
#28907,#28908,#28909,#28910,#28911,#28912,#28913),.UNSPECIFIED.,.F.,.F.,
(4,2,2,2,2,2,2,2,2,2,2,2,2,2,2,2,2,2,2,2,2,2,2,2,2,2,2,2,2,2,2,2,2,2,2,
2,2,2,4),(-0.241877241928533,-0.241619795735405,-0.239527531769983,-0.223830450244459,
-0.198818140520498,-0.189566229696313,-0.186689527539865,-0.18490136548066,
-0.183253228964646,-0.18108632530501,-0.1763438545345,-0.16993110489117,
-0.152068786838454,-0.130903271091689,-0.127946836819323,-0.126777426883858,
-0.125922079540128,-0.12498314209916,-0.123597336807539,-0.121977159984821,
-0.118966747174926,-0.111591014881524,-0.0956008125452895,-0.0734238926969615,
-0.0703071856780489,-0.0682873153153312,-0.0666554782071564,-0.0647831551336937,
-0.0615197191439157,-0.0453375296941648,-0.0198558688782215,-0.0125674908445179,
-0.0103143655522347,-0.00916539692384771,-0.00830733410877659,-0.0074399773927748,
-0.00637126135853562,-0.00397532333556067,-0.000340107566605497),
 .UNSPECIFIED.);
#269=B_SPLINE_CURVE_WITH_KNOTS('',3,(#28914,#28915,#28916,#28917,#28918,
#28919,#28920,#28921,#28922,#28923,#28924,#28925,#28926,#28927,#28928,#28929,
#28930,#28931,#28932,#28933,#28934,#28935,#28936,#28937,#28938,#28939,#28940,
#28941,#28942,#28943,#28944,#28945,#28946,#28947,#28948,#28949,#28950,#28951,
#28952,#28953,#28954,#28955,#28956,#28957,#28958,#28959,#28960,#28961,#28962,
#28963,#28964,#28965,#28966,#28967,#28968,#28969,#28970,#28971,#28972,#28973,
#28974,#28975,#28976,#28977,#28978,#28979,#28980,#28981,#28982,#28983,#28984,
#28985,#28986,#28987,#28988,#28989,#28990,#28991,#28992,#28993,#28994,#28995,
#28996,#28997,#28998,#28999,#29000,#29001,#29002,#29003,#29004,#29005,#29006,
#29007,#29008,#29009,#29010,#29011,#29012,#29013,#29014,#29015,#29016,#29017,
#29018,#29019,#29020,#29021,#29022,#29023,#29024,#29025,#29026,#29027,#29028,
#29029,#29030,#29031,#29032,#29033,#29034,#29035,#29036,#29037,#29038,#29039,
#29040,#29041,#29042,#29043,#29044,#29045,#29046,#29047,#29048,#29049,#29050,
#29051,#29052,#29053,#29054,#29055,#29056,#29057,#29058,#29059,#29060,#29061,
#29062,#29063,#29064,#29065,#29066,#29067,#29068,#29069,#29070,#29071,#29072,
#29073,#29074,#29075,#29076,#29077,#29078,#29079,#29080,#29081,#29082,#29083,
#29084,#29085,#29086,#29087,#29088,#29089,#29090,#29091,#29092,#29093,#29094,
#29095,#29096,#29097,#29098,#29099,#29100,#29101,#29102,#29103,#29104,#29105,
#29106,#29107,#29108,#29109,#29110,#29111,#29112,#29113,#29114,#29115,#29116,
#29117,#29118,#29119,#29120,#29121,#29122,#29123,#29124,#29125,#29126,#29127,
#29128,#29129),.UNSPECIFIED.,.F.,.F.,(4,2,2,2,2,2,2,2,2,2,2,2,2,2,2,2,2,
2,2,2,2,2,2,2,2,2,2,2,2,2,2,2,2,2,2,2,2,2,2,2,2,2,2,2,2,2,2,2,2,2,2,2,2,
2,2,2,2,2,2,2,2,2,2,2,2,2,2,2,2,2,2,2,2,2,2,2,2,2,2,2,2,2,2,2,2,2,2,2,2,
2,2,2,2,2,2,2,2,2,2,2,2,2,2,2,2,2,2,4),(-1.48447813887855,-1.44993276123579,
-1.43927478434815,-1.43636367976403,-1.43456823207176,-1.43292272299963,
-1.43080884476849,-1.42622965472528,-1.4004434401445,-1.3855033320513,-1.38081848943171,
-1.37861317048929,-1.37730443095426,-1.37614079035221,-1.37613605869907,
-1.37613125331992,-1.37612637225832,-1.37612141321535,-1.37611637423337,
-1.37611125273326,-1.37610604652552,-1.37610075312672,-1.37609536991382,
-1.3760898940988,-1.37608432296462,-1.37607865368691,-1.37607288307957,
-1.37606700803392,-1.37606102528906,-1.37605493150694,-1.37604872296438,
-1.37604239585419,-1.37603594645505,-1.37602937069825,-1.37602266430301,
-1.37601582273936,-1.37600884136323,-1.37600171541581,-1.37599443974402,
-1.37598700887642,-1.37597941731928,-1.37597165902972,-1.3759637280546,
-1.37595561801138,-1.37594732184286,-1.37593883240099,-1.37593014241902,
-1.37592124375391,-1.37591212815086,-1.37590278676235,-1.37589321016808,
-1.37588338865127,-1.37587331194629,-1.37498866611297,-1.37381651593659,
-1.37192039595824,-1.3591470933345,-1.33820005982344,-1.32266967375351,
-1.31943763208308,-1.3175723091197,-1.31594009015537,-1.31391131850543,
-1.31076458408937,-1.28881473386802,-1.27299023212113,-1.26172354491973,
-1.25975441002599,-1.25867959255592,-1.25776291208425,-1.25657936100898,
-1.25464488755773,-1.2379426226308,-1.22238556063083,-1.21121795724662,
-1.20642481677116,-1.20264259182654,-1.20066107801255,-1.1991895928448,
-1.19734507984015,-1.19420923329042,-1.18217622009633,-1.15698640207302,
-1.1485807886006,-1.14529733714547,-1.14285035998046,-1.14167813590655,
-1.14084943818705,-1.13980127523412,-1.13800297259332,-1.13083968860688,
-1.10027943698269,-1.08788812530975,-1.08484197076202,-1.08301703865256,
-1.08137867826305,-1.07928591849728,-1.07494150809859,-1.04619586832003,
-1.02807759218667,-1.02560935266101,-1.02443303813311,-1.02351689909638,
-1.02243675107123,-1.02049784122899,-1.01118306214216,-0.98781186896046,
-0.984053158365659),.UNSPECIFIED.);
#270=B_SPLINE_CURVE_WITH_KNOTS('',3,(#29135,#29136,#29137,#29138,#29139,
#29140,#29141,#29142,#29143,#29144,#29145,#29146,#29147,#29148,#29149,#29150,
#29151,#29152,#29153,#29154,#29155,#29156,#29157,#29158,#29159,#29160,#29161,
#29162,#29163,#29164,#29165,#29166,#29167,#29168,#29169,#29170,#29171,#29172,
#29173,#29174,#29175,#29176,#29177,#29178,#29179,#29180,#29181,#29182,#29183,
#29184,#29185,#29186,#29187,#29188,#29189,#29190,#29191,#29192,#29193,#29194,
#29195,#29196,#29197,#29198,#29199,#29200,#29201,#29202,#29203,#29204,#29205,
#29206,#29207,#29208,#29209,#29210,#29211,#29212,#29213,#29214,#29215,#29216,
#29217,#29218,#29219,#29220,#29221,#29222,#29223,#29224,#29225,#29226,#29227,
#29228,#29229,#29230,#29231,#29232,#29233,#29234,#29235,#29236,#29237,#29238,
#29239,#29240,#29241,#29242,#29243,#29244,#29245,#29246,#29247,#29248,#29249,
#29250,#29251,#29252,#29253,#29254,#29255,#29256,#29257,#29258,#29259,#29260,
#29261,#29262,#29263,#29264,#29265,#29266,#29267,#29268,#29269,#29270,#29271,
#29272,#29273,#29274,#29275,#29276,#29277,#29278,#29279,#29280,#29281,#29282),
 .UNSPECIFIED.,.F.,.F.,(4,2,2,2,2,2,2,2,2,2,2,2,2,2,2,2,2,2,2,2,2,2,2,2,
2,2,2,2,2,2,2,2,2,2,2,2,2,2,2,2,2,2,2,2,2,2,2,2,2,2,2,2,2,2,2,2,2,2,2,2,
2,2,2,2,2,2,2,2,2,2,2,2,2,4),(-0.500718660599513,-0.500400110751097,-0.499485194754859,
-0.498383951653016,-0.496291128044058,-0.480585339217535,-0.455552758774148,
-0.446318844691955,-0.443443603602185,-0.441655483213064,-0.4400068022588,
-0.437838325418924,-0.433088860312599,-0.426664202145293,-0.408745872232347,
-0.387657274117378,-0.38469691583698,-0.383526242184164,-0.382670446764753,
-0.381712305522132,-0.380278259986341,-0.376206248176301,-0.369718777818682,
-0.339281763618541,-0.329232131553156,-0.3262671757704,-0.32445953670125,
-0.32281652375529,-0.320689403586707,-0.316165165775265,-0.310133647655511,
-0.294061021399678,-0.270183115964008,-0.267310718879712,-0.266184045913166,
-0.265254659316578,-0.264258070727483,-0.262647365048782,-0.25703590953585,
-0.246656247942295,-0.223171151518339,-0.212166094743792,-0.209109414932852,
-0.207281748994032,-0.205643170510959,-0.203553208998678,-0.19922593986097,
-0.182443437973725,-0.177168294017118,-0.152890594518186,-0.150051337484662,
-0.148929896799405,-0.148001770147206,-0.147002675151922,-0.145380684613584,
-0.139743376234368,-0.129247968276644,-0.0975350303846231,-0.0928880002702371,
-0.0907613711845579,-0.0891135527506156,-0.0873232211707997,-0.0846943827588374,
-0.0757706437612646,-0.0600534964439603,-0.0355967045487589,-0.0328105664360528,
-0.0316793483313575,-0.0307488626859592,-0.0297544200010428,-0.028153331282767,
-0.0262405493043127,-0.0224210226223817,-0.000340524436432586),
 .UNSPECIFIED.);
#271=B_SPLINE_CURVE_WITH_KNOTS('',3,(#29283,#29284,#29285,#29286,#29287,
#29288,#29289,#29290,#29291,#29292,#29293,#29294,#29295,#29296,#29297,#29298,
#29299,#29300,#29301,#29302,#29303,#29304,#29305,#29306,#29307,#29308,#29309,
#29310,#29311,#29312,#29313,#29314,#29315,#29316,#29317,#29318,#29319,#29320,
#29321,#29322,#29323,#29324,#29325,#29326,#29327,#29328,#29329,#29330,#29331,
#29332,#29333,#29334,#29335,#29336,#29337,#29338,#29339,#29340,#29341,#29342,
#29343,#29344,#29345,#29346,#29347,#29348,#29349,#29350,#29351,#29352,#29353,
#29354),.UNSPECIFIED.,.F.,.F.,(4,2,2,2,2,2,2,2,2,2,2,2,2,2,2,2,2,2,2,2,
2,2,2,2,2,2,2,2,2,2,2,2,2,2,2,4),(-1.48436044637623,-1.46363610470996,-1.46068896284307,
-1.45874821980611,-1.45718862764179,-1.45555887871019,-1.45365730467275,
-1.45034881516589,-1.43463884215802,-1.42021635804648,-1.40262751754562,
-1.39967722319634,-1.39839279491649,-1.39746314436856,-1.39644410144448,
-1.39473132793389,-1.38874376399468,-1.36461110167954,-1.35155221209812,
-1.34624658357989,-1.3421873911038,-1.34020994604938,-1.33857067988293,
-1.33674843809142,-1.33371556245394,-1.32307255532416,-1.29657665364041,
-1.28390853466999,-1.28188995060368,-1.28080445990665,-1.27988865565304,
-1.27871900136947,-1.27683172631911,-1.26462104590702,-1.24308133150857,
-1.24268594727471),.UNSPECIFIED.);
#272=B_SPLINE_CURVE_WITH_KNOTS('',3,(#29355,#29356,#29357,#29358,#29359,
#29360,#29361,#29362,#29363,#29364,#29365,#29366,#29367,#29368,#29369,#29370,
#29371,#29372,#29373,#29374,#29375,#29376,#29377,#29378,#29379,#29380,#29381,
#29382,#29383,#29384,#29385,#29386,#29387,#29388,#29389,#29390,#29391,#29392,
#29393,#29394,#29395,#29396,#29397,#29398,#29399,#29400,#29401,#29402,#29403,
#29404,#29405,#29406,#29407,#29408,#29409,#29410,#29411,#29412,#29413,#29414,
#29415,#29416,#29417,#29418,#29419,#29420,#29421,#29422,#29423,#29424,#29425,
#29426,#29427,#29428,#29429,#29430,#29431,#29432,#29433,#29434,#29435,#29436,
#29437,#29438,#29439,#29440,#29441,#29442,#29443,#29444,#29445,#29446,#29447,
#29448,#29449,#29450,#29451,#29452,#29453,#29454,#29455,#29456,#29457,#29458,
#29459,#29460,#29461,#29462,#29463,#29464,#29465,#29466,#29467,#29468,#29469,
#29470,#29471,#29472,#29473,#29474,#29475,#29476,#29477,#29478,#29479,#29480,
#29481,#29482,#29483,#29484,#29485,#29486,#29487,#29488,#29489,#29490,#29491,
#29492,#29493,#29494,#29495,#29496,#29497,#29498,#29499,#29500,#29501,#29502,
#29503,#29504,#29505,#29506,#29507,#29508,#29509,#29510,#29511,#29512,#29513,
#29514,#29515,#29516,#29517,#29518,#29519,#29520,#29521,#29522,#29523,#29524,
#29525,#29526,#29527,#29528,#29529,#29530,#29531,#29532,#29533,#29534,#29535,
#29536,#29537,#29538,#29539,#29540,#29541,#29542,#29543,#29544,#29545,#29546,
#29547,#29548,#29549,#29550,#29551,#29552,#29553,#29554,#29555,#29556,#29557,
#29558,#29559,#29560,#29561,#29562,#29563,#29564,#29565,#29566,#29567,#29568,
#29569,#29570,#29571,#29572,#29573,#29574,#29575,#29576,#29577,#29578,#29579,
#29580,#29581,#29582),.UNSPECIFIED.,.F.,.F.,(4,2,2,2,2,2,2,2,2,2,2,2,2,
2,2,2,2,2,2,2,2,2,2,2,2,2,2,2,2,2,2,2,2,2,2,2,2,2,2,2,2,2,2,2,2,2,2,2,2,
2,2,2,2,2,2,2,2,2,2,2,2,2,2,2,2,2,2,2,2,2,2,2,2,2,2,2,2,2,2,2,2,2,2,2,2,
2,2,2,2,2,2,2,2,2,2,2,2,2,2,2,2,2,2,2,2,2,2,2,2,2,2,2,2,4),(-0.984053158365659,
-0.976712214041789,-0.971938326079979,-0.968168042193585,-0.966188961947261,
-0.964717695965065,-0.962871387267738,-0.959727351554003,-0.947571129667715,
-0.922489498362212,-0.914103868233824,-0.9108255446165,-0.90838151843392,
-0.9072098554621,-0.906381217433222,-0.90533266880774,-0.903532722358874,
-0.896349507928024,-0.870543513232499,-0.859473608806476,-0.854708173774071,
-0.850943138830566,-0.84896513230403,-0.84749396486923,-0.845646866275643,
-0.842499214437275,-0.83028799089571,-0.805254535093528,-0.7968779395003,
-0.793601939096763,-0.791159251771831,-0.78998784530935,-0.789159236268877,
-0.788110515683509,-0.786309829345756,-0.779117582648423,-0.773186504838792,
-0.754131010132862,-0.742554441257789,-0.735376790812867,-0.732754482784648,
-0.73119439673305,-0.729542360984107,-0.727348452454022,-0.722454571965926,
-0.715772781417891,-0.682486535913121,-0.675324631505821,-0.673526115415097,
-0.672477796291944,-0.671648943625247,-0.670476477744319,-0.66802887530248,
-0.656800353861006,-0.633140999369956,-0.619348152390165,-0.616134707900035,
-0.614254591994021,-0.612623361630794,-0.610613732337479,-0.60669443748868,
-0.601678733498216,-0.589710902974336,-0.563749878213513,-0.557865332505684,
-0.556162893592807,-0.555146068428914,-0.554215438867957,-0.552925471012426,
-0.549821522909534,-0.545338915834534,-0.531505575690141,-0.504112789416371,
-0.499693826973797,-0.497578602710253,-0.495932504309026,-0.494136877236163,
-0.491226529294816,-0.480584881549858,-0.462006164841777,-0.442799051953094,
-0.43979489528577,-0.438611902128175,-0.437753088318309,-0.436798821947255,
-0.435382993596101,-0.431444645446266,-0.425251861771903,-0.40790502918907,
-0.385239412731637,-0.382116080563427,-0.380094086933948,-0.378461944266476,
-0.376590818334384,-0.3733334895627,-0.357290373499673,-0.342865369498245,
-0.334379990628789,-0.323957920559101,-0.322134533860992,-0.3209840392454,
-0.320069264630318,-0.318968202829638,-0.316875761391885,-0.301177349361784,
-0.276162920683849,-0.266910221622156,-0.264033275071036,-0.262244961239208,
-0.260596684931616,-0.258429597620231,-0.253686725490098,-0.247273433524857,
-0.24206462708761),.UNSPECIFIED.);
#273=B_SPLINE_CURVE_WITH_KNOTS('',3,(#29587,#29588,#29589,#29590,#29591,
#29592,#29593,#29594,#29595,#29596,#29597,#29598,#29599,#29600,#29601,#29602,
#29603,#29604,#29605,#29606,#29607,#29608,#29609,#29610,#29611,#29612,#29613,
#29614,#29615,#29616,#29617,#29618,#29619,#29620,#29621,#29622,#29623,#29624,
#29625,#29626,#29627,#29628,#29629,#29630,#29631,#29632,#29633,#29634,#29635,
#29636,#29637,#29638,#29639,#29640,#29641,#29642,#29643,#29644,#29645,#29646,
#29647,#29648,#29649,#29650,#29651,#29652,#29653,#29654,#29655,#29656,#29657,
#29658,#29659,#29660,#29661,#29662,#29663,#29664,#29665,#29666,#29667,#29668,
#29669,#29670,#29671,#29672,#29673,#29674,#29675,#29676,#29677,#29678,#29679,
#29680,#29681,#29682,#29683,#29684,#29685,#29686,#29687,#29688,#29689,#29690,
#29691,#29692,#29693,#29694,#29695,#29696,#29697,#29698,#29699,#29700,#29701,
#29702,#29703,#29704,#29705,#29706,#29707,#29708,#29709,#29710,#29711,#29712,
#29713,#29714,#29715,#29716,#29717,#29718,#29719,#29720,#29721,#29722,#29723,
#29724,#29725,#29726,#29727,#29728,#29729,#29730,#29731,#29732,#29733,#29734,
#29735,#29736,#29737,#29738,#29739,#29740,#29741,#29742,#29743,#29744,#29745,
#29746,#29747,#29748,#29749,#29750,#29751,#29752,#29753,#29754,#29755,#29756,
#29757,#29758,#29759,#29760,#29761,#29762,#29763,#29764,#29765,#29766,#29767,
#29768,#29769,#29770,#29771,#29772,#29773,#29774,#29775,#29776,#29777,#29778,
#29779,#29780,#29781,#29782,#29783,#29784,#29785,#29786,#29787,#29788,#29789,
#29790,#29791,#29792,#29793,#29794,#29795,#29796,#29797,#29798),
 .UNSPECIFIED.,.F.,.F.,(4,2,2,2,2,2,2,2,2,2,2,2,2,2,2,2,2,2,2,2,2,2,2,2,
2,2,2,2,2,2,2,2,2,2,2,2,2,2,2,2,2,2,2,2,2,2,2,2,2,2,2,2,2,2,2,2,2,2,2,2,
2,2,2,2,2,2,2,2,2,2,2,2,2,2,2,2,2,2,2,2,2,2,2,2,2,2,2,2,2,2,2,2,2,2,2,2,
2,2,2,2,2,2,2,2,2,4),(-1.24280763943444,-1.22268571771476,-1.20697442025643,
-1.2048814307625,-1.20378019948657,-1.20286534714334,-1.2017148319585,-1.19989156922864,
-1.1894723252949,-1.18099836452278,-1.16658994224282,-1.15054449778414,
-1.14728702848753,-1.14541577034329,-1.14378347715707,-1.14176124948906,
-1.13863742880102,-1.11594522248837,-1.09855554159171,-1.0923893115782,
-1.08846341695498,-1.0870492130481,-1.08609522199718,-1.08523600457854,
-1.08405163604696,-1.08103954513751,-1.0617017711617,-1.04324572085829,
-1.03264315039829,-1.02973601405698,-1.02794095392827,-1.02629443483638,
-1.02417735867814,-1.01974970957412,-0.992437002652213,-0.978532823637424,
-0.974036597449419,-0.970925752719812,-0.969634549199411,-0.968703633052056,
-0.967687135350315,-0.965986532964893,-0.960120815296411,-0.934401571214883,
-0.917788636619313,-0.913482654270816,-0.911396766655546,-0.90975862877382,
-0.907928599426175,-0.904861117363274,-0.893700887775741,-0.867697487506419,
-0.859154922406015,-0.854222569158852,-0.85268321140019,-0.851702324373684,
-0.850763374019604,-0.849599536642928,-0.846709405654708,-0.824299533813988,
-0.79996898507792,-0.796013090677606,-0.793995899347205,-0.792363921691072,
-0.790488896037379,-0.787298702047962,-0.773897769001144,-0.751683479680263,
-0.742292270469208,-0.737132641237955,-0.735509917857048,-0.734510653143797,
-0.733571906241908,-0.732235819355497,-0.728844613182002,-0.723798008273827,
-0.70669760969028,-0.683831903439715,-0.679164246231147,-0.677033765165119,
-0.675385244130325,-0.673596427602753,-0.670718147175711,-0.660444524376605,
-0.640509338269064,-0.622230902008625,-0.619221211409352,-0.618037195126648,
-0.617178036025954,-0.616223861290774,-0.614808971413012,-0.61087840916066,
-0.604702924108123,-0.587336260307222,-0.564660018034641,-0.561536305481998,
-0.559514032810818,-0.557881641107584,-0.556010201494232,-0.552752246819358,
-0.536703166304568,-0.522280864721184,-0.513798442718789,-0.503374438652297,
-0.501550779193074,-0.500718660599513),.UNSPECIFIED.);
#274=B_SPLINE_CURVE_WITH_KNOTS('',3,(#29800,#29801,#29802,#29803,#29804,
#29805,#29806,#29807,#29808,#29809,#29810,#29811,#29812,#29813,#29814,#29815,
#29816,#29817,#29818,#29819,#29820,#29821,#29822,#29823,#29824,#29825,#29826,
#29827,#29828,#29829,#29830,#29831,#29832,#29833,#29834,#29835,#29836,#29837,
#29838,#29839,#29840,#29841,#29842,#29843,#29844,#29845,#29846,#29847,#29848,
#29849,#29850,#29851,#29852,#29853,#29854,#29855,#29856,#29857,#29858,#29859,
#29860,#29861,#29862,#29863,#29864,#29865,#29866,#29867,#29868,#29869,#29870,
#29871),.UNSPECIFIED.,.F.,.F.,(4,2,2,2,2,2,2,2,2,2,2,2,2,2,2,2,2,2,2,2,
2,2,2,2,2,2,2,2,2,2,2,2,2,2,2,4),(-0.24206462708761,-0.229409608471203,
-0.208242742972339,-0.205285752764569,-0.204116187756894,-0.203260754000776,
-0.202302473198574,-0.200867283906088,-0.196785692057573,-0.190276519887479,
-0.159505080654677,-0.149758964950301,-0.146828703665975,-0.14502881492429,
-0.14338408059051,-0.141367135341366,-0.137096545683497,-0.131439646267583,
-0.116977336489474,-0.0949351853640112,-0.0889165580126861,-0.0872005837593868,
-0.086180807865097,-0.0852513721303828,-0.0839684884640444,-0.0810276964737433,
-0.0614872094232513,-0.0478088219577944,-0.0332185623453336,-0.0299611576291717,
-0.0280710561831135,-0.0264405409194214,-0.0248773107901266,-0.0229234421895695,
-0.0199444790809123,-0.000340292378937216),.UNSPECIFIED.);
#275=B_SPLINE_CURVE_WITH_KNOTS('',3,(#29872,#29873,#29874,#29875,#29876,
#29877,#29878,#29879,#29880,#29881,#29882,#29883,#29884,#29885,#29886,#29887,
#29888,#29889,#29890,#29891,#29892,#29893,#29894,#29895,#29896,#29897,#29898,
#29899,#29900,#29901,#29902,#29903,#29904,#29905,#29906,#29907,#29908,#29909,
#29910,#29911,#29912,#29913,#29914,#29915,#29916,#29917,#29918,#29919,#29920,
#29921,#29922,#29923,#29924,#29925,#29926,#29927,#29928,#29929,#29930,#29931,
#29932,#29933,#29934,#29935,#29936,#29937,#29938,#29939,#29940,#29941,#29942,
#29943,#29944,#29945,#29946,#29947,#29948,#29949,#29950,#29951,#29952,#29953,
#29954,#29955,#29956,#29957,#29958,#29959,#29960,#29961,#29962,#29963,#29964,
#29965,#29966,#29967,#29968,#29969,#29970,#29971,#29972,#29973,#29974,#29975,
#29976,#29977,#29978,#29979,#29980,#29981,#29982,#29983,#29984,#29985,#29986,
#29987,#29988,#29989,#29990,#29991,#29992,#29993,#29994,#29995,#29996,#29997,
#29998,#29999,#30000,#30001,#30002,#30003,#30004,#30005,#30006,#30007,#30008,
#30009,#30010,#30011,#30012,#30013,#30014,#30015,#30016,#30017,#30018,#30019),
 .UNSPECIFIED.,.F.,.F.,(4,2,2,2,2,2,2,2,2,2,2,2,2,2,2,2,2,2,2,2,2,2,2,2,
2,2,2,2,2,2,2,2,2,2,2,2,2,2,2,2,2,2,2,2,2,2,2,2,2,2,2,2,2,2,2,2,2,2,2,2,
2,2,2,2,2,2,2,2,2,2,2,2,2,4),(-1.48430358760489,-1.4597246532768,-1.45666928759006,
-1.45503241734088,-1.4536170060634,-1.45266294653794,-1.4518042556676,-1.4506213636504,
-1.44761705387336,-1.42846664822781,-1.41207606660783,-1.39953211121336,
-1.39658933449029,-1.39502968458839,-1.39355793220374,-1.39171433500767,
-1.38858313733914,-1.37662208235956,-1.3481760858305,-1.34183125745421,
-1.33785051793992,-1.33641336227839,-1.33545472247536,-1.33459969888755,
-1.33343161981659,-1.33048363578237,-1.30912557320389,-1.29141312718798,
-1.28503105702883,-1.28030553386675,-1.27814165825848,-1.27649390687085,
-1.27470429196992,-1.27182110807929,-1.26250880178412,-1.23753042492945,
-1.22184425250862,-1.21975190116346,-1.21865087963237,-1.21773613073978,
-1.21658566418178,-1.21476233433302,-1.20433789918159,-1.195840689987,-1.18137380408734,
-1.16540978038666,-1.16215634257817,-1.1602860893635,-1.1586539073184,-1.15663082817078,
-1.15350379712415,-1.13095029453175,-1.11387561667634,-1.10742930633547,
-1.10337629692999,-1.10194491760816,-1.10098743847175,-1.1001313666006,
-1.09895924280717,-1.09601124304522,-1.07483943412046,-1.05699688614121,
-1.05058802556939,-1.04584720654982,-1.04368045973566,-1.04203219434918,
-1.0402436502048,-1.03736580189195,-1.02810551124147,-1.00307948367819,
-0.987374412326566,-0.98528157341315,-0.984180397635834,-0.984002691704062),
 .UNSPECIFIED.);
#276=B_SPLINE_CURVE_WITH_KNOTS('',3,(#30025,#30026,#30027,#30028,#30029,
#30030,#30031,#30032,#30033,#30034,#30035,#30036,#30037,#30038,#30039,#30040,
#30041,#30042,#30043,#30044,#30045,#30046,#30047,#30048,#30049,#30050,#30051,
#30052,#30053,#30054,#30055,#30056,#30057,#30058,#30059,#30060,#30061,#30062,
#30063,#30064,#30065,#30066,#30067,#30068,#30069,#30070,#30071,#30072,#30073,
#30074,#30075,#30076,#30077,#30078,#30079,#30080,#30081,#30082,#30083,#30084,
#30085,#30086,#30087,#30088,#30089,#30090,#30091,#30092,#30093,#30094,#30095,
#30096,#30097,#30098,#30099,#30100,#30101,#30102,#30103,#30104,#30105,#30106,
#30107,#30108,#30109,#30110,#30111,#30112,#30113,#30114,#30115,#30116,#30117,
#30118,#30119,#30120,#30121,#30122,#30123,#30124,#30125,#30126,#30127,#30128,
#30129,#30130,#30131,#30132,#30133,#30134,#30135,#30136,#30137,#30138,#30139,
#30140,#30141,#30142,#30143,#30144,#30145,#30146,#30147,#30148,#30149,#30150,
#30151,#30152,#30153,#30154,#30155,#30156,#30157,#30158,#30159,#30160,#30161,
#30162,#30163,#30164,#30165,#30166,#30167,#30168,#30169,#30170,#30171,#30172,
#30173,#30174,#30175,#30176,#30177,#30178,#30179,#30180),.UNSPECIFIED.,
 .F.,.F.,(4,2,2,2,2,2,2,2,2,2,2,2,2,2,2,2,2,2,2,2,2,2,2,2,2,2,2,2,2,2,2,
2,2,2,2,2,2,2,2,2,2,2,2,2,2,2,2,2,2,2,2,2,2,2,2,2,2,2,2,2,2,2,2,2,2,2,2,
2,2,2,2,2,2,2,2,2,2,4),(-0.500846823737344,-0.487606703081641,-0.484483003251093,
-0.482460739216415,-0.480828354744568,-0.478956923707451,-0.475698984702297,
-0.459650001234931,-0.445227745706519,-0.436745349986905,-0.426321393802306,
-0.424497742511653,-0.423347079203627,-0.42243216727492,-0.421330929051376,
-0.419238114666127,-0.403532391399216,-0.378499911225953,-0.369266050860534,
-0.366390823885218,-0.364602711733264,-0.362954038010901,-0.360785570154017,
-0.356036122533534,-0.349611486527616,-0.331693204732785,-0.310604747112755,
-0.307644398212804,-0.306473729904561,-0.305617938322044,-0.304659801291414,
-0.303225761916063,-0.299153766635581,-0.292666321621788,-0.262229390742629,
-0.252179852923616,-0.249214914212792,-0.247407284024581,-0.245764278162907,
-0.243637165763318,-0.239112939019434,-0.233081432093515,-0.217008807348068,
-0.193131119263884,-0.190258726762178,-0.189132057512633,-0.188202674730495,
-0.187206091172668,-0.185595395376335,-0.179983992450302,-0.169604456258818,
-0.14603173450636,-0.135101689611372,-0.132051609445832,-0.130225387997182,
-0.128619156439092,-0.127247968759405,-0.125306358799174,-0.122357382842953,
-0.116860991140866,-0.103052857908684,-0.0826668163600495,-0.0743661800669981,
-0.0724865950543069,-0.0714196619645263,-0.0705102806790766,-0.069319195194738,
-0.066774601339198,-0.0633212231158481,-0.0542433421583409,-0.0283444858439824,
-0.0179670642535147,-0.0148615777933429,-0.0130232913170418,-0.011420793302306,
-0.00984244810923627,-0.00783663028624213,-0.000340145515886172),
 .UNSPECIFIED.);
#277=B_SPLINE_CURVE_WITH_KNOTS('',3,(#30181,#30182,#30183,#30184,#30185,
#30186,#30187,#30188,#30189,#30190,#30191,#30192,#30193,#30194,#30195,#30196,
#30197,#30198,#30199,#30200,#30201,#30202,#30203,#30204,#30205,#30206,#30207,
#30208,#30209,#30210,#30211,#30212,#30213,#30214,#30215,#30216,#30217,#30218,
#30219,#30220,#30221,#30222,#30223,#30224,#30225,#30226,#30227,#30228,#30229,
#30230,#30231,#30232,#30233,#30234,#30235,#30236,#30237,#30238,#30239,#30240,
#30241,#30242,#30243,#30244,#30245,#30246,#30247,#30248,#30249,#30250,#30251,
#30252,#30253,#30254,#30255,#30256,#30257,#30258,#30259,#30260),
 .UNSPECIFIED.,.F.,.F.,(4,2,2,2,2,2,2,2,2,2,2,2,2,2,2,2,2,2,2,2,2,2,2,2,
2,2,2,2,2,2,2,2,2,2,2,2,2,2,2,4),(-1.48436245928363,-1.45697626582871,-1.44145867048246,
-1.43936947323549,-1.43826910742382,-1.43735431844207,-1.43620305700907,
-1.43437710222971,-1.42388697285354,-1.3964930501114,-1.3885998090499,-1.38480948759865,
-1.38252355478692,-1.38047273681414,-1.38045595817035,-1.38043776423287,
-1.38041799710493,-1.38039647477197,-1.37882236344308,-1.37701828969799,
-1.37406890358588,-1.36415202553159,-1.33355391205358,-1.32705412617481,
-1.3229770998334,-1.32154247853527,-1.32058429591438,-1.319728723641,-1.31855869256389,
-1.31559897714232,-1.29451507063247,-1.27661520431747,-1.27019472471291,
-1.26544729604828,-1.26327930921085,-1.26163081676943,-1.25984272115395,
-1.25696712739865,-1.2477287299737,-1.24280763943444),.UNSPECIFIED.);
#278=B_SPLINE_CURVE_WITH_KNOTS('',3,(#30261,#30262,#30263,#30264,#30265,
#30266,#30267,#30268,#30269,#30270,#30271,#30272,#30273,#30274,#30275,#30276,
#30277,#30278,#30279,#30280,#30281,#30282,#30283,#30284,#30285,#30286,#30287,
#30288,#30289,#30290,#30291,#30292,#30293,#30294,#30295,#30296,#30297,#30298,
#30299,#30300,#30301,#30302,#30303,#30304,#30305,#30306,#30307,#30308,#30309,
#30310,#30311,#30312,#30313,#30314,#30315,#30316,#30317,#30318,#30319,#30320,
#30321,#30322,#30323,#30324,#30325,#30326,#30327,#30328,#30329,#30330,#30331,
#30332,#30333,#30334,#30335,#30336,#30337,#30338,#30339,#30340,#30341,#30342,
#30343,#30344,#30345,#30346,#30347,#30348,#30349,#30350,#30351,#30352,#30353,
#30354,#30355,#30356,#30357,#30358,#30359,#30360,#30361,#30362,#30363,#30364,
#30365,#30366,#30367,#30368,#30369,#30370,#30371,#30372,#30373,#30374,#30375,
#30376,#30377,#30378,#30379,#30380,#30381,#30382,#30383,#30384,#30385,#30386,
#30387,#30388,#30389,#30390,#30391,#30392,#30393,#30394,#30395,#30396,#30397,
#30398,#30399,#30400,#30401,#30402,#30403,#30404,#30405,#30406,#30407,#30408,
#30409,#30410,#30411,#30412,#30413,#30414,#30415,#30416,#30417,#30418,#30419,
#30420,#30421,#30422,#30423,#30424,#30425,#30426,#30427,#30428,#30429,#30430,
#30431,#30432,#30433,#30434,#30435,#30436,#30437,#30438,#30439,#30440,#30441,
#30442,#30443,#30444,#30445,#30446,#30447,#30448,#30449,#30450,#30451,#30452,
#30453,#30454,#30455,#30456,#30457,#30458,#30459,#30460,#30461,#30462,#30463,
#30464,#30465,#30466,#30467,#30468,#30469,#30470,#30471,#30472,#30473,#30474,
#30475,#30476,#30477,#30478),.UNSPECIFIED.,.F.,.F.,(4,2,2,2,2,2,2,2,2,2,
2,2,2,2,2,2,2,2,2,2,2,2,2,2,2,2,2,2,2,2,2,2,2,2,2,2,2,2,2,2,2,2,2,2,2,2,
2,2,2,2,2,2,2,2,2,2,2,2,2,2,2,2,2,2,2,2,2,2,2,2,2,2,2,2,2,2,2,2,2,2,2,2,
2,2,2,2,2,2,2,2,2,2,2,2,2,2,2,2,2,2,2,2,2,2,2,2,2,2,4),(-0.984002691704062,
-0.983265579879282,-0.982115101342455,-0.98029188872968,-0.969873114741405,
-0.961395403523032,-0.946982485815175,-0.930941305467715,-0.927684090046827,
-0.925812929079602,-0.924180694436495,-0.922158507690352,-0.919034695475286,
-0.896334175187465,-0.878930388345964,-0.872776257329012,-0.868855926680461,
-0.867442519897269,-0.866488717189068,-0.865629399334593,-0.864444554557963,
-0.86142944006154,-0.843454637902599,-0.823316440839283,-0.812986537088207,
-0.810103407345437,-0.808313624475316,-0.806665581652403,-0.804537641222769,
-0.799883576699916,-0.776084945864894,-0.759679675084305,-0.754744262178868,
-0.751409009640127,-0.750081698988863,-0.749144596367316,-0.748266105096901,
-0.74675164702973,-0.742438018774673,-0.735211431508296,-0.719037524177743,
-0.696844320877178,-0.693707727904646,-0.69168164615558,-0.690049115134306,
-0.68818073020362,-0.684936415094689,-0.669173484735883,-0.645679776641144,
-0.635501171275532,-0.63368753033417,-0.63253991242042,-0.631625155715052,
-0.630521380238969,-0.628416287372753,-0.611981641479028,-0.585024778655133,
-0.577914827331452,-0.57530161156218,-0.573742995230213,-0.572089607893275,
-0.569888924856837,-0.564958501340524,-0.558211733620303,-0.538633053837819,
-0.53801465694927,-0.519887524301152,-0.516872493203845,-0.515687652933693,
-0.514828334885846,-0.513874517320948,-0.512461073139244,-0.508540447608072,
-0.502386467179895,-0.484997001677238,-0.462308755731776,-0.459185207759204,
-0.457163080613137,-0.455530834192337,-0.453659593727591,-0.450402077025643,
-0.434358342227161,-0.419932144090225,-0.411446058694533,-0.401023346719223,
-0.399199845278794,-0.398049278024558,-0.397134445485913,-0.39603331376506,
-0.393940738908263,-0.378241283270627,-0.353225142505801,-0.343972005043057,
-0.341094891854124,-0.339306468156209,-0.33765808637706,-0.335490854225948,
-0.330747639699413,-0.324333867464797,-0.306468546748124,-0.285300879846517,
-0.282343677369006,-0.281174033670358,-0.280318544594259,-0.279360204556625,
-0.277924931282514,-0.273843132786132,-0.267333664141669,-0.241916328248978),
 .UNSPECIFIED.);
#279=B_SPLINE_CURVE_WITH_KNOTS('',3,(#30483,#30484,#30485,#30486,#30487,
#30488,#30489,#30490,#30491,#30492,#30493,#30494,#30495,#30496,#30497,#30498,
#30499,#30500,#30501,#30502,#30503,#30504,#30505,#30506,#30507,#30508,#30509,
#30510,#30511,#30512,#30513,#30514,#30515,#30516,#30517,#30518,#30519,#30520,
#30521,#30522,#30523,#30524,#30525,#30526,#30527,#30528,#30529,#30530,#30531,
#30532,#30533,#30534,#30535,#30536,#30537,#30538,#30539,#30540,#30541,#30542,
#30543,#30544,#30545,#30546,#30547,#30548,#30549,#30550,#30551,#30552,#30553,
#30554,#30555,#30556,#30557,#30558,#30559,#30560,#30561,#30562,#30563,#30564,
#30565,#30566,#30567,#30568,#30569,#30570,#30571,#30572,#30573,#30574,#30575,
#30576,#30577,#30578,#30579,#30580,#30581,#30582,#30583,#30584,#30585,#30586,
#30587,#30588,#30589,#30590,#30591,#30592,#30593,#30594,#30595,#30596,#30597,
#30598,#30599,#30600,#30601,#30602,#30603,#30604,#30605,#30606,#30607,#30608,
#30609,#30610,#30611,#30612,#30613,#30614,#30615,#30616,#30617,#30618,#30619,
#30620,#30621,#30622,#30623,#30624,#30625,#30626,#30627,#30628,#30629,#30630,
#30631,#30632,#30633,#30634,#30635,#30636,#30637,#30638,#30639,#30640,#30641,
#30642,#30643,#30644,#30645,#30646,#30647,#30648,#30649,#30650,#30651,#30652,
#30653,#30654,#30655,#30656,#30657,#30658,#30659,#30660,#30661,#30662,#30663,
#30664,#30665,#30666,#30667,#30668,#30669,#30670,#30671,#30672,#30673,#30674,
#30675,#30676,#30677,#30678,#30679,#30680,#30681,#30682,#30683,#30684,#30685,
#30686,#30687,#30688,#30689,#30690,#30691,#30692,#30693,#30694),
 .UNSPECIFIED.,.F.,.F.,(4,2,2,2,2,2,2,2,2,2,2,2,2,2,2,2,2,2,2,2,2,2,2,2,
2,2,2,2,2,2,2,2,2,2,2,2,2,2,2,2,2,2,2,2,2,2,2,2,2,2,2,2,2,2,2,2,2,2,2,2,
2,2,2,2,2,2,2,2,2,2,2,2,2,2,2,2,2,2,2,2,2,2,2,2,2,2,2,2,2,2,2,2,2,2,2,2,
2,2,2,2,2,2,2,2,2,4),(-1.24301555874646,-1.24280678210364,-1.24164937253616,
-1.23879642287787,-1.21583894977737,-1.20211326195524,-1.19034727950917,
-1.18734594005223,-1.18553030458148,-1.18388911289608,-1.18177713532705,
-1.17733409199837,-1.14954091908435,-1.13074392557291,-1.12818555667396,
-1.12699181497948,-1.12608210959619,-1.12501679355969,-1.12314456580738,
-1.11495676763724,-1.08271293902672,-1.07610667431467,-1.07125435240713,
-1.06906745881062,-1.06741610561402,-1.06563599387225,-1.06279748095302,
-1.0539173283568,-1.02552264243608,-1.0167492763692,-1.01337188112954,-1.01087075703067,
-1.00968788531127,-1.00877091908418,-1.00769479847151,-1.00577480994069,
-0.996812153231707,-0.976921462576252,-0.959710502782217,-0.954263975461164,
-0.951975402469816,-0.950307410444432,-0.948771156501619,-0.946681412061269,
-0.942520268426617,-0.917613676933456,-0.909454695141724,-0.89660817274771,
-0.893783358840923,-0.892541033383309,-0.891617461381184,-0.890577836607942,
-0.888772343503266,-0.881782246024147,-0.848334195570448,-0.841642044160709,
-0.836741667048819,-0.834546302006329,-0.832893730206289,-0.831333541959309,
-0.828712057001917,-0.821543117196986,-0.791253015809147,-0.782295507970897,
-0.778872052174502,-0.77634465718312,-0.775156808162071,-0.77424772480152,
-0.773178553436826,-0.771289189757746,-0.762838915587905,-0.742576682293863,
-0.722126792506872,-0.718994879402654,-0.716970169060304,-0.715337670778208,
-0.713468147743128,-0.710218810167517,-0.694351792420643,-0.66986831634356,
-0.660694620291853,-0.658762777639333,-0.657683982342627,-0.656767307407488,
-0.655588137459173,-0.653106390464633,-0.637841737676232,-0.612351866017475,
-0.603638537489341,-0.600820966941319,-0.599045356300897,-0.597392264764845,
-0.595194219024158,-0.590279348572559,-0.583560605660456,-0.564133031249619,
-0.54517834487597,-0.542167968185322,-0.540983841148447,-0.54012465641764,
-0.539170519261211,-0.537755797621785,-0.533826429388241,-0.52765353779518,
-0.510284232297328,-0.500846823737344),.UNSPECIFIED.);
#280=B_SPLINE_CURVE_WITH_KNOTS('',3,(#30696,#30697,#30698,#30699,#30700,
#30701,#30702,#30703,#30704,#30705,#30706,#30707,#30708,#30709,#30710,#30711,
#30712,#30713,#30714,#30715,#30716,#30717,#30718,#30719,#30720,#30721,#30722,
#30723,#30724,#30725,#30726,#30727,#30728,#30729,#30730,#30731,#30732,#30733,
#30734,#30735,#30736,#30737,#30738,#30739,#30740,#30741,#30742,#30743,#30744,
#30745,#30746,#30747,#30748,#30749,#30750,#30751,#30752,#30753,#30754,#30755,
#30756,#30757,#30758,#30759,#30760,#30761,#30762,#30763,#30764,#30765,#30766,
#30767,#30768,#30769,#30770,#30771,#30772,#30773),.UNSPECIFIED.,.F.,.F.,
(4,2,2,2,2,2,2,2,2,2,2,2,2,2,2,2,2,2,2,2,2,2,2,2,2,2,2,2,2,2,2,2,2,2,2,
2,2,2,4),(-0.241916328248978,-0.236562051352221,-0.226813709406645,-0.223883087469065,
-0.222083046533686,-0.220438218608943,-0.218296264316374,-0.213691301802682,
-0.207519669427203,-0.190808523118788,-0.167904394656517,-0.165048232361707,
-0.16389033286731,-0.162953050000126,-0.161970043329616,-0.160420648258423,
-0.155396650676668,-0.146618744887094,-0.119029162039518,-0.109535578023307,
-0.10661954439565,-0.104822703424011,-0.103247809715307,-0.103229170337593,
-0.103212052745656,-0.103196304164034,-0.101141341876507,-0.0988529194085211,
-0.0950564235044132,-0.0871442297293138,-0.0595982870658473,-0.0492481992942097,
-0.0474276568445735,-0.0462779936179891,-0.0453632141980915,-0.0442613455262378,
-0.0421651843025551,-0.0262630380286178,-0.0003407087586844),
 .UNSPECIFIED.);
#281=B_SPLINE_CURVE_WITH_KNOTS('',3,(#30774,#30775,#30776,#30777,#30778,
#30779,#30780,#30781,#30782,#30783,#30784,#30785,#30786,#30787,#30788,#30789,
#30790,#30791,#30792,#30793,#30794,#30795,#30796,#30797,#30798,#30799,#30800,
#30801,#30802,#30803,#30804,#30805,#30806,#30807,#30808,#30809,#30810,#30811,
#30812,#30813,#30814,#30815,#30816,#30817,#30818,#30819,#30820,#30821,#30822,
#30823,#30824,#30825,#30826,#30827,#30828,#30829,#30830,#30831,#30832,#30833,
#30834,#30835,#30836,#30837,#30838,#30839,#30840,#30841,#30842,#30843,#30844,
#30845,#30846,#30847,#30848,#30849,#30850,#30851,#30852,#30853,#30854,#30855,
#30856,#30857,#30858,#30859,#30860,#30861,#30862,#30863,#30864,#30865,#30866,
#30867,#30868,#30869,#30870,#30871,#30872,#30873,#30874,#30875,#30876,#30877,
#30878,#30879,#30880,#30881,#30882,#30883,#30884,#30885,#30886,#30887,#30888,
#30889,#30890,#30891,#30892,#30893,#30894,#30895,#30896,#30897,#30898,#30899,
#30900,#30901,#30902,#30903,#30904,#30905,#30906,#30907,#30908,#30909,#30910,
#30911,#30912,#30913,#30914,#30915,#30916,#30917,#30918,#30919,#30920,#30921,
#30922,#30923,#30924,#30925,#30926,#30927,#30928,#30929,#30930,#30931,#30932,
#30933,#30934,#30935,#30936,#30937,#30938,#30939),.UNSPECIFIED.,.F.,.F.,
(4,2,2,2,2,2,2,2,2,2,2,2,2,2,2,2,2,2,2,2,2,2,2,2,2,2,2,2,2,2,2,2,2,2,2,
2,2,2,2,2,2,2,2,2,2,2,2,2,2,2,2,2,2,2,2,2,2,2,2,2,2,2,2,2,2,2,2,2,2,2,2,
2,2,2,2,2,2,2,2,2,2,2,4),(-1.48419118738283,-1.47921164972554,-1.47564836502954,
-1.47364501573966,-1.47206793642528,-1.47046570329038,-1.46862719724292,
-1.46551799142764,-1.45411967840977,-1.42385030441413,-1.41826632819307,
-1.4146135825172,-1.41323851531508,-1.41229269107301,-1.41142619362586,
-1.40997201289101,-1.40607144333268,-1.37193939764168,-1.36349629958902,
-1.3595268825577,-1.35629775870598,-1.35445321303051,-1.35442928284637,
-1.35439733448367,-1.3543547378575,-1.35429804700801,-1.35276370461461,
-1.35074218620048,-1.34761882012523,-1.32493705492615,-1.307552352111,-1.30139141264108,
-1.29746850112217,-1.29605517174715,-1.29510171406355,-1.29424293662532,
-1.29305912831267,-1.29004821714032,-1.27216274147199,-1.2519708500577,
-1.24162853439811,-1.23874527283915,-1.23695603791654,-1.23530892028595,
-1.23318276435052,-1.22853504276312,-1.20458170028576,-1.19065441478453,
-1.18431063867901,-1.18030437578359,-1.17887965722658,-1.17792383865088,
-1.17706707932346,-1.17589128006043,-1.17292839237909,-1.15217302071374,
-1.15091052317974,-1.13371420660334,-1.12744023820528,-1.12277666137749,
-1.12062448318291,-1.11897881018088,-1.1171847492777,-1.11427941380768,
-1.10476046252644,-1.07708845402743,-1.06836584945626,-1.06336422736914,
-1.06181765189496,-1.06083550510258,-1.05989823474671,-1.0587395173517,
-1.05587718506041,-1.03313573509099,-1.01634725762738,-1.01015987187919,
-1.00554580923614,-1.00340262046433,-1.00175808269149,-0.999959585418396,
-0.997034259152756,-0.987329249751594,-0.983859778380464),.UNSPECIFIED.);
#282=B_SPLINE_CURVE_WITH_KNOTS('',3,(#30945,#30946,#30947,#30948,#30949,
#30950,#30951,#30952,#30953,#30954,#30955,#30956,#30957,#30958,#30959,#30960,
#30961,#30962,#30963,#30964,#30965,#30966,#30967,#30968,#30969,#30970,#30971,
#30972,#30973,#30974,#30975,#30976,#30977,#30978,#30979,#30980,#30981,#30982,
#30983,#30984,#30985,#30986,#30987,#30988,#30989,#30990,#30991,#30992,#30993,
#30994,#30995,#30996,#30997,#30998,#30999,#31000,#31001,#31002,#31003,#31004,
#31005,#31006,#31007,#31008,#31009,#31010,#31011,#31012,#31013,#31014,#31015,
#31016,#31017,#31018,#31019,#31020,#31021,#31022,#31023,#31024,#31025,#31026,
#31027,#31028,#31029,#31030,#31031,#31032,#31033,#31034,#31035,#31036,#31037,
#31038,#31039,#31040,#31041,#31042,#31043,#31044,#31045,#31046,#31047,#31048,
#31049,#31050,#31051,#31052,#31053,#31054,#31055,#31056,#31057,#31058,#31059,
#31060,#31061,#31062,#31063,#31064,#31065,#31066,#31067,#31068,#31069,#31070,
#31071,#31072,#31073,#31074,#31075,#31076,#31077,#31078,#31079,#31080,#31081,
#31082),.UNSPECIFIED.,.F.,.F.,(4,2,2,2,2,2,2,2,2,2,2,2,2,2,2,2,2,2,2,2,
2,2,2,2,2,2,2,2,2,2,2,2,2,2,2,2,2,2,2,2,2,2,2,2,2,2,2,2,2,2,2,2,2,2,2,2,
2,2,2,2,2,2,2,2,2,2,2,2,4),(-0.500851044544667,-0.470894244201872,-0.465649373246299,
-0.464016774608514,-0.463015383174412,-0.462077864007863,-0.460748168974234,
-0.457397540441704,-0.452431991446596,-0.435838474650016,-0.412319264901858,
-0.407661000237684,-0.405532331804943,-0.403884202026082,-0.402094800157889,
-0.399213339085658,-0.388902201358566,-0.368830641023063,-0.350748574800594,
-0.347731367777153,-0.346546169047475,-0.345686760952296,-0.344733042471823,
-0.343320078712556,-0.339402918202136,-0.333256418499153,-0.315861217289976,
-0.293171659297553,-0.290048210487714,-0.288026114714526,-0.286393869772687,
-0.284522602736839,-0.281264959620612,-0.265217698604029,-0.250796482663248,
-0.242314702381025,-0.231891666712883,-0.230068172840124,-0.228917608321084,
-0.228002775010712,-0.226901631551511,-0.224808995620849,-0.209104479502421,
-0.184073770533595,-0.174841177479061,-0.171966249281754,-0.170178303133175,
-0.168529769197121,-0.166361465738672,-0.161612298021905,-0.155187986383279,
-0.137270113651277,-0.116185846134633,-0.113234634624075,-0.112060477173242,
-0.11120386541438,-0.110270629096301,-0.108945310054627,-0.107372092485822,
-0.104486831862825,-0.0720408047135209,-0.0582880063787682,-0.0550768717875946,
-0.0531972605332543,-0.0515659551181552,-0.0495555746376407,-0.0456326536754258,
-0.0246874792708936,-0.000340715134129704),.UNSPECIFIED.);
#283=B_SPLINE_CURVE_WITH_KNOTS('',3,(#31083,#31084,#31085,#31086,#31087,
#31088,#31089,#31090,#31091,#31092,#31093,#31094,#31095,#31096,#31097,#31098,
#31099,#31100,#31101,#31102,#31103,#31104,#31105,#31106,#31107,#31108,#31109,
#31110,#31111,#31112,#31113,#31114,#31115,#31116,#31117,#31118,#31119,#31120,
#31121,#31122,#31123,#31124,#31125,#31126,#31127,#31128,#31129,#31130,#31131,
#31132,#31133,#31134,#31135,#31136,#31137,#31138,#31139,#31140,#31141,#31142,
#31143,#31144,#31145,#31146,#31147,#31148,#31149,#31150,#31151,#31152,#31153,
#31154,#31155,#31156,#31157,#31158,#31159,#31160),.UNSPECIFIED.,.F.,.F.,
(4,2,2,2,2,2,2,2,2,2,2,2,2,2,2,2,2,2,2,2,2,2,2,2,2,2,2,2,2,2,2,2,2,2,2,
2,2,2,4),(-1.48461435640971,-1.48095567937514,-1.47974240158655,-1.47883059476506,
-1.47794354751819,-1.47691361604675,-1.47515157681881,-1.46865992468335,
-1.44929217834935,-1.42650225485955,-1.42256245148621,-1.42054875108082,
-1.41891732349596,-1.41704041715532,-1.41384087999495,-1.400282318118,-1.36771184950226,
-1.36476891410112,-1.36317400325097,-1.36180480368685,-1.3608695765384,
-1.36001083242486,-1.35882820169348,-1.35582634070192,-1.33871521949899,
-1.3179113197633,-1.31094598563399,-1.30589405601771,-1.30367217148542,
-1.30201548127954,-1.30024947393576,-1.29747573874274,-1.28913522682116,
-1.26011876050653,-1.25131260692672,-1.24627803778347,-1.24472735988065,
-1.24374400664924,-1.24301555874646),.UNSPECIFIED.);
#284=B_SPLINE_CURVE_WITH_KNOTS('',3,(#31161,#31162,#31163,#31164,#31165,
#31166,#31167,#31168,#31169,#31170,#31171,#31172,#31173,#31174,#31175,#31176,
#31177,#31178,#31179,#31180,#31181,#31182,#31183,#31184,#31185,#31186,#31187,
#31188,#31189,#31190,#31191,#31192,#31193,#31194,#31195,#31196,#31197,#31198,
#31199,#31200,#31201,#31202,#31203,#31204,#31205,#31206,#31207,#31208,#31209,
#31210,#31211,#31212,#31213,#31214,#31215,#31216,#31217,#31218,#31219,#31220,
#31221,#31222,#31223,#31224,#31225,#31226,#31227,#31228,#31229,#31230,#31231,
#31232,#31233,#31234,#31235,#31236,#31237,#31238,#31239,#31240,#31241,#31242,
#31243,#31244,#31245,#31246,#31247,#31248,#31249,#31250,#31251,#31252,#31253,
#31254,#31255,#31256,#31257,#31258,#31259,#31260,#31261,#31262,#31263,#31264,
#31265,#31266,#31267,#31268,#31269,#31270,#31271,#31272,#31273,#31274,#31275,
#31276,#31277,#31278,#31279,#31280,#31281,#31282,#31283,#31284,#31285,#31286,
#31287,#31288,#31289,#31290,#31291,#31292,#31293,#31294,#31295,#31296,#31297,
#31298,#31299,#31300,#31301,#31302,#31303,#31304,#31305,#31306,#31307,#31308,
#31309,#31310,#31311,#31312,#31313,#31314,#31315,#31316,#31317,#31318,#31319,
#31320,#31321,#31322,#31323,#31324,#31325,#31326,#31327,#31328,#31329,#31330,
#31331,#31332,#31333,#31334,#31335,#31336,#31337,#31338,#31339,#31340,#31341,
#31342,#31343,#31344,#31345,#31346,#31347,#31348,#31349,#31350,#31351,#31352,
#31353,#31354,#31355,#31356,#31357,#31358,#31359,#31360,#31361,#31362,#31363,
#31364,#31365,#31366),.UNSPECIFIED.,.F.,.F.,(4,2,2,2,2,2,2,2,2,2,2,2,2,
2,2,2,2,2,2,2,2,2,2,2,2,2,2,2,2,2,2,2,2,2,2,2,2,2,2,2,2,2,2,2,2,2,2,2,2,
2,2,2,2,2,2,2,2,2,2,2,2,2,2,2,2,2,2,2,2,2,2,2,2,2,2,2,2,2,2,2,2,2,2,2,2,
2,2,2,2,2,2,2,2,2,2,2,2,2,2,2,2,2,4),(-0.983859778380464,-0.956504322260066,
-0.949990619817789,-0.945907656089805,-0.944472491112579,-0.94351437847939,
-0.942659206983767,-0.941490152443025,-0.938537859202834,-0.917332862261902,
-0.899520681043165,-0.893118682458089,-0.888382026189533,-0.886216351454495,
-0.884568565581389,-0.8827802145083,-0.87990195187403,-0.870633334570441,
-0.845622578781929,-0.829924881779486,-0.827832617921649,-0.826731724218592,
-0.825817128910256,-0.824666915160807,-0.822844094873349,-0.812426562834528,
-0.803964432365397,-0.789576630597031,-0.77350823421958,-0.770250378464962,
-0.768379364120978,-0.766747558273291,-0.764726292123414,-0.761604649487132,
-0.742185020241834,-0.726888864122854,-0.712777138059242,-0.710861168394497,
-0.709683061650375,-0.708766760155919,-0.707687869288201,-0.705699914213867,
-0.693932804271416,-0.670440108515074,-0.656315300476018,-0.653083468215382,
-0.651199366351649,-0.649731815794533,-0.647799964512289,-0.644256897049762,
-0.619263397012194,-0.596808923862333,-0.593921997393029,-0.592758904546354,
-0.591820344534971,-0.590839596829148,-0.589300015442163,-0.584362923889726,
-0.575808244920175,-0.549698234382592,-0.538680644571589,-0.535623394671848,
-0.533795924912142,-0.532157860650581,-0.530069022833586,-0.525745814953144,
-0.508990969644128,-0.494870477813161,-0.478357825960762,-0.476423050565638,
-0.475239368364634,-0.474322614561491,-0.473247733329158,-0.471278556459339,
-0.460011379886193,-0.444199836384678,-0.422254400401983,-0.41911064692152,
-0.417082675807384,-0.415450389596015,-0.413584213706913,-0.410348705206556,
-0.394754795609124,-0.372716756975284,-0.367134511753262,-0.360497204350288,
-0.358722776699775,-0.357690189049464,-0.35676509042552,-0.355510117523619,
-0.352611700451612,-0.339054781104996,-0.335061952140706,-0.306431703458366,
-0.302076518480185,-0.299981611743217,-0.298342899413162,-0.296518943141558,
-0.293477681225447,-0.281159033943898,-0.25118057349547,-0.243408795535128,
-0.241907325797883),.UNSPECIFIED.);
#285=B_SPLINE_CURVE_WITH_KNOTS('',3,(#31371,#31372,#31373,#31374,#31375,
#31376,#31377,#31378,#31379,#31380,#31381,#31382,#31383,#31384,#31385,#31386,
#31387,#31388,#31389,#31390,#31391,#31392,#31393,#31394,#31395,#31396,#31397,
#31398,#31399,#31400,#31401,#31402,#31403,#31404,#31405,#31406,#31407,#31408,
#31409,#31410,#31411,#31412,#31413,#31414,#31415,#31416,#31417,#31418,#31419,
#31420,#31421,#31422,#31423,#31424,#31425,#31426,#31427,#31428,#31429,#31430,
#31431,#31432,#31433,#31434,#31435,#31436,#31437,#31438,#31439,#31440,#31441,
#31442,#31443,#31444,#31445,#31446,#31447,#31448,#31449,#31450,#31451,#31452,
#31453,#31454,#31455,#31456,#31457,#31458,#31459,#31460,#31461,#31462,#31463,
#31464,#31465,#31466,#31467,#31468,#31469,#31470,#31471,#31472,#31473,#31474,
#31475,#31476,#31477,#31478,#31479,#31480,#31481,#31482,#31483,#31484,#31485,
#31486,#31487,#31488,#31489,#31490,#31491,#31492,#31493,#31494,#31495,#31496,
#31497,#31498,#31499,#31500,#31501,#31502,#31503,#31504,#31505,#31506,#31507,
#31508,#31509,#31510,#31511,#31512,#31513,#31514,#31515,#31516,#31517,#31518,
#31519,#31520,#31521,#31522,#31523,#31524,#31525,#31526,#31527,#31528,#31529,
#31530,#31531,#31532,#31533,#31534,#31535,#31536,#31537,#31538,#31539,#31540,
#31541,#31542,#31543,#31544,#31545,#31546,#31547,#31548,#31549,#31550,#31551,
#31552,#31553,#31554,#31555,#31556,#31557,#31558,#31559,#31560,#31561,#31562,
#31563,#31564,#31565,#31566,#31567,#31568,#31569,#31570,#31571,#31572,#31573,
#31574,#31575,#31576,#31577,#31578,#31579,#31580,#31581,#31582,#31583,#31584,
#31585,#31586,#31587,#31588,#31589,#31590),.UNSPECIFIED.,.F.,.F.,(4,2,2,
2,2,2,2,2,2,2,2,2,2,2,2,2,2,2,2,2,2,2,2,2,2,2,2,2,2,2,2,2,2,2,2,2,2,2,2,
2,2,2,2,2,2,2,2,2,2,2,2,2,2,2,2,2,2,2,2,2,2,2,2,2,2,2,2,2,2,2,2,2,2,2,2,
2,2,2,2,2,2,2,2,2,2,2,2,2,2,2,2,2,2,2,2,2,2,2,2,2,2,2,2,2,2,2,2,2,2,4),
(-1.2427255514666,-1.23060639702225,-1.22734995878737,-1.22547924039624,
-1.22384738677346,-1.2218256634024,-1.21870254924936,-1.19599880834317,
-1.17858368190725,-1.17244529391067,-1.16853251114878,-1.16712041934795,
-1.16616709789873,-1.16530792723202,-1.1641228860977,-1.16110513657904,
-1.14308012134878,-1.12299513858127,-1.11268157357094,-1.10980059671523,
-1.10801169641925,-1.10636416351028,-1.1042364574599,-1.09958115577374,
-1.07591712084999,-1.06177958613118,-1.05538720100713,-1.05135878925255,
-1.04993095819828,-1.04897439716279,-1.04811792428216,-1.04694382727023,
-1.04399201665834,-1.0229712970852,-1.00503526460183,-0.998607946502903,
-0.993856820084637,-0.991688375720636,-0.990040030279437,-0.988252573869962,
-0.985379064781073,-0.976157428830489,-0.951108805714289,-0.93539687307613,
-0.933304157500287,-0.932203074612696,-0.931288375468315,-0.930138077140012,
-0.928315145539022,-0.91789723601422,-0.909425950442992,-0.89502035921056,
-0.878978888820759,-0.875722134865666,-0.87385127700113,-0.872219326820631,
-0.870197516313012,-0.867074326196596,-0.844384905671827,-0.826995860488933,
-0.820833303343909,-0.816909327136579,-0.815495580962352,-0.814541831431272,
-0.813682779619426,-0.812498575102276,-0.80948655641407,-0.790609908013162,
-0.771155266060003,-0.764432591104257,-0.759515363871419,-0.757317245885591,
-0.755664477296493,-0.753889572141093,-0.751073898163996,-0.742373361690178,
-0.726899212117861,-0.702037861028191,-0.6992589620858,-0.698038179503742,
-0.697114789673177,-0.696075504625279,-0.694270921341789,-0.686242128345383,
-0.666913550870398,-0.644940258253765,-0.641801216129891,-0.639774546274086,
-0.638142181373455,-0.636274683570456,-0.633033700117319,-0.617332040787526,
-0.594373451152823,-0.589357020035347,-0.583119770253274,-0.581382332131788,
-0.580357811938072,-0.579430029637448,-0.578157702095767,-0.575158706713002,
-0.570875962911844,-0.558070181845823,-0.529054678352759,-0.524741928417015,
-0.522654986779741,-0.521017005459846,-0.519188171415971,-0.516125144550386,
-0.503498200677261,-0.500851044544667),.UNSPECIFIED.);
#286=B_SPLINE_CURVE_WITH_KNOTS('',3,(#31592,#31593,#31594,#31595,#31596,
#31597,#31598,#31599,#31600,#31601,#31602,#31603,#31604,#31605,#31606,#31607,
#31608,#31609,#31610,#31611,#31612,#31613,#31614,#31615,#31616,#31617,#31618,
#31619,#31620,#31621,#31622,#31623,#31624,#31625,#31626,#31627,#31628,#31629,
#31630,#31631,#31632,#31633,#31634,#31635,#31636,#31637,#31638,#31639,#31640,
#31641,#31642,#31643,#31644,#31645,#31646,#31647,#31648,#31649,#31650,#31651,
#31652,#31653,#31654,#31655,#31656,#31657,#31658,#31659,#31660,#31661,#31662,
#31663,#31664,#31665,#31666,#31667,#31668,#31669,#31670,#31671,#31672,#31673,
#31674,#31675,#31676,#31677,#31678,#31679),.UNSPECIFIED.,.F.,.F.,(4,2,2,
2,2,2,2,2,2,2,2,2,2,2,2,2,2,2,2,2,2,2,2,2,2,2,2,2,2,2,2,2,2,2,2,2,2,2,2,
2,2,2,2,4),(-0.241907325797883,-0.241564736786382,-0.2405060295345,-0.239679017943203,
-0.238522152108265,-0.236154348097133,-0.233007704473341,-0.225126565777923,
-0.201723109279611,-0.187408074081491,-0.184165567342836,-0.182278938034591,
-0.180648332175155,-0.178647450960559,-0.174771021102985,-0.169825066938676,
-0.158111036262439,-0.144624591959884,-0.126640701292084,-0.124722421562707,
-0.123543586682625,-0.122644011424788,-0.121598200755175,-0.120466219902755,
-0.118697580026735,-0.115283174764137,-0.106361259804418,-0.0761777649382564,
-0.0689124259559693,-0.0662779636630842,-0.0647155665043315,-0.0630646866011098,
-0.0608784413088461,-0.0560277048481825,-0.0494229319742788,-0.0456307667643694,
-0.0142563478955802,-0.00858120041559184,-0.00690292372145922,-0.00589149484902674,
-0.00501412596607927,-0.00409312851683857,-0.00241291697315785,-0.000340185083165174),
 .UNSPECIFIED.);
#287=B_SPLINE_CURVE_WITH_KNOTS('',3,(#31680,#31681,#31682,#31683,#31684,
#31685,#31686,#31687,#31688,#31689,#31690,#31691,#31692,#31693,#31694,#31695,
#31696,#31697,#31698,#31699,#31700,#31701,#31702,#31703,#31704,#31705,#31706,
#31707,#31708,#31709,#31710,#31711,#31712,#31713,#31714,#31715,#31716,#31717,
#31718,#31719,#31720,#31721,#31722,#31723,#31724,#31725,#31726,#31727,#31728,
#31729,#31730,#31731,#31732,#31733,#31734,#31735,#31736,#31737,#31738,#31739,
#31740,#31741,#31742,#31743,#31744,#31745,#31746,#31747,#31748,#31749,#31750,
#31751,#31752,#31753,#31754,#31755,#31756,#31757,#31758,#31759,#31760,#31761,
#31762,#31763,#31764,#31765,#31766,#31767,#31768,#31769,#31770,#31771,#31772,
#31773,#31774,#31775,#31776,#31777,#31778,#31779,#31780,#31781,#31782,#31783,
#31784,#31785,#31786,#31787,#31788,#31789,#31790,#31791,#31792,#31793,#31794),
 .UNSPECIFIED.,.F.,.F.,(4,3,3,3,3,3,3,3,3,3,3,3,3,3,3,3,3,3,3,3,3,3,3,3,
3,3,3,3,3,3,3,3,3,3,3,3,3,3,4),(128.805298797903,128.92420180571,129.042936368382,
129.161556941574,129.280117790517,129.398763160983,129.517442871689,129.636361003745,
129.752144419847,129.876237071814,129.995823264793,130.115290605822,130.234691814404,
130.354079495645,130.47358802796,130.593169404387,130.71296572914,130.744885635581,
130.868978287548,130.988564594503,131.10803205027,131.227433374119,131.346821170921,
131.466329818357,131.585911309774,131.705707748165,131.737626851315,131.861719503282,
131.981305352592,132.100772351382,132.22017321981,132.339560563643,132.459068765062,
132.578649814039,132.698445819611,132.730368067049,132.850162222238,132.969754516053,
133.043121691919),.UNSPECIFIED.);
#288=B_SPLINE_CURVE_WITH_KNOTS('',3,(#31800,#31801,#31802,#31803,#31804,
#31805,#31806,#31807,#31808,#31809,#31810,#31811,#31812,#31813,#31814,#31815,
#31816,#31817,#31818,#31819,#31820,#31821,#31822,#31823,#31824,#31825,#31826,
#31827,#31828,#31829,#31830,#31831,#31832,#31833,#31834,#31835,#31836,#31837,
#31838,#31839,#31840,#31841,#31842,#31843,#31844,#31845,#31846,#31847,#31848,
#31849,#31850,#31851,#31852,#31853,#31854,#31855,#31856,#31857,#31858,#31859,
#31860,#31861,#31862,#31863,#31864,#31865,#31866,#31867,#31868,#31869,#31870,
#31871,#31872,#31873,#31874,#31875,#31876,#31877,#31878,#31879,#31880,#31881,
#31882,#31883,#31884,#31885,#31886,#31887,#31888,#31889,#31890,#31891,#31892,
#31893,#31894,#31895,#31896,#31897,#31898,#31899,#31900,#31901,#31902,#31903,
#31904,#31905,#31906,#31907,#31908,#31909,#31910,#31911),.UNSPECIFIED.,
 .F.,.F.,(4,3,3,3,3,3,3,3,3,3,3,3,3,3,3,3,3,3,3,3,3,3,3,3,3,3,3,3,3,3,3,
3,3,3,3,3,3,4),(135.088484104816,135.235319650575,135.372911768261,135.497004420228,
135.616613963295,135.736104467611,135.855528609251,135.974938949634,136.094469573001,
136.214072732833,136.33389017762,136.365652983995,136.489745635962,136.609357211818,
136.728850230044,136.848277355743,136.967691140023,137.087225850178,137.206833475805,
137.326655887354,137.358394199729,137.482486851696,137.601928623404,137.721251639095,
137.840508895953,137.959753276841,138.079120520349,138.198561623553,138.318220556655,
138.351135415463,138.472967083591,138.592769381413,138.712449797914,138.832060644392,
138.955492673417,139.075196120745,139.200492440618,139.325788760491),
 .UNSPECIFIED.);
#289=B_SPLINE_CURVE_WITH_KNOTS('',3,(#31912,#31913,#31914,#31915,#31916,
#31917,#31918,#31919,#31920,#31921,#31922,#31923,#31924,#31925,#31926,#31927,
#31928,#31929,#31930,#31931,#31932,#31933,#31934,#31935,#31936,#31937,#31938,
#31939,#31940,#31941,#31942,#31943,#31944,#31945,#31946,#31947,#31948,#31949,
#31950,#31951,#31952,#31953,#31954,#31955,#31956,#31957,#31958,#31959,#31960,
#31961,#31962,#31963,#31964,#31965,#31966,#31967,#31968,#31969,#31970,#31971,
#31972,#31973,#31974,#31975,#31976,#31977,#31978,#31979,#31980,#31981,#31982,
#31983,#31984,#31985),.UNSPECIFIED.,.F.,.F.,(4,2,2,2,2,2,2,2,2,2,2,2,2,
2,2,2,2,2,2,2,2,2,2,2,2,2,2,2,2,2,2,2,2,2,2,2,4),(-1.48433664459609,-1.46671782054178,
-1.46371943846842,-1.461758308634,-1.46019416291955,-1.45856476614673,-1.45668477152549,
-1.45346669170546,-1.43956052911776,-1.42476392374183,-1.41144205555522,
-1.40368120358948,-1.40189154794862,-1.40085624895909,-1.39993245513015,
-1.39870663663035,-1.39589864627127,-1.37133735902695,-1.35570646797292,
-1.34977485815692,-1.34534046054347,-1.34329373304463,-1.34164426587415,
-1.33985883508753,-1.336995700033,-1.32787579135332,-1.30275607210206,-1.28701833701235,
-1.28492474437849,-1.28382323918716,-1.28290836603037,-1.28175799058702,
-1.2799348673473,-1.26951253007453,-1.261048704623,-1.24664495753197,-1.2427255514666),
 .UNSPECIFIED.);
#290=B_SPLINE_CURVE_WITH_KNOTS('',3,(#31987,#31988,#31989,#31990,#31991,
#31992,#31993,#31994,#31995,#31996,#31997,#31998,#31999,#32000,#32001,#32002,
#32003,#32004,#32005,#32006,#32007,#32008,#32009,#32010,#32011,#32012,#32013,
#32014,#32015,#32016,#32017,#32018,#32019,#32020,#32021,#32022,#32023,#32024,
#32025,#32026,#32027,#32028,#32029,#32030,#32031,#32032,#32033,#32034,#32035,
#32036,#32037,#32038,#32039,#32040,#32041),.UNSPECIFIED.,.F.,.F.,(4,3,3,
3,3,3,3,3,3,3,3,3,3,3,3,3,3,3,4),(133.043121691919,133.16254457611,133.281931744498,
133.401423904568,133.520968990874,133.640744469938,133.723109282783,133.84720193475,
133.966788928961,134.086257075103,134.205659091046,134.325047580267,134.444556915418,
134.56413909254,134.683936206814,134.715850498517,134.851216151486,134.985568509351,
135.088484103636),.UNSPECIFIED.);
#291=B_SPLINE_CURVE_WITH_KNOTS('',3,(#32042,#32043,#32044,#32045,#32046,
#32047,#32048,#32049,#32050,#32051,#32052,#32053,#32054,#32055,#32056,#32057,
#32058,#32059,#32060,#32061,#32062,#32063,#32064,#32065,#32066,#32067,#32068,
#32069,#32070,#32071,#32072,#32073,#32074,#32075,#32076,#32077,#32078,#32079,
#32080,#32081,#32082,#32083,#32084,#32085,#32086,#32087,#32088,#32089,#32090,
#32091,#32092,#32093,#32094,#32095,#32096,#32097,#32098,#32099,#32100,#32101,
#32102,#32103,#32104,#32105,#32106,#32107,#32108,#32109,#32110,#32111,#32112,
#32113,#32114,#32115,#32116,#32117,#32118,#32119,#32120,#32121,#32122,#32123,
#32124,#32125,#32126,#32127,#32128,#32129,#32130,#32131,#32132,#32133,#32134,
#32135,#32136,#32137,#32138,#32139,#32140,#32141,#32142,#32143,#32144,#32145,
#32146,#32147,#32148,#32149,#32150,#32151,#32152,#32153,#32154,#32155,#32156,
#32157,#32158,#32159,#32160,#32161,#32162,#32163,#32164,#32165,#32166,#32167,
#32168,#32169,#32170,#32171,#32172,#32173,#32174,#32175,#32176,#32177,#32178,
#32179,#32180,#32181,#32182,#32183,#32184,#32185,#32186,#32187,#32188,#32189,
#32190,#32191,#32192,#32193,#32194,#32195),.UNSPECIFIED.,.F.,.F.,(4,2,2,
2,2,2,2,2,2,2,2,2,2,2,2,2,2,2,2,2,2,2,2,2,2,2,2,2,2,2,2,2,2,2,2,2,2,2,2,
2,2,2,2,2,2,2,2,2,2,2,2,2,2,2,2,2,2,2,2,2,2,2,2,2,2,2,2,2,2,2,2,2,2,2,2,
2,4),(0.500786432389318,0.512128357748242,0.515212285446151,0.517046105357922,
0.518520106997671,0.520519510482704,0.524386314514495,0.529315375315604,
0.540964201475301,0.559881492768139,0.562846546633378,0.572769307541564,
0.574567560361756,0.57571031546824,0.576624314654795,0.57773081720011,0.579852194656469,
0.597599957817087,0.627349344461373,0.631646249968152,0.633728953812867,
0.635365090787654,0.637193378608985,0.640259064057918,0.652953175769306,
0.686280538407828,0.690882046830322,0.692434278844384,0.693319577537061,
0.694251550172155,0.695550980788332,0.698712808466119,0.703307756442877,
0.717746353397341,0.744260486092286,0.748350882736053,0.750423186768318,
0.751955117939803,0.753626638816482,0.755935134568518,0.761504157214373,
0.782949708419264,0.805845372659464,0.808699585127555,0.8098573260419,0.810794755757872,
0.811777965195418,0.813328434968161,0.818362519764478,0.827168181138911,
0.855641342762716,0.864409188682483,0.867232411448932,0.869008841809705,
0.870627939153777,0.872750076516439,0.875104279531898,0.879064300347567,
0.88747727406923,0.921039827713324,0.925427952290645,0.926952410093915,
0.927832712943928,0.928768170478391,0.930087463870695,0.933373504830684,
0.938211794778996,0.954036446931215,0.968368149659771,0.979680459449246,
0.983222018779296,0.985345229338978,0.9869922044933,0.988519355524955,0.990278595138859,
0.992780135022167,1.00127085069662),.UNSPECIFIED.);
#292=B_SPLINE_CURVE_WITH_KNOTS('',3,(#32201,#32202,#32203,#32204,#32205,
#32206),.UNSPECIFIED.,.F.,.F.,(4,1,1,4),(-4.09202352044853,-3.97096486293603,
-2.97822364720202,-2.07364390538107),.UNSPECIFIED.);
#293=B_SPLINE_CURVE_WITH_KNOTS('',3,(#32209,#32210,#32211,#32212,#32213),
 .UNSPECIFIED.,.F.,.F.,(4,1,4),(0.,0.992741215733998,1.12274180646084),
 .UNSPECIFIED.);
#294=B_SPLINE_CURVE_WITH_KNOTS('',3,(#32218,#32219,#32220,#32221,#32222,
#32223,#32224,#32225,#32226,#32227),.UNSPECIFIED.,.F.,.F.,(4,1,1,1,1,1,
1,4),(-10.3752053909602,-9.92741215734008,-8.93467094160607,-7.94192972587206,
-6.94918851013805,-5.95644729440404,-4.96370607867004,-4.09202352044853),
 .UNSPECIFIED.);
#295=B_SPLINE_CURVE_WITH_KNOTS('',3,(#32228,#32229,#32230,#32231,#32232,
#32233,#32234,#32235,#32236,#32237,#32238,#32239,#32240,#32241,#32242,#32243,
#32244,#32245,#32246,#32247,#32248,#32249,#32250,#32251,#32252,#32253,#32254,
#32255,#32256,#32257,#32258,#32259,#32260,#32261,#32262,#32263,#32264,#32265,
#32266,#32267,#32268,#32269,#32270,#32271,#32272,#32273,#32274,#32275,#32276,
#32277,#32278,#32279,#32280,#32281,#32282,#32283,#32284,#32285,#32286,#32287,
#32288,#32289,#32290,#32291,#32292,#32293,#32294,#32295,#32296,#32297,#32298,
#32299,#32300,#32301,#32302,#32303,#32304,#32305,#32306,#32307,#32308,#32309,
#32310,#32311,#32312,#32313,#32314,#32315,#32316,#32317,#32318,#32319,#32320,
#32321,#32322,#32323,#32324,#32325,#32326,#32327,#32328,#32329,#32330,#32331,
#32332,#32333,#32334,#32335,#32336,#32337,#32338,#32339,#32340,#32341,#32342,
#32343,#32344,#32345,#32346,#32347,#32348,#32349,#32350,#32351,#32352,#32353,
#32354,#32355,#32356,#32357,#32358,#32359,#32360,#32361,#32362,#32363,#32364,
#32365,#32366,#32367,#32368,#32369,#32370,#32371,#32372,#32373,#32374,#32375,
#32376,#32377,#32378,#32379,#32380,#32381,#32382,#32383,#32384,#32385,#32386,
#32387,#32388,#32389,#32390,#32391,#32392,#32393,#32394,#32395,#32396,#32397,
#32398,#32399),.UNSPECIFIED.,.F.,.F.,(4,3,3,3,3,3,3,3,3,3,3,3,3,3,3,3,3,
3,3,3,3,3,3,3,3,3,3,3,3,3,3,3,3,3,3,3,3,3,3,3,3,3,3,3,3,3,3,3,3,3,3,3,3,
3,3,3,3,4),(1.12274180646084,1.23355937374209,1.34423918815353,1.45482944455971,
1.56537815734206,1.67601277927824,1.78668774769182,1.89757125282276,1.98548243146801,
2.09908269663091,2.21248030600278,2.32576514911402,2.43898180620018,2.55217475654608,
2.66546889339697,2.77881317901057,2.89236747726848,2.97822364720202,3.09188643018773,
3.20535340945894,3.31871176665814,3.43200594742818,3.54528030150624,3.65866123708271,
3.77209545052106,3.88574371923928,3.97096486293603,4.0843145896902,4.19745986938771,
4.31049148709486,4.4234544918255,4.536393830391,4.64943648022474,4.76253007371526,
4.87583814693796,4.96370607867004,5.07720989041121,5.19051208640097,5.30370223548262,
5.41682510052755,5.52992534434195,5.64312923773688,5.75638451459586,5.86985297185556,
5.95644729440405,6.06994635889941,6.18324442746533,6.29643083241813,6.40955034376972,
6.522647631939,6.63584921520513,6.74910253713155,6.86256965122693,6.94918851013806,
7.07058636504131,7.19168899525419,7.3123612953248,7.40592711324594),
 .UNSPECIFIED.);
#296=B_SPLINE_CURVE_WITH_KNOTS('',3,(#32404,#32405,#32406,#32407,#32408,
#32409,#32410,#32411,#32412,#32413,#32414,#32415,#32416,#32417,#32418,#32419,
#32420,#32421,#32422,#32423,#32424,#32425,#32426,#32427,#32428,#32429,#32430,
#32431,#32432,#32433,#32434,#32435,#32436,#32437,#32438,#32439,#32440,#32441,
#32442,#32443,#32444,#32445,#32446,#32447,#32448,#32449,#32450,#32451,#32452,
#32453,#32454,#32455,#32456,#32457,#32458,#32459,#32460,#32461,#32462,#32463,
#32464,#32465,#32466,#32467,#32468,#32469,#32470,#32471,#32472,#32473,#32474,
#32475,#32476,#32477,#32478,#32479,#32480,#32481,#32482,#32483,#32484,#32485,
#32486,#32487,#32488,#32489,#32490,#32491,#32492,#32493,#32494,#32495,#32496,
#32497,#32498,#32499,#32500,#32501,#32502,#32503,#32504,#32505,#32506,#32507,
#32508,#32509,#32510,#32511,#32512,#32513,#32514,#32515,#32516,#32517,#32518,
#32519,#32520,#32521,#32522,#32523,#32524,#32525,#32526,#32527,#32528,#32529,
#32530,#32531,#32532,#32533,#32534,#32535,#32536,#32537,#32538,#32539,#32540,
#32541,#32542,#32543,#32544,#32545,#32546,#32547,#32548,#32549,#32550,#32551,
#32552,#32553,#32554,#32555,#32556,#32557,#32558,#32559,#32560,#32561,#32562,
#32563,#32564,#32565,#32566,#32567,#32568,#32569,#32570,#32571,#32572,#32573,
#32574,#32575),.UNSPECIFIED.,.F.,.F.,(4,3,3,3,3,3,3,3,3,3,3,3,3,3,3,3,3,
3,3,3,3,3,3,3,3,3,3,3,3,3,3,3,3,3,3,3,3,3,3,3,3,3,3,3,3,3,3,3,3,3,3,3,3,
3,3,3,3,4),(-16.6583941342588,-16.5466839297704,-16.4350647570386,-16.3234895832408,
-16.2118304445513,-16.1001347697573,-15.9882254957626,-15.8838594517441,
-15.7703802606902,-15.6571027547231,-15.5439373184522,-15.4308391434175,
-15.3177635212612,-15.2045839431989,-15.0913528487032,-14.9779080503663,
-14.8911182360101,-14.7776389385898,-14.6643613248847,-14.5511957801209,
-14.4380974960384,-14.325021764479,-14.2118420773477,-14.098610873801,-13.985165967815,
-13.8983770202761,-13.7848981557516,-13.671620974954,-13.5584558627794,
-13.4453580102098,-13.3322827083287,-13.2191034446402,-13.1058726617254,
-12.9924281665408,-12.9056358045421,-12.7921564211267,-12.6788787267111,
-12.5657131045183,-12.4526147463851,-12.3395389442535,-12.2263591924163,
-12.1131279273202,-11.9996829656535,-11.9128945888081,-11.7994146477071,
-11.6861363842348,-11.5729701864831,-11.4598712473816,-11.3467948599574,
-11.2336145209221,-11.1203826666689,-11.0069371201003,-10.9201533730741,
-10.8031896759694,-10.6865155346278,-10.5700128234899,-10.4536777554397,
-10.3752088276281),.UNSPECIFIED.);
#297=B_SPLINE_CURVE_WITH_KNOTS('',3,(#32576,#32577,#32578,#32579,#32580,
#32581,#32582,#32583,#32584,#32585,#32586,#32587,#32588,#32589,#32590,#32591,
#32592,#32593,#32594,#32595,#32596,#32597,#32598,#32599,#32600,#32601,#32602,
#32603,#32604,#32605,#32606,#32607,#32608,#32609,#32610,#32611,#32612,#32613,
#32614,#32615,#32616,#32617,#32618,#32619,#32620,#32621,#32622,#32623,#32624,
#32625,#32626,#32627,#32628,#32629,#32630,#32631,#32632,#32633,#32634,#32635,
#32636,#32637,#32638,#32639,#32640,#32641,#32642,#32643,#32644,#32645,#32646,
#32647,#32648,#32649,#32650,#32651,#32652,#32653,#32654,#32655,#32656,#32657,
#32658,#32659,#32660,#32661,#32662,#32663,#32664,#32665,#32666,#32667,#32668,
#32669,#32670,#32671,#32672,#32673,#32674,#32675,#32676,#32677,#32678,#32679,
#32680,#32681,#32682,#32683,#32684,#32685,#32686,#32687,#32688,#32689,#32690,
#32691,#32692,#32693,#32694,#32695,#32696,#32697,#32698,#32699,#32700,#32701,
#32702,#32703,#32704,#32705,#32706,#32707,#32708,#32709,#32710,#32711,#32712,
#32713,#32714,#32715,#32716,#32717,#32718,#32719,#32720,#32721,#32722,#32723,
#32724,#32725,#32726,#32727,#32728,#32729,#32730,#32731,#32732,#32733,#32734,
#32735,#32736,#32737,#32738,#32739,#32740,#32741,#32742,#32743,#32744,#32745,
#32746,#32747),.UNSPECIFIED.,.F.,.F.,(4,3,3,3,3,3,3,3,3,3,3,3,3,3,3,3,3,
3,3,3,3,3,3,3,3,3,3,3,3,3,3,3,3,3,3,3,3,3,3,3,3,3,3,3,3,3,3,3,3,3,3,3,3,
3,3,3,3,4),(7.40592711364043,7.52254421271226,7.63940844128119,7.75640405188725,
7.87369086241296,7.94192972587207,8.05541344444123,8.16869552285997,8.28186555550056,
8.39496834237503,8.50804858342432,8.62123275397868,8.73446843335694,8.84791774642208,
8.93467094160608,9.04815210392042,9.16143166055977,9.27459919455485,9.38769951052788,
9.50077731305781,9.61395911540794,9.72719246201059,9.84063953017342,9.92741215734009,
10.0408890554138,10.1541642137661,10.267327270786,10.3804230392832,10.4934962319243,
10.6066733642354,10.7199020001953,10.8333443496985,10.9201533730741,11.0336333034009,
11.1469115595896,11.260077752197,11.3731766882899,11.4862530748409,11.5994334163036,
11.7126652748211,11.826110828601,11.9128945888081,12.0263739369873,12.1396516092528,
12.2528172173109,12.3659155693028,12.4789913732743,12.5921711392499,12.7054024253357,
12.8188474189226,12.9056358045421,13.0175007058498,13.1292062137034,13.2407996694667,
13.3528778571923,13.4644298780027,13.5767711491859,13.6891124203691),
 .UNSPECIFIED.);
#298=B_SPLINE_CURVE_WITH_KNOTS('',3,(#32752,#32753,#32754,#32755,#32756,
#32757,#32758,#32759,#32760,#32761,#32762,#32763,#32764,#32765,#32766,#32767,
#32768,#32769,#32770,#32771,#32772,#32773,#32774,#32775,#32776,#32777,#32778,
#32779,#32780,#32781,#32782,#32783,#32784,#32785,#32786,#32787,#32788,#32789,
#32790,#32791,#32792,#32793,#32794,#32795,#32796,#32797,#32798,#32799,#32800,
#32801,#32802,#32803,#32804,#32805,#32806,#32807,#32808,#32809,#32810,#32811,
#32812,#32813,#32814,#32815,#32816,#32817,#32818,#32819,#32820,#32821,#32822,
#32823,#32824,#32825,#32826,#32827,#32828,#32829,#32830,#32831,#32832,#32833,
#32834,#32835,#32836,#32837,#32838,#32839,#32840,#32841,#32842,#32843,#32844,
#32845,#32846,#32847,#32848,#32849,#32850,#32851,#32852,#32853,#32854,#32855,
#32856,#32857,#32858,#32859,#32860,#32861,#32862,#32863,#32864,#32865,#32866,
#32867,#32868,#32869,#32870,#32871,#32872,#32873,#32874,#32875,#32876,#32877,
#32878,#32879,#32880,#32881,#32882,#32883,#32884,#32885,#32886,#32887,#32888,
#32889,#32890,#32891,#32892,#32893,#32894,#32895,#32896,#32897,#32898,#32899,
#32900,#32901,#32902,#32903,#32904,#32905,#32906,#32907,#32908,#32909,#32910,
#32911,#32912,#32913,#32914,#32915,#32916,#32917,#32918,#32919,#32920,#32921,
#32922,#32923),.UNSPECIFIED.,.F.,.F.,(4,3,3,3,3,3,3,3,3,3,3,3,3,3,3,3,3,
3,3,3,3,3,3,3,3,3,3,3,3,3,3,3,3,3,3,3,3,3,3,3,3,3,3,3,3,3,3,3,3,3,3,3,3,
3,3,3,3,4),(-22.9415794419873,-22.8330479618822,-22.7195687853659,-22.6062912933183,
-22.4931258705797,-22.3800277086708,-22.2669520992146,-22.1537725331014,
-22.0405414501564,-21.9270966625821,-21.8403067461482,-21.7268275693145,
-21.6135500769637,-21.500384653931,-21.3872864917374,-21.2742108820062,
-21.1610313156354,-21.0478002324418,-20.9343554446367,-20.8475655304142,
-20.734086350754,-20.6208088555591,-20.5076434296737,-20.3945452646239,
-20.2814696520382,-20.1682900828382,-20.0550589968252,-19.941614206252,
-19.8548243146802,-19.7413451423172,-19.6280676544019,-19.5149022357798,
-19.4018040779645,-19.2887284725718,-19.175548910444,-19.0623178314471,
-18.9488730477109,-18.8620830989461,-18.7486039218275,-18.6353264292627,
-18.5221610060591,-18.4090628437377,-18.2959872339214,-18.1828076675315,
-18.0695765843554,-17.9561317966267,-17.8693418832121,-17.7558626881208,
-17.6425851774241,-17.5294197360051,-17.416321555418,-17.3032459273188,
-17.1900663427658,-17.0768352414653,-16.9633904359026,-16.8766006674781,
-16.7220055544691,-16.6583941348077),.UNSPECIFIED.);
#299=B_SPLINE_CURVE_WITH_KNOTS('',3,(#32924,#32925,#32926,#32927,#32928,
#32929,#32930,#32931,#32932,#32933,#32934,#32935,#32936,#32937,#32938,#32939,
#32940,#32941,#32942,#32943,#32944,#32945,#32946,#32947,#32948,#32949,#32950,
#32951,#32952,#32953,#32954,#32955,#32956,#32957,#32958,#32959,#32960,#32961,
#32962,#32963,#32964,#32965,#32966,#32967,#32968,#32969,#32970,#32971,#32972,
#32973,#32974,#32975,#32976,#32977,#32978,#32979,#32980,#32981,#32982,#32983,
#32984,#32985,#32986,#32987,#32988,#32989,#32990,#32991,#32992,#32993,#32994,
#32995,#32996,#32997,#32998,#32999,#33000,#33001,#33002,#33003,#33004,#33005,
#33006,#33007,#33008,#33009,#33010,#33011,#33012,#33013,#33014,#33015,#33016,
#33017,#33018,#33019,#33020,#33021,#33022,#33023,#33024,#33025,#33026,#33027,
#33028,#33029,#33030,#33031,#33032,#33033,#33034,#33035,#33036,#33037,#33038,
#33039,#33040,#33041,#33042,#33043,#33044,#33045,#33046,#33047,#33048,#33049,
#33050,#33051,#33052,#33053,#33054,#33055,#33056,#33057,#33058,#33059,#33060,
#33061,#33062,#33063,#33064,#33065,#33066,#33067,#33068,#33069,#33070,#33071,
#33072,#33073,#33074,#33075,#33076,#33077,#33078,#33079,#33080,#33081,#33082,
#33083,#33084,#33085,#33086,#33087,#33088,#33089,#33090,#33091,#33092,#33093,
#33094,#33095),.UNSPECIFIED.,.F.,.F.,(4,3,3,3,3,3,3,3,3,3,3,3,3,3,3,3,3,
3,3,3,3,3,3,3,3,3,3,3,3,3,3,3,3,3,3,3,3,3,3,3,3,3,3,3,3,3,3,3,3,3,3,3,3,
3,3,3,3,4),(13.68911242082,13.8466881871004,13.8983770202761,14.0118563143335,
14.1251339258355,14.2382994691069,14.3513977524058,14.4644734838899,14.5776531720396,
14.6908843772135,14.804329285801,14.8911182360101,15.0045974231147,15.1178749266047,
15.2310403613002,15.3441385356588,15.4572141580369,15.5703937377043,15.6836248345758,
15.7970696365178,15.8838594517441,15.9973385929408,16.1106160486916,16.2237814345631,
16.3368795591022,16.4499551307528,16.5631346586859,16.676365703184,16.789810452353,
16.8766006674781,16.9900798618807,17.1033573721298,17.2165228132485,17.3296209936827,
17.4426966217761,17.5558762065502,17.6691073081982,17.7825521143103,17.8693418832121,
17.9828210599164,18.0960985522228,18.2092639752631,18.3223621375165,18.4354377473594,
18.5486173139223,18.6618483973528,18.7752931854659,18.8620830989461,18.9755622717187,
19.0888397598947,19.2020051786863,19.3151033365802,19.4281789419606,19.541358503936,
19.6545895827026,19.7680343660839,19.8548243146801,19.9722977279996),
 .UNSPECIFIED.);
#300=B_SPLINE_CURVE_WITH_KNOTS('',3,(#33100,#33101,#33102,#33103,#33104,
#33105,#33106,#33107,#33108,#33109,#33110,#33111,#33112,#33113,#33114,#33115,
#33116,#33117,#33118,#33119,#33120,#33121,#33122,#33123,#33124,#33125,#33126,
#33127,#33128,#33129,#33130,#33131,#33132,#33133,#33134,#33135,#33136,#33137,
#33138,#33139,#33140,#33141,#33142,#33143,#33144,#33145,#33146,#33147,#33148,
#33149,#33150,#33151,#33152,#33153,#33154,#33155,#33156,#33157,#33158,#33159,
#33160,#33161,#33162,#33163,#33164,#33165,#33166,#33167,#33168,#33169,#33170,
#33171,#33172,#33173,#33174,#33175,#33176,#33177,#33178,#33179,#33180,#33181,
#33182,#33183,#33184,#33185,#33186,#33187,#33188,#33189,#33190,#33191,#33192,
#33193,#33194,#33195,#33196,#33197,#33198,#33199,#33200,#33201,#33202,#33203,
#33204,#33205,#33206,#33207,#33208,#33209,#33210,#33211,#33212,#33213,#33214,
#33215,#33216,#33217,#33218,#33219,#33220,#33221,#33222,#33223,#33224,#33225,
#33226,#33227,#33228,#33229,#33230,#33231,#33232,#33233,#33234,#33235,#33236,
#33237,#33238,#33239,#33240,#33241,#33242,#33243,#33244,#33245,#33246,#33247,
#33248,#33249,#33250,#33251,#33252,#33253,#33254,#33255,#33256,#33257,#33258,
#33259,#33260,#33261,#33262,#33263,#33264,#33265,#33266,#33267,#33268,#33269,
#33270,#33271),.UNSPECIFIED.,.F.,.F.,(4,3,3,3,3,3,3,3,3,3,3,3,3,3,3,3,3,
3,3,3,3,3,3,3,3,3,3,3,3,3,3,3,3,3,3,3,3,3,3,3,3,3,3,3,3,3,3,3,3,3,3,3,3,
3,3,3,3,4),(-29.2247647485903,-29.1026702317892,-28.9802494953267,-28.8573319787146,
-28.7894952562862,-28.6760160792305,-28.5627385866474,-28.449573163376,
-28.336475000938,-28.2233993909572,-28.1102198243307,-27.9969887408777,
-27.8835439528106,-27.7967540405522,-27.6832748635018,-27.5699973709241,
-27.4568319476583,-27.3437337852261,-27.2306581752511,-27.1174786086306,
-27.0042475251837,-26.8908027371227,-26.8040128248182,-26.690533647707,
-26.5772561550685,-26.4640907317418,-26.3509925692487,-26.237916959213,
-26.1247373925325,-26.011506309026,-25.8980615209065,-25.8112716090842,
-25.6977924320825,-25.5845149395528,-25.4713495163346,-25.3582513539493,
-25.2451757440206,-25.131996177445,-25.0187650940424,-24.905320306024,-24.8185303933502,
-24.7050512163485,-24.5917737238206,-24.4786083006053,-24.3655101382241,
-24.2524345283007,-24.139254961732,-24.0260238783372,-23.912579090328,-23.8257891776162,
-23.7138259496525,-23.6020187560681,-23.4903204007749,-23.3786838657664,
-23.2669922326728,-23.1552793919515,-23.0433808076553,-22.941579442425),
 .UNSPECIFIED.);
#301=B_SPLINE_CURVE_WITH_KNOTS('',3,(#33272,#33273,#33274,#33275,#33276,
#33277,#33278,#33279,#33280,#33281,#33282,#33283,#33284,#33285,#33286,#33287,
#33288,#33289,#33290,#33291,#33292,#33293,#33294,#33295,#33296,#33297,#33298,
#33299,#33300,#33301,#33302,#33303,#33304,#33305,#33306,#33307,#33308,#33309,
#33310,#33311,#33312,#33313,#33314,#33315,#33316,#33317,#33318,#33319,#33320,
#33321,#33322,#33323,#33324,#33325,#33326,#33327,#33328,#33329,#33330,#33331,
#33332,#33333,#33334,#33335,#33336,#33337,#33338,#33339,#33340,#33341,#33342,
#33343,#33344,#33345,#33346,#33347,#33348,#33349,#33350,#33351,#33352,#33353,
#33354,#33355,#33356,#33357,#33358,#33359,#33360,#33361,#33362,#33363,#33364,
#33365,#33366,#33367,#33368,#33369,#33370,#33371,#33372,#33373,#33374,#33375,
#33376,#33377,#33378,#33379,#33380,#33381,#33382,#33383,#33384,#33385,#33386,
#33387,#33388,#33389,#33390,#33391,#33392,#33393,#33394,#33395,#33396,#33397,
#33398,#33399,#33400,#33401,#33402,#33403,#33404,#33405,#33406,#33407,#33408,
#33409,#33410,#33411,#33412,#33413,#33414,#33415,#33416,#33417,#33418,#33419,
#33420,#33421,#33422,#33423,#33424,#33425,#33426,#33427,#33428,#33429,#33430,
#33431,#33432,#33433,#33434,#33435,#33436,#33437,#33438,#33439,#33440,#33441,
#33442,#33443),.UNSPECIFIED.,.F.,.F.,(4,3,3,3,3,3,3,3,3,3,3,3,3,3,3,3,3,
3,3,3,3,3,3,3,3,3,3,3,3,3,3,3,3,3,3,3,3,3,3,3,3,3,3,3,3,3,3,3,3,3,3,3,3,
3,3,3,3,4),(19.9722977284267,20.0841292785655,20.1958270514293,20.3074382184884,
20.4190098076767,20.5306685538794,20.6423678179856,20.7542767869761,20.8475655304142,
20.9610447072092,21.074322199536,21.187487622554,21.3005857847419,21.4136613944765,
21.5268409608648,21.6400720440837,21.7535168319264,21.8403067461482,21.9537859227176,
22.067063414799,22.1802288375596,22.2933269994785,22.4064026089331,22.5195821750265,
22.6328132579415,22.7462580454697,22.8330479618822,22.9465271392873,23.0598046322271,
23.1729700558593,23.2860682186617,23.3991438290096,23.5123233960049,23.6255544798281,
23.7389992682632,23.8257891776162,23.9392683546151,24.0525458471412,24.1657112703555,
24.2788094327363,24.3918850426602,24.5050646092305,24.6182956926275,24.7317404806399,
24.8185303933502,24.9320095703586,25.0452870628925,25.1584524861135,25.2715506485001,
25.3846262584287,25.4978058250018,25.6110369084006,25.7244816964131,25.8112716090842,
25.9335247835262,26.0554606987231,26.1769226517213,26.2554830346759),
 .UNSPECIFIED.);
#302=B_SPLINE_CURVE_WITH_KNOTS('',3,(#33448,#33449,#33450,#33451,#33452,
#33453,#33454,#33455,#33456,#33457,#33458,#33459,#33460,#33461,#33462,#33463,
#33464,#33465,#33466,#33467,#33468,#33469,#33470,#33471,#33472,#33473,#33474,
#33475,#33476,#33477,#33478,#33479,#33480,#33481,#33482,#33483,#33484,#33485,
#33486,#33487,#33488,#33489,#33490,#33491,#33492,#33493,#33494,#33495,#33496,
#33497,#33498,#33499,#33500,#33501,#33502,#33503,#33504,#33505,#33506,#33507,
#33508,#33509,#33510,#33511,#33512,#33513,#33514,#33515,#33516,#33517,#33518,
#33519,#33520,#33521,#33522,#33523,#33524,#33525,#33526,#33527,#33528,#33529,
#33530,#33531,#33532,#33533,#33534,#33535,#33536,#33537,#33538,#33539,#33540,
#33541,#33542,#33543,#33544,#33545,#33546,#33547,#33548,#33549,#33550,#33551,
#33552,#33553,#33554,#33555,#33556,#33557,#33558,#33559,#33560,#33561,#33562,
#33563,#33564,#33565,#33566,#33567,#33568,#33569,#33570,#33571,#33572,#33573,
#33574,#33575,#33576,#33577,#33578,#33579,#33580,#33581,#33582,#33583,#33584,
#33585,#33586,#33587,#33588,#33589,#33590,#33591,#33592,#33593,#33594,#33595,
#33596,#33597,#33598,#33599,#33600,#33601,#33602,#33603,#33604,#33605,#33606,
#33607,#33608,#33609,#33610,#33611,#33612,#33613,#33614,#33615,#33616,#33617,
#33618,#33619),.UNSPECIFIED.,.F.,.F.,(4,3,3,3,3,3,3,3,3,3,3,3,3,3,3,3,3,
3,3,3,3,3,3,3,3,3,3,3,3,3,3,3,3,3,3,3,3,3,3,3,3,3,3,3,3,3,3,3,3,3,3,3,3,
3,3,3,3,4),(-35.5079500558816,-35.3961730046961,-35.2844803930079,-35.1728253066734,
-35.0610809083684,-34.9492943671217,-34.837297707012,-34.7459425506903,
-34.6324633736283,-34.5191858810389,-34.4060204577614,-34.2929222953172,
-34.1798466853304,-34.066667118698,-33.9534360352393,-33.8399912471666,
-33.7532013349563,-33.6397221578946,-33.5264446653055,-33.4132792420282,
-33.3001810795844,-33.1871054695977,-33.0739259029656,-32.9606948195071,
-32.8472500314346,-32.7604601192223,-32.6469809421594,-32.5337034495691,
-32.4205380262906,-32.3074398638457,-32.1943642538579,-32.0811846872246,
-31.9679536037652,-31.8545088156916,-31.7677189034882,-31.6542397264265,
-31.5409622338377,-31.4277968105605,-31.3146986481168,-31.2016230381304,
-31.0884434714985,-30.9752123880402,-30.8617675999679,-30.7749776877542,
-30.6614985106941,-30.5482210181067,-30.4350555948313,-30.3219574323891,
-30.2088818224045,-30.0957022557741,-29.9824711723175,-29.8690263842467,
-29.7822364720202,-29.6657715448526,-29.5495817486318,-29.4335543161685,
-29.3176737571639,-29.2247647491669),.UNSPECIFIED.);
#303=B_SPLINE_CURVE_WITH_KNOTS('',3,(#33620,#33621,#33622,#33623,#33624,
#33625,#33626,#33627,#33628,#33629,#33630,#33631,#33632,#33633,#33634,#33635,
#33636,#33637,#33638,#33639,#33640,#33641,#33642,#33643,#33644,#33645,#33646,
#33647,#33648,#33649,#33650,#33651,#33652,#33653,#33654,#33655,#33656,#33657,
#33658,#33659,#33660,#33661,#33662,#33663,#33664,#33665,#33666,#33667,#33668,
#33669,#33670,#33671,#33672,#33673,#33674,#33675,#33676,#33677,#33678,#33679,
#33680,#33681,#33682,#33683,#33684,#33685,#33686,#33687,#33688,#33689,#33690,
#33691,#33692,#33693,#33694,#33695,#33696,#33697,#33698,#33699,#33700,#33701,
#33702,#33703,#33704,#33705,#33706,#33707,#33708,#33709,#33710,#33711,#33712,
#33713,#33714,#33715,#33716,#33717,#33718,#33719,#33720,#33721,#33722,#33723,
#33724,#33725,#33726,#33727,#33728,#33729,#33730,#33731,#33732,#33733,#33734,
#33735,#33736,#33737,#33738,#33739,#33740,#33741,#33742,#33743,#33744,#33745,
#33746,#33747,#33748,#33749,#33750,#33751,#33752,#33753,#33754,#33755,#33756,
#33757,#33758,#33759,#33760,#33761,#33762,#33763,#33764,#33765,#33766,#33767,
#33768,#33769,#33770,#33771,#33772,#33773,#33774,#33775,#33776,#33777,#33778,
#33779,#33780,#33781,#33782,#33783,#33784,#33785,#33786,#33787,#33788,#33789,
#33790,#33791),.UNSPECIFIED.,.F.,.F.,(4,3,3,3,3,3,3,3,3,3,3,3,3,3,3,3,3,
3,3,3,3,3,3,3,3,3,3,3,3,3,3,3,3,3,3,3,3,3,3,3,3,3,3,3,3,3,3,3,3,3,3,3,3,
3,3,3,3,4),(26.2554830351792,26.3716311906272,26.4880031249538,26.6044911021221,
26.7212648320428,26.8040128248182,26.9174920018686,27.0307694944462,27.1439349177118,
27.2570330801439,27.3701086901187,27.4832882567393,27.5965193401862,27.7099641282473,
27.7967540405522,27.9102332176087,28.0235107101925,28.1366761334643,28.2497742959025,
28.3628499058832,28.4760294725095,28.5892605559621,28.7027053440286,28.7894952562862,
28.9029744333544,29.0162519259501,29.1294173492341,29.2425155116847,29.355591121678,
29.468770688317,29.5820017717822,29.6954465598615,29.7822364720202,29.8957156490803,
30.0089931416678,30.1221585649435,30.2352567273858,30.3483323373709,30.4615119040014,
30.5747429874581,30.688187775529,30.7749776877543,30.8884568648157,31.0017343574046,
31.1148997806817,31.2279979431252,31.3410735531117,31.4542531197435,31.5674842032017,
31.6809289912738,31.7677189034883,31.8796560322216,31.9914328602303,32.1030966456068,
32.2147356549155,32.3263521668632,32.4380819604925,32.5386683419494),
 .UNSPECIFIED.);
#304=B_SPLINE_CURVE_WITH_KNOTS('',3,(#33796,#33797,#33798,#33799,#33800,
#33801,#33802,#33803,#33804,#33805,#33806,#33807,#33808,#33809,#33810,#33811,
#33812,#33813,#33814,#33815,#33816,#33817,#33818,#33819,#33820,#33821,#33822,
#33823,#33824,#33825,#33826,#33827,#33828,#33829,#33830,#33831,#33832,#33833,
#33834,#33835,#33836,#33837,#33838,#33839,#33840,#33841,#33842,#33843,#33844,
#33845,#33846,#33847,#33848,#33849,#33850,#33851,#33852,#33853,#33854,#33855,
#33856,#33857,#33858,#33859,#33860,#33861,#33862,#33863,#33864,#33865,#33866,
#33867,#33868,#33869,#33870,#33871,#33872,#33873,#33874,#33875,#33876,#33877,
#33878,#33879,#33880,#33881,#33882,#33883,#33884,#33885,#33886,#33887,#33888,
#33889,#33890,#33891,#33892,#33893,#33894,#33895,#33896,#33897,#33898,#33899,
#33900,#33901,#33902,#33903,#33904,#33905,#33906,#33907,#33908,#33909,#33910,
#33911,#33912,#33913,#33914,#33915,#33916,#33917,#33918,#33919,#33920,#33921,
#33922,#33923,#33924,#33925,#33926,#33927,#33928,#33929,#33930,#33931,#33932,
#33933,#33934,#33935,#33936,#33937,#33938,#33939,#33940,#33941,#33942,#33943,
#33944,#33945,#33946,#33947,#33948,#33949,#33950,#33951,#33952,#33953,#33954,
#33955,#33956,#33957,#33958,#33959,#33960,#33961,#33962,#33963,#33964,#33965,
#33966,#33967),.UNSPECIFIED.,.F.,.F.,(4,3,3,3,3,3,3,3,3,3,3,3,3,3,3,3,3,
3,3,3,3,3,3,3,3,3,3,3,3,3,3,3,3,3,3,3,3,3,3,3,3,3,3,3,3,3,3,3,3,3,3,3,3,
3,3,3,3,4),(-41.791135363526,-41.6951310608283,-41.5816518837661,-41.4683743911766,
-41.355208967899,-41.2421108054547,-41.1290351954678,-41.0158556288353,
-40.9026245453764,-40.7891797573035,-40.7023898450943,-40.5889106680321,
-40.4756331754426,-40.3624677521649,-40.2493695897207,-40.1362939797336,
-40.0231144131011,-39.9098833296422,-39.7964385415693,-39.7096486293603,
-39.5961694522984,-39.482891959709,-39.3697265364315,-39.2566283739875,
-39.1435527640006,-39.0303731973683,-38.9171421139096,-38.8036973258369,
-38.7169074136263,-38.6034282365642,-38.4901507439748,-38.3769853206972,
-38.263887158253,-38.1508115482661,-38.0376319816337,-37.9244008981749,
-37.8109561101021,-37.7241661978923,-37.6106870208302,-37.4974095282408,
-37.3842441049631,-37.271145942519,-37.158070332532,-37.0448907658995,-36.9316596824407,
-36.8182148943679,-36.7314249821583,-36.6179458050963,-36.5046683125069,
-36.3915028892294,-36.2784047267853,-36.1653291167985,-36.0521495501662,
-35.9389184667075,-35.8254736786347,-35.7386837664243,-35.5878041738866,
-35.5079500563465),.UNSPECIFIED.);
#305=B_SPLINE_CURVE_WITH_KNOTS('',3,(#33968,#33969,#33970,#33971,#33972,
#33973,#33974,#33975,#33976,#33977,#33978,#33979,#33980,#33981,#33982,#33983,
#33984,#33985,#33986,#33987,#33988,#33989,#33990,#33991,#33992,#33993,#33994,
#33995,#33996,#33997,#33998,#33999,#34000,#34001,#34002,#34003,#34004,#34005,
#34006,#34007,#34008,#34009,#34010,#34011,#34012,#34013,#34014,#34015,#34016,
#34017,#34018,#34019,#34020,#34021,#34022,#34023,#34024,#34025,#34026,#34027,
#34028,#34029,#34030,#34031,#34032,#34033,#34034,#34035,#34036,#34037,#34038,
#34039,#34040,#34041,#34042,#34043,#34044,#34045,#34046,#34047,#34048,#34049,
#34050,#34051,#34052,#34053,#34054,#34055,#34056,#34057,#34058,#34059,#34060,
#34061,#34062,#34063,#34064,#34065,#34066,#34067,#34068,#34069,#34070,#34071,
#34072,#34073,#34074,#34075,#34076,#34077,#34078,#34079,#34080,#34081,#34082,
#34083,#34084,#34085,#34086,#34087,#34088,#34089,#34090,#34091,#34092,#34093,
#34094,#34095,#34096,#34097,#34098,#34099,#34100,#34101,#34102,#34103,#34104,
#34105,#34106,#34107,#34108,#34109,#34110,#34111,#34112,#34113,#34114,#34115,
#34116,#34117,#34118,#34119,#34120,#34121,#34122,#34123,#34124,#34125,#34126,
#34127,#34128,#34129,#34130,#34131,#34132,#34133,#34134,#34135,#34136,#34137,
#34138,#34139),.UNSPECIFIED.,.F.,.F.,(4,3,3,3,3,3,3,3,3,3,3,3,3,3,3,3,3,
3,3,3,3,3,3,3,3,3,3,3,3,3,3,3,3,3,3,3,3,3,3,3,3,3,3,3,3,3,3,3,3,3,3,3,3,
3,3,3,3,4),(32.5386683423588,32.692149172839,32.7604601192223,32.873939296284,
32.9872167888731,33.1003822121503,33.2134803745941,33.3265559845806,33.4397355512127,
33.5529666346711,33.6664114227435,33.7532013349563,33.8666805120184,33.9799580046078,
34.0931234278855,34.2062215903296,34.3192972003165,34.4324767669489,34.5457078504077,
34.6591526384805,34.7459425506903,34.8594217277524,34.9726992203419,35.0858646436196,
35.1989628060638,35.3120384160508,35.4252179826833,35.5384490661421,35.651893854215,
35.7386837664243,35.8521629434862,35.9654404360756,36.0786058593531,36.1917040217971,
36.3047796317839,36.4179591984163,36.5311902818749,36.6446350699476,36.7314249821583,
36.8449041592204,36.95818165181,37.0713470750876,37.1844452375319,37.2975208475188,
37.4107004141514,37.5239314976102,37.6373762856831,37.7241661978923,37.8376453749543,
37.9509228675437,38.0640882908212,38.1771864532653,38.2902620632522,38.4034416298846,
38.5166727133433,38.630117501416,38.7169074136263,38.8218536495384),
 .UNSPECIFIED.);
#306=B_SPLINE_CURVE_WITH_KNOTS('',3,(#34144,#34145,#34146,#34147,#34148,
#34149,#34150,#34151,#34152,#34153,#34154,#34155,#34156,#34157,#34158,#34159,
#34160,#34161,#34162,#34163,#34164,#34165,#34166,#34167,#34168,#34169,#34170,
#34171,#34172,#34173,#34174,#34175,#34176,#34177,#34178,#34179,#34180,#34181,
#34182,#34183,#34184,#34185,#34186,#34187,#34188,#34189,#34190,#34191,#34192,
#34193,#34194,#34195,#34196,#34197,#34198,#34199,#34200,#34201,#34202,#34203,
#34204,#34205,#34206,#34207,#34208,#34209,#34210,#34211,#34212,#34213,#34214,
#34215,#34216,#34217,#34218,#34219,#34220,#34221,#34222,#34223,#34224,#34225,
#34226,#34227,#34228,#34229,#34230,#34231,#34232,#34233,#34234,#34235,#34236,
#34237,#34238,#34239,#34240,#34241,#34242,#34243,#34244,#34245,#34246,#34247,
#34248,#34249,#34250,#34251,#34252,#34253,#34254,#34255,#34256,#34257,#34258,
#34259,#34260,#34261,#34262,#34263,#34264,#34265,#34266,#34267,#34268,#34269,
#34270,#34271,#34272,#34273,#34274,#34275,#34276,#34277,#34278,#34279,#34280,
#34281,#34282,#34283,#34284,#34285,#34286,#34287,#34288,#34289,#34290,#34291,
#34292,#34293,#34294,#34295,#34296,#34297,#34298,#34299,#34300,#34301,#34302,
#34303,#34304,#34305,#34306,#34307,#34308,#34309,#34310,#34311,#34312,#34313,
#34314,#34315),.UNSPECIFIED.,.F.,.F.,(4,3,3,3,3,3,3,3,3,3,3,3,3,3,3,3,3,
3,3,3,3,3,3,3,3,3,3,3,3,3,3,3,3,3,3,3,3,3,3,3,3,3,3,3,3,3,3,3,3,3,3,3,3,
3,3,3,3,4),(-48.0743206700366,-47.9513559785244,-47.8280201492357,-47.7041583150349,
-47.6515783552324,-47.5380991781703,-47.4248216855807,-47.311656262303,
-47.1985580998588,-47.0854824898718,-46.9723029232392,-46.8590718397803,
-46.7456270517074,-46.6588371394984,-46.5453579624364,-46.4320804698471,
-46.3189150465696,-46.2058168841256,-46.0927412741388,-45.9795617075064,
-45.8663306240477,-45.752885835975,-45.6660959237644,-45.5526167467024,
-45.4393392541129,-45.3261738308353,-45.2130756683912,-45.1000000584043,
-44.9868204917719,-44.8735894083131,-44.7601446202403,-44.6733547080304,
-44.5598755309683,-44.4465980383788,-44.3334326151011,-44.2203344526569,
-44.10725884267,-43.9940792760374,-43.8808481925786,-43.7674034045057,-43.6806134922963,
-43.5671343152343,-43.4538568226449,-43.3406913993673,-43.2275932369232,
-43.1145176269363,-43.0013380603039,-42.8881069768452,-42.7746621887724,
-42.6878722765623,-42.5757801624873,-42.4638771065973,-42.3520829464153,
-42.2403507816478,-42.1280469272264,-42.0162357830346,-41.9036855734984,
-41.7911353639623),.UNSPECIFIED.);
#307=B_SPLINE_CURVE_WITH_KNOTS('',3,(#34316,#34317,#34318,#34319,#34320,
#34321,#34322,#34323,#34324,#34325,#34326,#34327,#34328,#34329,#34330,#34331,
#34332,#34333,#34334,#34335,#34336,#34337,#34338,#34339,#34340,#34341,#34342,
#34343,#34344,#34345,#34346,#34347,#34348,#34349,#34350,#34351,#34352,#34353,
#34354,#34355,#34356,#34357,#34358,#34359,#34360,#34361,#34362,#34363,#34364,
#34365,#34366,#34367,#34368,#34369,#34370,#34371,#34372,#34373,#34374,#34375,
#34376,#34377,#34378,#34379,#34380,#34381,#34382,#34383,#34384,#34385,#34386,
#34387,#34388,#34389,#34390,#34391,#34392,#34393,#34394,#34395,#34396,#34397,
#34398,#34399,#34400,#34401,#34402,#34403,#34404,#34405,#34406,#34407,#34408,
#34409,#34410,#34411,#34412,#34413,#34414,#34415,#34416,#34417,#34418,#34419,
#34420,#34421,#34422,#34423,#34424,#34425,#34426,#34427,#34428,#34429,#34430,
#34431,#34432,#34433,#34434,#34435,#34436,#34437,#34438,#34439,#34440,#34441,
#34442,#34443,#34444,#34445,#34446,#34447,#34448,#34449,#34450,#34451,#34452,
#34453,#34454,#34455,#34456,#34457,#34458,#34459,#34460,#34461,#34462,#34463,
#34464,#34465,#34466,#34467,#34468,#34469,#34470,#34471,#34472,#34473,#34474,
#34475,#34476,#34477,#34478,#34479,#34480,#34481,#34482,#34483,#34484,#34485,
#34486,#34487),.UNSPECIFIED.,.F.,.F.,(4,3,3,3,3,3,3,3,3,3,3,3,3,3,3,3,3,
3,3,3,3,3,3,3,3,3,3,3,3,3,3,3,3,3,3,3,3,3,3,3,3,3,3,3,3,3,3,3,3,3,3,3,3,
3,3,3,3,4),(38.8218536499721,38.9337807794537,39.0455700846174,39.1572686518251,
39.2689234195309,39.3806624113781,39.492437953731,39.6044275384758,39.7096486293603,
39.8231278064224,39.9364052990119,40.0495707222895,40.1626688847336,40.2757444947206,
40.3889240613531,40.5021551448117,40.6155999328846,40.7023898450943,40.8158690221563,
40.9291465147457,41.0423119380234,41.1554101004674,41.2684857104543,41.3816652770868,
41.4948963605456,41.6083411486183,41.6951310608283,41.8086102378904,41.9218877304798,
42.0350531537575,42.1481513162016,42.2612269261883,42.3744064928207,42.4876375762795,
42.6010823643522,42.6878722765623,42.8013514536243,42.9146289462137,43.0277943694912,
43.1408925319353,43.2539681419222,43.3671477085544,43.480378792013,43.5938235800858,
43.6806134922963,43.7940926693582,43.9073701619477,44.0205355852253,44.1336337476695,
44.2467093576567,44.3598889242893,44.4731200077481,44.5865647958209,44.6733547080304,
44.7964919316645,44.919285870672,45.0415576677713,45.1050389561137),
 .UNSPECIFIED.);
#308=B_SPLINE_CURVE_WITH_KNOTS('',3,(#34492,#34493,#34494,#34495,#34496,
#34497,#34498,#34499,#34500,#34501,#34502,#34503,#34504,#34505,#34506,#34507,
#34508,#34509,#34510,#34511,#34512,#34513,#34514,#34515,#34516,#34517,#34518,
#34519,#34520,#34521,#34522,#34523,#34524,#34525,#34526,#34527,#34528,#34529,
#34530,#34531,#34532,#34533,#34534,#34535,#34536,#34537,#34538,#34539,#34540,
#34541,#34542,#34543,#34544,#34545,#34546,#34547,#34548,#34549,#34550,#34551,
#34552,#34553,#34554,#34555,#34556,#34557,#34558,#34559,#34560,#34561,#34562,
#34563,#34564,#34565,#34566,#34567,#34568,#34569,#34570,#34571,#34572,#34573,
#34574,#34575,#34576,#34577,#34578,#34579,#34580,#34581,#34582,#34583,#34584,
#34585,#34586,#34587,#34588,#34589,#34590,#34591,#34592,#34593,#34594,#34595,
#34596,#34597,#34598,#34599,#34600,#34601,#34602,#34603,#34604,#34605,#34606,
#34607,#34608,#34609,#34610,#34611,#34612,#34613,#34614,#34615,#34616,#34617,
#34618,#34619,#34620,#34621,#34622,#34623,#34624,#34625,#34626,#34627,#34628,
#34629,#34630,#34631,#34632,#34633,#34634,#34635,#34636,#34637,#34638,#34639,
#34640,#34641,#34642,#34643,#34644,#34645,#34646,#34647,#34648,#34649,#34650,
#34651,#34652,#34653,#34654,#34655,#34656,#34657,#34658,#34659,#34660,#34661,
#34662,#34663),.UNSPECIFIED.,.F.,.F.,(4,3,3,3,3,3,3,3,3,3,3,3,3,3,3,3,3,
3,3,3,3,3,3,3,3,3,3,3,3,3,3,3,3,3,3,3,3,3,3,3,3,3,3,3,3,3,3,3,3,3,3,3,3,
3,3,3,3,4),(-54.3575059778852,-54.2456434060343,-54.1338583683125,-54.0221040958961,
-53.9102549193038,-53.7983577896496,-53.6862537502742,-53.6080256496364,
-53.4945464725744,-53.3812689799849,-53.2681035567074,-53.1550053942634,
-53.0419297842766,-52.9287502176442,-52.8155191341854,-52.7020743461126,
-52.6152844339024,-52.5018052568402,-52.3885277642508,-52.2753623409732,
-52.162264178529,-52.0491885685422,-51.9360090019097,-51.8227779184509,
-51.7093331303781,-51.6225432181684,-51.5090640411063,-51.3957865485169,
-51.2826211252393,-51.1695229627951,-51.0564473528081,-50.9432677861756,
-50.8300367027168,-50.716591914644,-50.6298020024344,-50.5163228253723,
-50.4030453327828,-50.2898799095051,-50.1767817470609,-50.063706137074,
-49.9505265704415,-49.8372954869827,-49.7238506989099,-49.6370607867004,
-49.5235816096383,-49.410304117049,-49.2971386937714,-49.1840405313274,
-49.0709649213402,-48.9577853547078,-48.8445542712491,-48.7311094831763,
-48.6443195709664,-48.5283239378195,-48.4125900933358,-48.2970107053752,
-48.1815581061127,-48.0743206707056),.UNSPECIFIED.);
#309=B_SPLINE_CURVE_WITH_KNOTS('',3,(#34664,#34665,#34666,#34667,#34668,
#34669,#34670,#34671,#34672,#34673,#34674,#34675,#34676,#34677,#34678,#34679,
#34680,#34681,#34682,#34683,#34684,#34685,#34686,#34687,#34688,#34689,#34690,
#34691,#34692,#34693,#34694,#34695,#34696,#34697,#34698,#34699,#34700,#34701,
#34702,#34703,#34704,#34705,#34706,#34707,#34708,#34709,#34710,#34711,#34712,
#34713,#34714,#34715,#34716,#34717,#34718,#34719,#34720,#34721,#34722,#34723,
#34724,#34725,#34726,#34727,#34728,#34729,#34730,#34731,#34732,#34733,#34734,
#34735,#34736,#34737,#34738,#34739,#34740,#34741,#34742,#34743,#34744,#34745,
#34746,#34747,#34748,#34749,#34750,#34751,#34752,#34753,#34754,#34755,#34756,
#34757,#34758,#34759,#34760,#34761,#34762,#34763,#34764,#34765,#34766,#34767,
#34768,#34769,#34770,#34771,#34772,#34773,#34774,#34775,#34776,#34777,#34778,
#34779,#34780,#34781,#34782,#34783,#34784,#34785,#34786,#34787,#34788,#34789,
#34790,#34791,#34792,#34793,#34794,#34795,#34796,#34797,#34798,#34799,#34800,
#34801,#34802,#34803,#34804,#34805,#34806,#34807,#34808,#34809,#34810,#34811,
#34812,#34813,#34814,#34815,#34816,#34817,#34818,#34819,#34820,#34821,#34822,
#34823,#34824,#34825,#34826,#34827,#34828,#34829,#34830,#34831,#34832,#34833,
#34834,#34835),.UNSPECIFIED.,.F.,.F.,(4,3,3,3,3,3,3,3,3,3,3,3,3,3,3,3,3,
3,3,3,3,3,3,3,3,3,3,3,3,3,3,3,3,3,3,3,3,3,3,3,3,3,3,3,3,3,3,3,3,3,3,3,3,
3,3,3,3,4),(45.105038956718,45.2207328062171,45.3366289382953,45.4526267946966,
45.5689058923966,45.6660959237644,45.7795751008264,45.8928525934158,46.0060180166932,
46.1191161791372,46.232191789124,46.3453713557563,46.4586024392149,46.5720472272876,
46.6588371394984,46.7723163165606,46.8855938091501,46.9987592324278,47.1118573948719,
47.2249330048587,47.3381125714912,47.4513436549501,47.564788443023,47.6515783552324,
47.7650575322944,47.8783350248838,47.9915004481613,48.1045986106053,48.2176742205921,
48.3308537872245,48.4440848706832,48.557529658756,48.6443195709664,48.7577987480284,
48.8710762406179,48.9842416638955,49.0973398263396,49.2104154363265,49.323595002959,
49.4368260864178,49.5502708744906,49.6370607867004,49.7505399637626,49.863817456352,
49.9769828796296,50.0900810420738,50.2031566520604,50.3163362186928,50.4295673021514,
50.5430120902243,50.6298020024344,50.7418301681541,50.8536969762416,50.9654495759481,
51.0771721138825,51.1888712037852,51.300671980135,51.3882242638976),
 .UNSPECIFIED.);
#310=B_SPLINE_CURVE_WITH_KNOTS('',3,(#34840,#34841,#34842,#34843,#34844,
#34845,#34846,#34847,#34848,#34849,#34850,#34851,#34852,#34853,#34854,#34855,
#34856,#34857,#34858,#34859,#34860,#34861,#34862,#34863,#34864,#34865,#34866,
#34867,#34868,#34869,#34870,#34871,#34872,#34873,#34874,#34875,#34876,#34877,
#34878,#34879,#34880,#34881,#34882,#34883,#34884,#34885,#34886,#34887,#34888,
#34889,#34890,#34891,#34892,#34893,#34894,#34895,#34896,#34897,#34898,#34899,
#34900,#34901,#34902,#34903,#34904,#34905,#34906,#34907,#34908,#34909,#34910,
#34911,#34912,#34913,#34914,#34915,#34916,#34917,#34918,#34919,#34920,#34921,
#34922,#34923,#34924,#34925,#34926,#34927,#34928,#34929,#34930,#34931,#34932,
#34933,#34934,#34935,#34936,#34937,#34938,#34939,#34940,#34941,#34942,#34943,
#34944,#34945,#34946,#34947,#34948,#34949,#34950,#34951,#34952,#34953,#34954,
#34955,#34956,#34957,#34958,#34959,#34960,#34961,#34962,#34963,#34964,#34965,
#34966,#34967,#34968,#34969,#34970,#34971,#34972,#34973,#34974,#34975,#34976,
#34977,#34978,#34979,#34980,#34981,#34982,#34983,#34984,#34985,#34986,#34987,
#34988,#34989,#34990,#34991,#34992,#34993,#34994,#34995,#34996,#34997,#34998,
#34999,#35000,#35001,#35002,#35003,#35004,#35005,#35006,#35007,#35008,#35009,
#35010,#35011),.UNSPECIFIED.,.F.,.F.,(4,3,3,3,3,3,3,3,3,3,3,3,3,3,3,3,3,
3,3,3,3,3,3,3,3,3,3,3,3,3,3,3,3,3,3,3,3,3,3,3,3,3,3,3,3,3,3,3,3,3,3,3,3,
3,3,3,3,4),(-60.6406912850648,-60.5572141597745,-60.4437349827122,-60.3304574901225,
-60.2172920668446,-60.1041939044002,-59.9911182944131,-59.8779387277803,
-59.7647076443212,-59.6512628562482,-59.5644729440405,-59.4509937669785,
-59.3377162743891,-59.2245508511116,-59.1114526886675,-58.9983770786806,
-58.8851975120482,-58.7719664285894,-58.6585216405167,-58.5717317283065,
-58.4582525512445,-58.3449750586551,-58.2318096353775,-58.1187114729334,
-58.0056358629466,-57.8924562963142,-57.7792252128554,-57.6657804247827,
-57.5789905125725,-57.4655113355104,-57.3522338429209,-57.2390684196433,
-57.1259702571991,-57.0128946472122,-56.8997150805797,-56.7864839971209,
-56.673039209048,-56.5862492968384,-56.4727701197763,-56.3594926271869,
-56.2463272039093,-56.1332290414652,-56.0201534314783,-55.9069738648458,
-55.793742781387,-55.6802979933142,-55.5935080811044,-55.4800289040424,
-55.366751411453,-55.2535859881754,-55.1404878257313,-55.0274122157444,
-54.914232649112,-54.8010015656532,-54.6875567775805,-54.6007668653704,
-54.4531582068316,-54.3575059783892),.UNSPECIFIED.);
#311=B_SPLINE_CURVE_WITH_KNOTS('',3,(#35012,#35013,#35014,#35015,#35016,
#35017,#35018,#35019,#35020,#35021,#35022,#35023,#35024,#35025,#35026,#35027,
#35028,#35029,#35030,#35031,#35032,#35033,#35034,#35035,#35036,#35037,#35038,
#35039,#35040,#35041,#35042,#35043,#35044,#35045,#35046,#35047,#35048,#35049,
#35050,#35051,#35052,#35053,#35054,#35055,#35056,#35057,#35058,#35059,#35060,
#35061,#35062,#35063,#35064,#35065,#35066,#35067,#35068,#35069,#35070,#35071,
#35072,#35073,#35074,#35075,#35076,#35077,#35078,#35079,#35080,#35081,#35082,
#35083,#35084,#35085,#35086,#35087,#35088,#35089,#35090,#35091,#35092,#35093,
#35094,#35095,#35096,#35097,#35098,#35099,#35100,#35101,#35102,#35103,#35104,
#35105,#35106,#35107,#35108,#35109,#35110,#35111,#35112,#35113,#35114,#35115,
#35116,#35117,#35118,#35119,#35120,#35121,#35122,#35123,#35124,#35125,#35126,
#35127,#35128,#35129,#35130,#35131,#35132,#35133,#35134,#35135,#35136,#35137,
#35138,#35139,#35140,#35141,#35142,#35143,#35144,#35145,#35146,#35147,#35148,
#35149,#35150,#35151,#35152,#35153,#35154,#35155,#35156,#35157,#35158,#35159,
#35160,#35161,#35162,#35163,#35164,#35165,#35166,#35167,#35168,#35169,#35170,
#35171,#35172,#35173,#35174,#35175,#35176,#35177,#35178,#35179,#35180,#35181,
#35182,#35183),.UNSPECIFIED.,.F.,.F.,(4,3,3,3,3,3,3,3,3,3,3,3,3,3,3,3,3,
3,3,3,3,3,3,3,3,3,3,3,3,3,3,3,3,3,3,3,3,3,3,3,3,3,3,3,3,3,3,3,3,3,3,3,3,
3,3,3,3,4),(51.3882242642754,51.5381262078476,51.6225432181684,51.7360223952304,
51.8492998878198,51.9624653110973,52.0755634735413,52.1886390835281,52.3018186501605,
52.4150497336192,52.528494521692,52.6152844339024,52.7287636109646,52.8420411035543,
52.9552065268321,53.0683046892764,53.1813802992635,53.2945598658962,53.4077909493552,
53.5212357374281,53.6080256496364,53.7215048266983,53.8347823192877,53.9479477425652,
54.0610459050092,54.174121514996,54.2873010816284,54.400532165087,54.5139769531597,
54.6007668653704,54.7142460424324,54.8275235350218,54.9406889582994,55.0537871207435,
55.1668627307304,55.2800422973628,55.3932733808216,55.5067181688944,55.5935080811044,
55.7069872581665,55.820264750756,55.9334301740336,56.0465283364778,56.1596039464647,
56.2727835130972,56.386014596556,56.4994593846288,56.5862492968384,56.6997284739004,
56.8130059664899,56.9261713897674,57.0392695522115,57.1523451621984,57.2655247288308,
57.3787558122896,57.4922006003623,57.5789905125724,57.6714095710771),
 .UNSPECIFIED.);
#312=B_SPLINE_CURVE_WITH_KNOTS('',3,(#35188,#35189,#35190,#35191,#35192,
#35193,#35194,#35195,#35196,#35197,#35198,#35199,#35200,#35201,#35202,#35203,
#35204,#35205,#35206,#35207,#35208,#35209,#35210,#35211,#35212,#35213,#35214,
#35215,#35216,#35217,#35218,#35219,#35220,#35221,#35222,#35223,#35224,#35225,
#35226,#35227,#35228,#35229,#35230,#35231,#35232,#35233,#35234,#35235,#35236,
#35237,#35238,#35239,#35240,#35241,#35242,#35243,#35244,#35245,#35246,#35247,
#35248,#35249,#35250,#35251,#35252,#35253,#35254,#35255,#35256,#35257,#35258,
#35259,#35260,#35261,#35262,#35263,#35264,#35265,#35266,#35267,#35268,#35269,
#35270,#35271,#35272,#35273,#35274,#35275,#35276,#35277,#35278,#35279,#35280,
#35281,#35282,#35283,#35284,#35285,#35286,#35287,#35288,#35289,#35290,#35291,
#35292,#35293,#35294,#35295,#35296,#35297,#35298,#35299,#35300,#35301,#35302,
#35303,#35304,#35305,#35306,#35307,#35308,#35309,#35310,#35311,#35312,#35313,
#35314,#35315,#35316,#35317,#35318,#35319,#35320,#35321,#35322,#35323,#35324,
#35325,#35326,#35327,#35328,#35329,#35330,#35331,#35332,#35333,#35334,#35335,
#35336,#35337,#35338,#35339,#35340,#35341,#35342,#35343,#35344,#35345,#35346,
#35347,#35348,#35349,#35350,#35351,#35352,#35353,#35354,#35355,#35356,#35357,
#35358,#35359),.UNSPECIFIED.,.F.,.F.,(4,3,3,3,3,3,3,3,3,3,3,3,3,3,3,3,3,
3,3,3,3,3,3,3,3,3,3,3,3,3,3,3,3,3,3,3,3,3,3,3,3,3,3,3,3,3,3,3,3,3,3,3,3,
3,3,3,3,4),(-66.9238765918734,-66.7999837454187,-66.6756687169425,-66.5507949918877,
-66.5136614541785,-66.4001822771164,-66.2869047845269,-66.1737393612492,
-66.060641198805,-65.9475655888181,-65.8343860221856,-65.7211549387267,
-65.6077101506539,-65.5209202384445,-65.4074410613825,-65.2941635687931,
-65.1809981455155,-65.0678999830714,-64.9548243730845,-64.8416448064521,
-64.7284137229934,-64.6149689349206,-64.5281790227105,-64.4146998456485,
-64.3014223530591,-64.1882569297815,-64.0751587673374,-63.9620831573505,
-63.8489035907181,-63.7356725072594,-63.6222277191866,-63.5354378069765,
-63.4219586299144,-63.3086811373249,-63.1955157140473,-63.0824175516031,
-62.9693419416161,-62.8561623749836,-62.7429312915248,-62.629486503452,
-62.5426965912425,-62.4292174141805,-62.3159399215912,-62.2027744983137,
-62.0896763358696,-61.9766007258828,-61.8634211592504,-61.7501900757918,
-61.6367452877191,-61.5499553755085,-61.4362973642558,-61.3242814200128,
-61.212373921956,-61.1005281162358,-60.9855689085486,-60.8736400732645,
-60.7571656793757,-60.6406912854869),.UNSPECIFIED.);
#313=B_SPLINE_CURVE_WITH_KNOTS('',3,(#35360,#35361,#35362,#35363,#35364,
#35365,#35366,#35367,#35368,#35369,#35370,#35371,#35372,#35373,#35374,#35375,
#35376,#35377,#35378,#35379,#35380,#35381,#35382,#35383,#35384,#35385,#35386,
#35387,#35388,#35389,#35390,#35391,#35392,#35393,#35394,#35395,#35396,#35397,
#35398,#35399,#35400,#35401,#35402,#35403,#35404,#35405,#35406,#35407,#35408,
#35409,#35410,#35411,#35412,#35413,#35414,#35415,#35416,#35417,#35418,#35419,
#35420,#35421,#35422,#35423,#35424,#35425,#35426,#35427,#35428,#35429,#35430,
#35431,#35432,#35433,#35434,#35435,#35436,#35437,#35438,#35439,#35440,#35441,
#35442,#35443,#35444,#35445,#35446,#35447,#35448,#35449,#35450,#35451,#35452,
#35453,#35454,#35455,#35456,#35457,#35458,#35459,#35460,#35461,#35462,#35463,
#35464,#35465,#35466,#35467,#35468,#35469,#35470,#35471,#35472,#35473,#35474,
#35475,#35476,#35477,#35478,#35479,#35480,#35481,#35482,#35483,#35484,#35485,
#35486,#35487,#35488,#35489,#35490,#35491,#35492,#35493,#35494,#35495,#35496,
#35497,#35498,#35499,#35500,#35501,#35502,#35503,#35504,#35505,#35506,#35507,
#35508,#35509,#35510,#35511,#35512,#35513,#35514,#35515,#35516,#35517,#35518,
#35519,#35520,#35521,#35522,#35523,#35524,#35525,#35526,#35527,#35528,#35529,
#35530,#35531),.UNSPECIFIED.,.F.,.F.,(4,3,3,3,3,3,3,3,3,3,3,3,3,3,3,3,3,
3,3,3,3,3,3,3,3,3,3,3,3,3,3,3,3,3,3,3,3,3,3,3,3,3,3,3,3,3,3,3,3,3,3,3,3,
3,3,3,3,4),(57.6714095715052,57.7839498411054,57.8958482199626,58.0076522192365,
58.1194086614283,58.2324894281479,58.3443610886813,58.4580464084939,58.5717317283065,
58.6852109053686,58.7984883979581,58.9116538212357,59.0247519836799,59.1378275936667,
59.2510071602992,59.364238243758,59.4776830318308,59.5644729440405,59.6779521211025,
59.7912296136919,59.9043950369695,60.0174931994135,60.1305688094003,60.2437483760328,
60.3569794594915,60.4704242475643,60.5572141597745,60.6706933368366,60.783970829426,
60.8971362527035,61.0102344151474,61.1233100251344,61.2364895917668,61.3497206752254,
61.4631654632981,61.5499553755085,61.6634345525706,61.7767120451602,61.8898774684378,
62.0029756308821,62.1160512408688,62.2292308075014,62.3424618909603,62.4559066790332,
62.5426965912425,62.6561757683046,62.7694532608939,62.8826186841714,62.9957168466155,
63.1087924566022,63.2219720232345,63.3352031066934,63.4486478947661,63.5354378069765,
63.6595194390276,63.7832273544188,63.9063594692549,63.9545948779129),
 .UNSPECIFIED.);
#314=B_SPLINE_CURVE_WITH_KNOTS('',3,(#35536,#35537,#35538,#35539,#35540,
#35541,#35542,#35543,#35544,#35545,#35546,#35547,#35548,#35549,#35550,#35551,
#35552,#35553,#35554,#35555,#35556,#35557,#35558,#35559,#35560,#35561,#35562,
#35563,#35564,#35565,#35566,#35567,#35568,#35569,#35570,#35571,#35572,#35573,
#35574,#35575,#35576,#35577,#35578,#35579,#35580,#35581,#35582,#35583,#35584,
#35585,#35586,#35587,#35588,#35589,#35590,#35591,#35592,#35593,#35594,#35595,
#35596,#35597,#35598,#35599,#35600,#35601,#35602,#35603,#35604,#35605,#35606,
#35607,#35608,#35609,#35610,#35611,#35612,#35613,#35614,#35615,#35616,#35617,
#35618,#35619,#35620,#35621,#35622,#35623,#35624,#35625,#35626,#35627,#35628,
#35629,#35630,#35631,#35632,#35633,#35634,#35635,#35636,#35637,#35638,#35639,
#35640,#35641,#35642,#35643,#35644,#35645,#35646,#35647,#35648,#35649,#35650,
#35651,#35652,#35653,#35654,#35655,#35656,#35657,#35658,#35659,#35660,#35661,
#35662,#35663,#35664,#35665,#35666,#35667,#35668,#35669,#35670,#35671,#35672,
#35673,#35674,#35675,#35676,#35677,#35678,#35679,#35680,#35681,#35682,#35683,
#35684,#35685,#35686,#35687,#35688,#35689,#35690,#35691,#35692,#35693,#35694,
#35695,#35696,#35697,#35698,#35699,#35700,#35701,#35702,#35703,#35704,#35705,
#35706,#35707),.UNSPECIFIED.,.F.,.F.,(4,3,3,3,3,3,3,3,3,3,3,3,3,3,3,3,3,
3,3,3,3,3,3,3,3,3,3,3,3,3,3,3,3,3,3,3,3,3,3,3,3,3,3,3,3,3,3,3,3,3,3,3,3,
3,3,3,3,4),(-73.207061899424,-73.0950948311733,-72.9831980604612,-72.8713249933925,
-72.7593511740308,-72.6473233814793,-72.5350916115429,-72.4701087485826,
-72.3566295715205,-72.2433520789311,-72.1301866556534,-72.0170884932091,
-71.9040128832222,-71.7908333165897,-71.6776022331308,-71.5641574450579,
-71.4773675328486,-71.3638883557865,-71.2506108631971,-71.1374454399195,
-71.0243472774754,-70.9112716674883,-70.7980921008558,-70.6848610173971,
-70.5714162293243,-70.4846263171145,-70.3711471400524,-70.257869647463,
-70.1447042241854,-70.0316060617412,-69.9185304517543,-69.8053508851218,
-69.692119801663,-69.5786750135902,-69.4918851013805,-69.3784059243185,
-69.265128431729,-69.1519630084514,-69.0388648460073,-68.9257892360203,
-68.8126096693879,-68.6993785859291,-68.5859337978563,-68.4991438856465,
-68.3856647085844,-68.2723872159949,-68.1592217927173,-68.046123630273,
-67.9330480202861,-67.8198684536536,-67.7066373701949,-67.5931925821221,
-67.5064026699125,-67.3908458947147,-67.2741035690971,-67.1589453653598,
-67.0414109788021,-66.9238765922444),.UNSPECIFIED.);
#315=B_SPLINE_CURVE_WITH_KNOTS('',3,(#35708,#35709,#35710,#35711,#35712,
#35713,#35714,#35715,#35716,#35717,#35718,#35719,#35720,#35721,#35722,#35723,
#35724,#35725,#35726,#35727,#35728,#35729,#35730,#35731,#35732,#35733,#35734,
#35735,#35736,#35737,#35738,#35739,#35740,#35741,#35742,#35743,#35744,#35745,
#35746,#35747,#35748,#35749,#35750,#35751,#35752,#35753,#35754,#35755,#35756,
#35757,#35758,#35759,#35760,#35761,#35762,#35763,#35764,#35765,#35766,#35767,
#35768,#35769,#35770,#35771,#35772,#35773,#35774,#35775,#35776,#35777,#35778,
#35779,#35780,#35781,#35782,#35783,#35784,#35785,#35786,#35787,#35788,#35789,
#35790,#35791,#35792,#35793,#35794,#35795,#35796,#35797,#35798,#35799,#35800,
#35801,#35802,#35803,#35804,#35805,#35806,#35807,#35808,#35809,#35810,#35811,
#35812,#35813,#35814,#35815,#35816,#35817,#35818,#35819,#35820,#35821,#35822,
#35823,#35824,#35825,#35826,#35827,#35828,#35829,#35830,#35831,#35832,#35833,
#35834,#35835,#35836,#35837,#35838,#35839,#35840,#35841,#35842,#35843,#35844,
#35845,#35846,#35847,#35848,#35849,#35850,#35851,#35852,#35853,#35854,#35855,
#35856,#35857,#35858,#35859,#35860,#35861,#35862,#35863,#35864,#35865,#35866,
#35867,#35868,#35869,#35870,#35871,#35872,#35873,#35874,#35875,#35876,#35877,
#35878,#35879),.UNSPECIFIED.,.F.,.F.,(4,3,3,3,3,3,3,3,3,3,3,3,3,3,3,3,3,
3,3,3,3,3,3,3,3,3,3,3,3,3,3,3,3,3,3,3,3,3,3,3,3,3,3,3,3,3,3,3,3,3,3,3,3,
3,3,3,3,4),(63.9545948782567,64.0698636722456,64.1853150539345,64.3008548231995,
64.4166721465947,64.5281790227105,64.6416581997726,64.7549356923621,64.8681011156398,
64.9811992780839,65.0942748880708,65.2074544547033,65.3206855381621,65.434130326235,
65.5209202384445,65.6343994155065,65.747676908096,65.8608423313735,65.9739404938176,
66.0870161038044,66.2001956704368,66.3134267538955,66.4268715419683,66.5136614541785,
66.6271406312406,66.74041812383,66.8535835471076,66.9666817095518,67.0797573195385,
67.1929368861709,67.3061679696297,67.4196127577025,67.5064026699125,67.6198818469746,
67.7331593395642,67.8463247628417,67.959422925286,68.0724985352728,68.1856781019053,
68.298909185364,68.4123539734368,68.4991438856465,68.6126230627086,68.725900555298,
68.8390659785756,68.9521641410198,69.0652397510065,69.1784193176389,69.2916504010977,
69.4050951891705,69.4918851013805,69.6040236394296,69.7159996034553,69.8278600055178,
69.9396848486517,70.051485086998,70.1633755926539,70.2377801854363),
 .UNSPECIFIED.);
#316=B_SPLINE_CURVE_WITH_KNOTS('',3,(#35884,#35885,#35886,#35887,#35888,
#35889,#35890,#35891,#35892,#35893,#35894,#35895,#35896,#35897,#35898,#35899,
#35900,#35901,#35902,#35903,#35904,#35905,#35906,#35907,#35908,#35909,#35910,
#35911,#35912,#35913,#35914,#35915,#35916,#35917,#35918,#35919,#35920,#35921,
#35922,#35923,#35924,#35925,#35926,#35927,#35928,#35929,#35930,#35931,#35932,
#35933,#35934,#35935,#35936,#35937,#35938,#35939,#35940,#35941,#35942,#35943,
#35944,#35945,#35946,#35947,#35948,#35949,#35950,#35951,#35952,#35953,#35954,
#35955,#35956,#35957,#35958,#35959,#35960,#35961,#35962,#35963,#35964,#35965,
#35966,#35967,#35968,#35969,#35970,#35971,#35972,#35973,#35974,#35975,#35976,
#35977,#35978,#35979,#35980,#35981,#35982,#35983,#35984,#35985,#35986,#35987,
#35988,#35989,#35990,#35991,#35992,#35993,#35994,#35995,#35996,#35997,#35998,
#35999,#36000,#36001,#36002,#36003,#36004,#36005,#36006,#36007,#36008,#36009,
#36010,#36011,#36012,#36013,#36014,#36015,#36016,#36017,#36018,#36019,#36020,
#36021,#36022,#36023,#36024,#36025,#36026,#36027,#36028,#36029,#36030,#36031,
#36032,#36033,#36034,#36035,#36036,#36037,#36038,#36039,#36040,#36041,#36042,
#36043,#36044,#36045,#36046,#36047,#36048,#36049,#36050,#36051,#36052,#36053,
#36054,#36055),.UNSPECIFIED.,.F.,.F.,(4,3,3,3,3,3,3,3,3,3,3,3,3,3,3,3,3,
3,3,3,3,3,3,3,3,3,3,3,3,3,3,3,3,3,3,3,3,3,3,3,3,3,3,3,3,3,3,3,3,3,3,3,3,
3,3,3,3,4),(-79.4902472066036,-79.4192972587206,-79.3058180816587,-79.1925405890693,
-79.0793751657918,-78.9662770033477,-78.853201393361,-78.7400218267286,
-78.6267907432699,-78.5133459551973,-78.4265560429866,-78.3130768659242,
-78.1997993733345,-78.0866339500565,-77.9735357876121,-77.8604601776248,
-77.747280610992,-77.6340495275329,-77.5206047394597,-77.4338148272526,
-77.3203356501907,-77.2070581576014,-77.093892734324,-76.98079457188,-76.8677189618932,
-76.7545393952609,-76.6413083118023,-76.5278635237296,-76.4410736115186,
-76.3275944344566,-76.2143169418672,-76.1011515185896,-75.9880533561455,
-75.8749777461586,-75.7617981795262,-75.6485670960674,-75.5351223079947,
-75.4483323957846,-75.3348532187225,-75.221575726133,-75.1084103028553,
-74.9953121404112,-74.8822365304243,-74.7690569637918,-74.655825880333,
-74.5423810922601,-74.4555911800506,-74.3421120029886,-74.2288345103991,
-74.1156690871216,-74.0025709246775,-73.8894953146906,-73.7763157480582,
-73.6630846645994,-73.5496398765266,-73.4628499643166,-73.3181473348919,
-73.2070618999507),.UNSPECIFIED.);
#317=B_SPLINE_CURVE_WITH_KNOTS('',3,(#36056,#36057,#36058,#36059,#36060,
#36061,#36062,#36063,#36064,#36065,#36066,#36067,#36068,#36069,#36070,#36071,
#36072,#36073,#36074,#36075,#36076,#36077,#36078,#36079,#36080,#36081,#36082,
#36083,#36084,#36085,#36086,#36087,#36088,#36089,#36090,#36091,#36092,#36093,
#36094,#36095,#36096,#36097,#36098,#36099,#36100,#36101,#36102,#36103,#36104,
#36105,#36106,#36107,#36108,#36109,#36110,#36111,#36112,#36113,#36114,#36115,
#36116,#36117,#36118,#36119,#36120,#36121,#36122,#36123,#36124,#36125,#36126,
#36127,#36128,#36129,#36130,#36131,#36132,#36133,#36134,#36135,#36136,#36137,
#36138,#36139,#36140,#36141,#36142,#36143,#36144,#36145,#36146,#36147,#36148,
#36149,#36150,#36151,#36152,#36153,#36154,#36155,#36156,#36157,#36158,#36159,
#36160,#36161,#36162,#36163,#36164,#36165,#36166,#36167,#36168,#36169,#36170,
#36171,#36172,#36173,#36174,#36175,#36176,#36177,#36178,#36179,#36180,#36181,
#36182,#36183,#36184,#36185,#36186,#36187,#36188,#36189,#36190,#36191,#36192,
#36193,#36194,#36195,#36196,#36197,#36198,#36199,#36200,#36201,#36202,#36203,
#36204,#36205,#36206,#36207,#36208,#36209,#36210,#36211,#36212,#36213,#36214,
#36215,#36216,#36217,#36218,#36219,#36220,#36221,#36222,#36223,#36224,#36225,
#36226,#36227),.UNSPECIFIED.,.F.,.F.,(4,3,3,3,3,3,3,3,3,3,3,3,3,3,3,3,3,
3,3,3,3,3,3,3,3,3,3,3,3,3,3,3,3,3,3,3,3,3,3,3,3,3,3,3,3,3,3,3,3,3,3,3,3,
3,3,3,3,4),(70.2377801861003,70.3845228516675,70.4846263171145,70.5981054941765,
70.7113829867659,70.8245484100434,70.9376465724876,71.0507221824744,71.1639017491068,
71.2771328325656,71.3905776206383,71.4773675328486,71.5908467099108,71.7041242025004,
71.8172896257782,71.9303877882225,72.0434633982096,72.1566429648422,72.2698740483012,
72.3833188363742,72.4701087485826,72.5835879256446,72.6968654182339,72.8100308415114,
72.9231290039555,73.0362046139423,73.1493841805746,73.2626152640333,73.376060052106,
73.4628499643166,73.5763291413786,73.689606633968,73.8027720572456,73.9158702196897,
74.0289458296766,74.142125396309,74.2553564797677,74.3688012678405,74.4555911800506,
74.5690703571127,74.6823478497023,74.7955132729799,74.9086114354242,75.0216870454112,
75.1348666120437,75.2480976955025,75.3615424835754,75.4483323957846,75.5618115728466,
75.675089065436,75.7882544887136,75.9013526511576,76.0144282611445,76.1276078277769,
76.2408389112356,76.3542836993083,76.4410736115186,76.5209654926159),
 .UNSPECIFIED.);
#318=B_SPLINE_CURVE_WITH_KNOTS('',3,(#36232,#36233,#36234,#36235,#36236,
#36237,#36238,#36239,#36240,#36241,#36242,#36243,#36244,#36245,#36246,#36247,
#36248,#36249,#36250,#36251,#36252,#36253,#36254,#36255,#36256,#36257,#36258,
#36259,#36260,#36261,#36262,#36263,#36264,#36265,#36266,#36267,#36268,#36269,
#36270,#36271,#36272,#36273,#36274,#36275,#36276,#36277,#36278,#36279,#36280,
#36281,#36282,#36283,#36284,#36285,#36286,#36287,#36288,#36289,#36290,#36291,
#36292,#36293,#36294,#36295,#36296,#36297,#36298,#36299,#36300,#36301,#36302,
#36303,#36304,#36305,#36306,#36307,#36308,#36309,#36310,#36311,#36312,#36313,
#36314,#36315,#36316,#36317,#36318,#36319,#36320,#36321,#36322,#36323,#36324,
#36325,#36326,#36327,#36328,#36329,#36330,#36331,#36332,#36333,#36334,#36335,
#36336,#36337,#36338,#36339,#36340,#36341,#36342,#36343,#36344,#36345,#36346,
#36347,#36348,#36349,#36350,#36351,#36352,#36353,#36354,#36355,#36356,#36357,
#36358,#36359,#36360,#36361,#36362,#36363,#36364,#36365,#36366,#36367,#36368,
#36369,#36370,#36371,#36372,#36373,#36374,#36375,#36376,#36377,#36378,#36379,
#36380,#36381,#36382,#36383,#36384,#36385,#36386,#36387,#36388,#36389,#36390,
#36391,#36392,#36393,#36394,#36395,#36396,#36397,#36398,#36399,#36400,#36401,
#36402,#36403,#36404,#36405,#36406),.UNSPECIFIED.,.F.,.F.,(4,3,3,3,3,3,
3,3,3,3,3,3,3,3,3,3,3,3,3,3,3,3,3,3,3,3,3,3,3,3,3,3,3,3,3,3,3,3,3,3,3,3,
3,3,3,3,3,3,3,3,3,3,3,3,3,3,3,3,4),(-85.7734325133808,-85.6485487228822,
-85.5231844388738,-85.3972249658836,-85.3757445531247,-85.2622653760628,
-85.1489878834734,-85.035822460196,-84.9227242977519,-84.8096486877652,
-84.6964691211328,-84.5832380376741,-84.4697932496014,-84.3830033373907,
-84.2695241603285,-84.1562466677389,-84.0430812444612,-83.9299830820169,
-83.8169074720299,-83.7037279053972,-83.5904968219383,-83.4770520338654,
-83.3902621216566,-83.2767829445946,-83.1635054520052,-83.0503400287277,
-82.9372418662836,-82.8241662562967,-82.7109866896643,-82.5977556062056,
-82.4843108181328,-82.3975209059226,-82.2840417288606,-82.1707642362712,
-82.0575988129937,-81.9445006505496,-81.8314250405627,-81.7182454739304,
-81.6050143904716,-81.4915696023989,-81.4047796901886,-81.2913005131265,
-81.178023020537,-81.0648575972594,-80.9517594348152,-80.8386838248283,
-80.7255042581958,-80.6122731747369,-80.4988283866641,-80.4120384744546,
-80.2968145660226,-80.1846668139561,-80.0726271544152,-79.9606490097494,
-79.8430485590616,-79.730983798647,-79.6188550029826,-79.5065475500105,
-79.4902472069982),.UNSPECIFIED.);
#319=B_SPLINE_CURVE_WITH_KNOTS('',3,(#36407,#36408,#36409,#36410,#36411,
#36412,#36413,#36414,#36415,#36416,#36417,#36418,#36419,#36420,#36421,#36422,
#36423,#36424,#36425,#36426,#36427,#36428,#36429,#36430,#36431,#36432,#36433,
#36434,#36435,#36436,#36437,#36438,#36439,#36440,#36441,#36442,#36443,#36444,
#36445,#36446,#36447,#36448,#36449,#36450,#36451,#36452,#36453,#36454,#36455,
#36456,#36457,#36458,#36459,#36460,#36461,#36462,#36463,#36464,#36465,#36466,
#36467,#36468,#36469,#36470,#36471,#36472,#36473,#36474,#36475,#36476,#36477,
#36478,#36479,#36480,#36481,#36482,#36483,#36484,#36485,#36486,#36487,#36488,
#36489,#36490,#36491,#36492,#36493,#36494,#36495,#36496,#36497,#36498,#36499,
#36500,#36501,#36502,#36503,#36504,#36505,#36506,#36507,#36508,#36509,#36510,
#36511,#36512,#36513,#36514,#36515,#36516,#36517,#36518,#36519,#36520,#36521,
#36522,#36523,#36524,#36525,#36526,#36527,#36528,#36529,#36530,#36531,#36532,
#36533,#36534,#36535,#36536,#36537,#36538,#36539,#36540,#36541,#36542,#36543,
#36544,#36545,#36546,#36547,#36548,#36549,#36550,#36551,#36552,#36553,#36554,
#36555,#36556,#36557,#36558,#36559,#36560,#36561,#36562,#36563,#36564,#36565,
#36566,#36567,#36568,#36569,#36570,#36571,#36572,#36573,#36574,#36575,#36576,
#36577,#36578),.UNSPECIFIED.,.F.,.F.,(4,3,3,3,3,3,3,3,3,3,3,3,3,3,3,3,3,
3,3,3,3,3,3,3,3,3,3,3,3,3,3,3,3,3,3,3,3,3,3,3,3,3,3,3,3,3,3,3,3,3,3,3,3,
3,3,3,3,4),(76.5209654930255,76.6350716598039,76.7470962172469,76.8590234384047,
76.9709000002762,77.0866287070203,77.1986165292358,77.3162156782442,77.4338148272526,
77.5472940043146,77.660571496904,77.7737369201816,77.8868350826257,77.9999106926124,
78.1130902592448,78.2263213427036,78.3397661307763,78.4265560429866,78.5400352200487,
78.6533127126381,78.7664781359158,78.8795762983599,78.9926519083468,79.1058314749793,
79.2190625584381,79.3325073465109,79.4192972587206,79.5327764357826,79.646053928372,
79.7592193516496,79.8723175140938,79.9853931240806,80.098572690713,80.2118037741718,
80.3252485622446,80.4120384744546,80.5255176515167,80.6387951441061,80.7519605673837,
80.8650587298277,80.9781343398147,81.0913139064472,81.204544989906,81.3179897779787,
81.4047796901886,81.5182588672508,81.6315363598402,81.7447017831178,81.857799945562,
81.9708755555491,82.0840551221816,82.1972862056402,82.310730993713,82.3975209059226,
82.5226125308546,82.6472946873853,82.7713407864416,82.8041507994147),
 .UNSPECIFIED.);
#320=B_SPLINE_CURVE_WITH_KNOTS('',3,(#36583,#36584,#36585,#36586,#36587,
#36588,#36589,#36590,#36591,#36592,#36593,#36594,#36595,#36596,#36597,#36598,
#36599,#36600,#36601,#36602,#36603,#36604,#36605,#36606,#36607,#36608,#36609,
#36610,#36611,#36612,#36613,#36614,#36615,#36616,#36617,#36618,#36619,#36620,
#36621,#36622,#36623,#36624,#36625,#36626,#36627,#36628,#36629,#36630,#36631,
#36632,#36633,#36634,#36635,#36636,#36637,#36638,#36639,#36640,#36641,#36642,
#36643,#36644,#36645,#36646,#36647,#36648,#36649,#36650,#36651,#36652,#36653,
#36654,#36655,#36656,#36657,#36658,#36659,#36660,#36661,#36662,#36663,#36664,
#36665,#36666,#36667,#36668,#36669,#36670,#36671,#36672,#36673,#36674,#36675,
#36676,#36677,#36678,#36679,#36680,#36681,#36682,#36683,#36684,#36685,#36686,
#36687,#36688,#36689,#36690,#36691,#36692,#36693,#36694,#36695,#36696,#36697,
#36698,#36699,#36700,#36701,#36702,#36703,#36704,#36705,#36706,#36707,#36708,
#36709,#36710,#36711,#36712,#36713,#36714,#36715,#36716,#36717,#36718,#36719,
#36720,#36721,#36722,#36723,#36724,#36725,#36726,#36727,#36728,#36729,#36730,
#36731,#36732,#36733,#36734,#36735,#36736,#36737,#36738,#36739,#36740,#36741,
#36742,#36743,#36744,#36745,#36746,#36747,#36748,#36749,#36750,#36751,#36752,
#36753,#36754,#36755,#36756,#36757),.UNSPECIFIED.,.F.,.F.,(4,3,3,3,3,3,
3,3,3,3,3,3,3,3,3,3,3,3,3,3,3,3,3,3,3,3,3,3,3,3,3,3,3,3,3,3,3,3,3,3,3,3,
3,3,3,3,3,3,3,3,3,3,3,3,3,3,3,3,4),(-92.0566178209628,-91.9445269762773,
-91.8324988389338,-91.7204870233133,-91.6083683376705,-91.4961894402909,
-91.3838092159556,-91.3321918475287,-91.2187126704667,-91.1054351778774,
-90.9922697545999,-90.8791715921557,-90.7660959821688,-90.6529164155364,
-90.5396853320778,-90.426240544005,-90.3394506317947,-90.2259714547327,
-90.1126939621431,-89.9995285388655,-89.8864303764212,-89.7733547664343,
-89.6601751998018,-89.5469441163429,-89.4334993282701,-89.3467094160607,
-89.2332302389987,-89.1199527464093,-89.0067873231316,-88.8936891606874,
-88.7806135507007,-88.6674339840682,-88.5542029006094,-88.4407581125366,
-88.3539682003267,-88.2404890232647,-88.1272115306754,-88.0140461073978,
-87.9009479449537,-87.7878723349669,-87.6746927683346,-87.561461684876,
-87.4480168968032,-87.3612269845927,-87.2477478075305,-87.1344703149409,
-87.0213048916631,-86.9082067292188,-86.7951311192316,-86.681951552599,
-86.5687204691401,-86.4552756810672,-86.3684857688587,-86.253338783512,
-86.1333622160798,-86.0186000153121,-85.9039411269373,-85.789345853808,
-85.7734325137832),.UNSPECIFIED.);
#321=B_SPLINE_CURVE_WITH_KNOTS('',3,(#36758,#36759,#36760,#36761,#36762,
#36763,#36764,#36765,#36766,#36767,#36768,#36769,#36770,#36771,#36772,#36773,
#36774,#36775,#36776,#36777,#36778,#36779,#36780,#36781,#36782,#36783,#36784,
#36785,#36786,#36787,#36788,#36789,#36790,#36791,#36792,#36793,#36794,#36795,
#36796,#36797,#36798,#36799,#36800,#36801,#36802,#36803,#36804,#36805,#36806,
#36807,#36808,#36809,#36810,#36811,#36812,#36813,#36814,#36815,#36816,#36817,
#36818,#36819,#36820,#36821,#36822,#36823,#36824,#36825,#36826,#36827,#36828,
#36829,#36830,#36831,#36832,#36833,#36834,#36835,#36836,#36837,#36838,#36839,
#36840,#36841,#36842,#36843,#36844,#36845,#36846,#36847,#36848,#36849,#36850,
#36851,#36852,#36853,#36854,#36855,#36856,#36857,#36858,#36859,#36860,#36861,
#36862,#36863,#36864,#36865,#36866,#36867,#36868,#36869,#36870,#36871,#36872,
#36873,#36874,#36875,#36876,#36877,#36878,#36879,#36880,#36881,#36882,#36883,
#36884,#36885,#36886,#36887,#36888,#36889,#36890,#36891,#36892,#36893,#36894,
#36895,#36896,#36897,#36898,#36899,#36900,#36901,#36902,#36903,#36904,#36905,
#36906,#36907,#36908,#36909,#36910,#36911,#36912,#36913,#36914,#36915,#36916,
#36917,#36918,#36919,#36920,#36921,#36922,#36923,#36924,#36925,#36926,#36927,
#36928,#36929),.UNSPECIFIED.,.F.,.F.,(4,3,3,3,3,3,3,3,3,3,3,3,3,3,3,3,3,
3,3,3,3,3,3,3,3,3,3,3,3,3,3,3,3,3,3,3,3,3,3,3,3,3,3,3,3,3,3,3,3,3,3,3,3,
3,3,3,3,4),(82.8041507997955,82.9190225628795,83.0368324525738,83.1519469049721,
83.2711045133144,83.3902621216566,83.5037412987186,83.6170187913081,83.7301842145858,
83.8432823770299,83.9563579870169,84.0695375536494,84.1827686371082,84.296213425181,
84.3830033373907,84.4964825144528,84.6097600070423,84.7229254303199,84.836023592764,
84.9490992027509,85.0622787693834,85.1755098528421,85.288954640915,85.3757445531247,
85.4892237301867,85.6025012227762,85.7156666460537,85.8287648084979,85.9418404184848,
86.0550199851173,86.168251068576,86.2816958566487,86.3684857688587,86.4819649459208,
86.5952424385102,86.7084078617878,86.821506024232,86.9345816342187,87.0477612008512,
87.1609922843101,87.2744370723829,87.3612269845927,87.4747061616547,87.5879836542441,
87.7011490775217,87.8142472399658,87.9273228499528,88.0405024165853,88.153733500044,
88.2671782881169,88.3539682003267,88.4662367419806,88.5783413179199,88.6903287715846,
88.802274943831,88.9141951257727,89.0261943465735,89.0873361069751),
 .UNSPECIFIED.);
#322=B_SPLINE_CURVE_WITH_KNOTS('',3,(#36934,#36935,#36936,#36937,#36938,
#36939,#36940,#36941,#36942,#36943,#36944,#36945,#36946,#36947,#36948,#36949,
#36950,#36951,#36952,#36953,#36954,#36955,#36956,#36957,#36958,#36959,#36960,
#36961,#36962,#36963,#36964,#36965,#36966,#36967,#36968,#36969,#36970,#36971,
#36972,#36973,#36974,#36975,#36976,#36977,#36978,#36979,#36980,#36981,#36982,
#36983,#36984,#36985,#36986,#36987,#36988,#36989,#36990,#36991,#36992,#36993,
#36994,#36995,#36996,#36997,#36998,#36999,#37000,#37001,#37002,#37003,#37004,
#37005,#37006,#37007,#37008,#37009,#37010,#37011,#37012,#37013,#37014,#37015,
#37016,#37017,#37018,#37019,#37020,#37021,#37022,#37023,#37024,#37025,#37026,
#37027,#37028,#37029,#37030,#37031,#37032,#37033,#37034,#37035,#37036,#37037,
#37038,#37039,#37040,#37041,#37042,#37043,#37044,#37045,#37046,#37047,#37048,
#37049,#37050,#37051,#37052,#37053,#37054,#37055,#37056,#37057,#37058,#37059,
#37060,#37061,#37062,#37063,#37064,#37065,#37066,#37067,#37068,#37069,#37070,
#37071,#37072,#37073,#37074,#37075,#37076,#37077,#37078,#37079,#37080,#37081,
#37082,#37083,#37084,#37085,#37086,#37087,#37088,#37089,#37090,#37091,#37092,
#37093,#37094,#37095,#37096,#37097,#37098,#37099,#37100,#37101,#37102,#37103,
#37104,#37105),.UNSPECIFIED.,.F.,.F.,(4,3,3,3,3,3,3,3,3,3,3,3,3,3,3,3,3,
3,3,3,3,3,3,3,3,3,3,3,3,3,3,3,3,3,3,3,3,3,3,3,3,3,3,3,3,3,3,3,3,3,3,3,3,
3,3,3,3,4),(-98.3398031281424,-98.2813803576668,-98.1679011806047,-98.054623688015,
-97.9414582647372,-97.828360102293,-97.7152844923059,-97.6021049256733,
-97.4888738422143,-97.3754290541414,-97.2886391419328,-97.1751599648709,
-97.0618824722816,-96.9487170490041,-96.8356188865602,-96.7225432765735,
-96.6093637099411,-96.4961326264825,-96.3826878384099,-96.2958979261987,
-96.1824187491366,-96.0691412565472,-95.9559758332695,-95.8428776708253,
-95.7298020608384,-95.6166224942059,-95.5033914107471,-95.3899466226742,
-95.3031567104647,-95.1896775334027,-95.0764000408132,-94.9632346175356,
-94.8501364550915,-94.7370608451046,-94.6238812784722,-94.5106501950134,
-94.3972054069406,-94.3104154947307,-94.1969363176687,-94.0836588250792,
-93.9704934018016,-93.8573952393575,-93.7443196293706,-93.6311400627381,
-93.5179089792793,-93.4044641912065,-93.3176742789967,-93.2041951019347,
-93.0909176093452,-92.9777521860676,-92.8646540236235,-92.7515784136366,
-92.6383988470042,-92.5251677635455,-92.4117229754727,-92.3249330632627,
-92.1828327203833,-92.0566178213547),.UNSPECIFIED.);
#323=B_SPLINE_CURVE_WITH_KNOTS('',3,(#37106,#37107,#37108,#37109,#37110,
#37111,#37112,#37113,#37114,#37115,#37116,#37117,#37118,#37119,#37120,#37121,
#37122,#37123,#37124,#37125,#37126,#37127,#37128,#37129,#37130,#37131,#37132,
#37133,#37134,#37135,#37136,#37137,#37138,#37139,#37140,#37141,#37142,#37143,
#37144,#37145,#37146,#37147,#37148,#37149,#37150,#37151,#37152,#37153,#37154,
#37155,#37156,#37157,#37158,#37159,#37160,#37161,#37162,#37163,#37164,#37165,
#37166,#37167,#37168,#37169,#37170,#37171,#37172,#37173,#37174,#37175,#37176,
#37177,#37178,#37179,#37180,#37181,#37182,#37183,#37184,#37185,#37186,#37187,
#37188,#37189,#37190,#37191,#37192,#37193,#37194,#37195,#37196,#37197,#37198,
#37199,#37200,#37201,#37202,#37203,#37204,#37205,#37206,#37207,#37208,#37209,
#37210,#37211,#37212,#37213,#37214,#37215,#37216,#37217,#37218,#37219,#37220,
#37221,#37222,#37223,#37224,#37225,#37226,#37227,#37228,#37229,#37230,#37231,
#37232,#37233,#37234,#37235,#37236,#37237,#37238,#37239,#37240,#37241,#37242,
#37243,#37244,#37245,#37246,#37247,#37248,#37249,#37250,#37251,#37252,#37253,
#37254,#37255,#37256,#37257,#37258,#37259,#37260,#37261,#37262,#37263,#37264,
#37265,#37266,#37267,#37268,#37269,#37270,#37271,#37272,#37273,#37274,#37275,
#37276,#37277),.UNSPECIFIED.,.F.,.F.,(4,3,3,3,3,3,3,3,3,3,3,3,3,3,3,3,3,
3,3,3,3,3,3,3,3,3,3,3,3,3,3,3,3,3,3,3,3,3,3,3,3,3,3,3,3,3,3,3,3,3,3,3,3,
3,3,3,3,4),(89.0873361075773,89.2312652478138,89.3467094160607,89.4601885931227,
89.5734660857121,89.6866315089897,89.7997296714338,89.9128052814208,90.0259848480532,
90.1392159315119,90.2526607195847,90.3394506317947,90.4529298088567,90.5662073014462,
90.6793727247237,90.7924708871679,90.9055464971547,91.0187260637872,91.131957147246,
91.2454019353187,91.3321918475287,91.4456710245907,91.5589485171802,91.6721139404578,
91.7852121029019,91.8982877128888,92.0114672795213,92.1246983629801,92.2381431510529,
92.3249330632627,92.4384122403247,92.5516897329142,92.6648551561918,92.777953318636,
92.8910289286229,93.0042084952553,93.1174395787141,93.2308843667869,93.3176742789967,
93.4311534560588,93.5444309486482,93.6575963719257,93.7706945343698,93.8837701443567,
93.9969497109891,94.1101807944479,94.2236255825206,94.3104154947307,94.4238946717927,
94.5371721643822,94.6503375876598,94.7634357501039,94.8765113600907,94.9896909267232,
95.1029220101819,95.2163667982547,95.3031567104647,95.3705214141547),
 .UNSPECIFIED.);
#324=B_SPLINE_CURVE_WITH_KNOTS('',3,(#37282,#37283,#37284,#37285,#37286,
#37287,#37288,#37289,#37290,#37291,#37292,#37293,#37294,#37295,#37296,#37297,
#37298,#37299,#37300,#37301,#37302,#37303,#37304,#37305,#37306,#37307,#37308,
#37309,#37310,#37311,#37312,#37313,#37314,#37315,#37316,#37317,#37318,#37319,
#37320,#37321,#37322,#37323,#37324,#37325,#37326,#37327,#37328,#37329,#37330,
#37331,#37332,#37333,#37334,#37335,#37336,#37337,#37338,#37339,#37340,#37341,
#37342,#37343,#37344,#37345,#37346,#37347,#37348,#37349,#37350,#37351,#37352,
#37353,#37354,#37355,#37356,#37357,#37358,#37359,#37360,#37361,#37362,#37363,
#37364,#37365,#37366,#37367,#37368,#37369,#37370,#37371,#37372,#37373,#37374,
#37375,#37376,#37377,#37378,#37379,#37380,#37381,#37382,#37383,#37384,#37385,
#37386,#37387,#37388,#37389,#37390,#37391,#37392,#37393,#37394,#37395,#37396,
#37397,#37398,#37399,#37400,#37401,#37402,#37403,#37404,#37405,#37406,#37407,
#37408,#37409,#37410,#37411,#37412,#37413,#37414,#37415,#37416,#37417,#37418,
#37419,#37420,#37421,#37422,#37423,#37424,#37425,#37426,#37427,#37428,#37429,
#37430,#37431,#37432,#37433,#37434,#37435,#37436,#37437,#37438,#37439,#37440,
#37441,#37442,#37443,#37444,#37445,#37446,#37447,#37448,#37449,#37450,#37451,
#37452,#37453),.UNSPECIFIED.,.F.,.F.,(4,3,3,3,3,3,3,3,3,3,3,3,3,3,3,3,3,
3,3,3,3,3,3,3,3,3,3,3,3,3,3,3,3,3,3,3,3,3,3,3,3,3,3,3,3,3,3,3,3,3,3,3,3,
3,3,3,3,4),(-104.622988434897,-104.497045431599,-104.367436541835,-104.237827652071,
-104.124348475011,-104.011070982423,-103.897905559147,-103.784807396705,
-103.67173178672,-103.55855222009,-103.445321136633,-103.331876348562,-103.245086436337,
-103.131607259276,-103.018329766687,-102.90516434341,-102.792066180966,
-102.67899057098,-102.565811004348,-102.45257992089,-102.339135132818,-102.252345220603,
-102.13886604354,-102.02558855095,-101.912423127672,-101.799324965227,-101.686249355239,
-101.573069788606,-101.459838705146,-101.346393917072,-101.259604004869,
-101.146124827807,-101.032847335218,-100.919681911941,-100.806583749497,
-100.69350813951,-100.580328572878,-100.46709748942,-100.353652701347,-100.266862789135,
-100.153383612073,-100.040106119484,-99.9269406962061,-99.813842533762,
-99.7007669237751,-99.5875873571428,-99.4743562736841,-99.3609114856114,
-99.2741215734008,-99.1573317677877,-99.045033056258,-98.9328421780367,
-98.8207127649638,-98.7085985481294,-98.5963824897407,-98.4841051256357,
-98.3716413638913,-98.3398031284962),.UNSPECIFIED.);
#325=B_SPLINE_CURVE_WITH_KNOTS('',3,(#37454,#37455,#37456,#37457,#37458,
#37459,#37460,#37461,#37462,#37463,#37464,#37465,#37466,#37467,#37468,#37469,
#37470,#37471,#37472,#37473,#37474,#37475,#37476,#37477,#37478,#37479,#37480,
#37481,#37482,#37483,#37484,#37485,#37486,#37487,#37488,#37489,#37490,#37491,
#37492,#37493,#37494,#37495,#37496,#37497,#37498,#37499,#37500,#37501,#37502,
#37503,#37504,#37505,#37506,#37507,#37508,#37509,#37510,#37511,#37512,#37513,
#37514,#37515,#37516,#37517,#37518,#37519,#37520,#37521,#37522,#37523,#37524,
#37525,#37526,#37527,#37528,#37529,#37530,#37531,#37532,#37533,#37534,#37535,
#37536,#37537,#37538,#37539,#37540,#37541,#37542,#37543,#37544,#37545,#37546,
#37547,#37548,#37549,#37550,#37551,#37552,#37553,#37554,#37555,#37556,#37557,
#37558,#37559,#37560,#37561,#37562,#37563,#37564,#37565,#37566,#37567,#37568,
#37569,#37570,#37571,#37572,#37573,#37574,#37575,#37576,#37577,#37578,#37579,
#37580,#37581,#37582,#37583,#37584,#37585,#37586,#37587,#37588,#37589,#37590,
#37591,#37592,#37593,#37594,#37595,#37596,#37597,#37598,#37599,#37600,#37601,
#37602,#37603,#37604,#37605,#37606,#37607,#37608,#37609,#37610,#37611,#37612,
#37613,#37614,#37615,#37616,#37617,#37618,#37619,#37620,#37621,#37622,#37623,
#37624,#37625,#37626,#37627,#37628),.UNSPECIFIED.,.F.,.F.,(4,3,3,3,3,3,
3,3,3,3,3,3,3,3,3,3,3,3,3,3,3,3,3,3,3,3,3,3,3,3,3,3,3,3,3,3,3,3,3,3,3,3,
3,3,3,3,3,3,3,3,3,3,3,3,3,3,3,3,4),(95.3705214145325,95.4861934784908,95.5983624149504,
95.7104313611073,95.8224468167166,95.934455192268,96.0465754703724,96.1587643887504,
96.2711448642132,96.2958979261987,96.4093771032606,96.52265459585,96.6358200191276,
96.7489181815718,96.8619937915587,96.9751733581911,97.0884044416497,97.2018492297225,
97.2886391419327,97.4021183189946,97.515395811584,97.6285612348617,97.7416593973056,
97.8547350072924,97.9679145739248,98.0811456573836,98.1945904454564,98.2813803576667,
98.3948595347287,98.5081370273182,98.6213024505959,98.73440061304,98.847476223027,
98.9606557896595,99.0738868731184,99.1873316611913,99.2741215734008,99.3876007504629,
99.5008782430525,99.6140436663302,99.7271418287744,99.8402174387616,99.9533970053941,
100.066628088853,100.180072876926,100.266862789135,100.380341966197,100.493619458786,
100.606784882064,100.719883044508,100.832958654494,100.946138221127,101.059369304585,
101.172814092658,101.259604004869,101.385777191572,101.511498690172,101.636515904144,
101.653706720924),.UNSPECIFIED.);
#326=B_SPLINE_CURVE_WITH_KNOTS('',3,(#37633,#37634,#37635,#37636,#37637,
#37638,#37639,#37640,#37641,#37642,#37643,#37644,#37645,#37646,#37647,#37648,
#37649,#37650,#37651,#37652,#37653,#37654,#37655,#37656,#37657,#37658,#37659,
#37660,#37661,#37662,#37663,#37664,#37665,#37666,#37667,#37668,#37669,#37670,
#37671,#37672,#37673,#37674,#37675,#37676,#37677,#37678,#37679,#37680,#37681,
#37682,#37683,#37684,#37685,#37686,#37687,#37688,#37689,#37690,#37691,#37692,
#37693,#37694,#37695,#37696,#37697,#37698,#37699,#37700,#37701,#37702,#37703,
#37704,#37705,#37706,#37707,#37708,#37709,#37710,#37711,#37712,#37713,#37714,
#37715,#37716,#37717,#37718,#37719,#37720,#37721,#37722,#37723,#37724,#37725,
#37726,#37727,#37728,#37729,#37730,#37731,#37732,#37733,#37734,#37735,#37736,
#37737,#37738,#37739,#37740,#37741,#37742,#37743,#37744,#37745,#37746,#37747,
#37748,#37749,#37750,#37751,#37752,#37753,#37754,#37755,#37756,#37757,#37758,
#37759,#37760,#37761,#37762,#37763,#37764,#37765,#37766,#37767,#37768,#37769,
#37770,#37771,#37772,#37773,#37774,#37775,#37776,#37777,#37778,#37779,#37780,
#37781,#37782,#37783,#37784,#37785,#37786,#37787,#37788,#37789,#37790,#37791,
#37792,#37793,#37794,#37795,#37796,#37797,#37798,#37799,#37800,#37801,#37802,
#37803,#37804,#37805,#37806,#37807),.UNSPECIFIED.,.F.,.F.,(4,3,3,3,3,3,
3,3,3,3,3,3,3,3,3,3,3,3,3,3,3,3,3,3,3,3,3,3,3,3,3,3,3,3,3,3,3,3,3,3,3,3,
3,3,3,3,3,3,3,3,3,3,3,3,3,3,3,3,4),(-110.906173742502,-110.793939498286,
-110.681759990839,-110.569589080838,-110.457304897499,-110.344954035642,
-110.232404211857,-110.194274946475,-110.080795769476,-109.967518276951,
-109.854352853737,-109.741254691356,-109.628179081433,-109.514999514863,
-109.401768431466,-109.288323643454,-109.201533730741,-109.088054553733,
-108.974777061199,-108.861611637978,-108.748513475592,-108.635437865664,
-108.522258299091,-108.409027215692,-108.295582427679,-108.208792515007,
-108.095313337899,-107.982035845262,-107.868870421936,-107.755772259443,
-107.642696649408,-107.529517082726,-107.416285999217,-107.302841211095,
-107.216051299273,-107.102572122223,-106.989294629645,-106.87612920638,
-106.763031043948,-106.649955433973,-106.536775867352,-106.423544783906,
-106.310099995844,-106.223310083539,-106.109830906482,-105.996553413898,
-105.883387990627,-105.770289828188,-105.657214218208,-105.544034651581,
-105.430803568129,-105.317358780062,-105.230568867805,-105.115803842946,
-105.001231835846,-104.886830152399,-104.772527199561,-104.658275035006,
-104.622988435322),.UNSPECIFIED.);
#327=B_SPLINE_CURVE_WITH_KNOTS('',3,(#37808,#37809,#37810,#37811,#37812,
#37813,#37814,#37815,#37816,#37817,#37818,#37819,#37820,#37821,#37822,#37823,
#37824,#37825,#37826,#37827,#37828,#37829,#37830,#37831,#37832,#37833,#37834,
#37835,#37836,#37837,#37838,#37839,#37840,#37841,#37842,#37843,#37844,#37845,
#37846,#37847,#37848,#37849,#37850,#37851,#37852,#37853,#37854,#37855,#37856,
#37857,#37858,#37859,#37860,#37861,#37862,#37863,#37864,#37865,#37866,#37867,
#37868,#37869,#37870,#37871,#37872,#37873,#37874,#37875,#37876,#37877,#37878,
#37879,#37880,#37881,#37882,#37883,#37884,#37885,#37886,#37887,#37888,#37889,
#37890,#37891,#37892,#37893,#37894,#37895,#37896,#37897,#37898,#37899,#37900,
#37901,#37902,#37903,#37904,#37905,#37906,#37907,#37908,#37909,#37910,#37911,
#37912,#37913,#37914,#37915,#37916,#37917,#37918,#37919,#37920,#37921,#37922,
#37923,#37924,#37925,#37926,#37927,#37928,#37929,#37930,#37931,#37932,#37933,
#37934,#37935,#37936,#37937,#37938,#37939,#37940,#37941,#37942,#37943,#37944,
#37945,#37946,#37947,#37948,#37949,#37950,#37951,#37952,#37953,#37954,#37955,
#37956,#37957,#37958,#37959,#37960,#37961,#37962,#37963,#37964,#37965,#37966,
#37967,#37968,#37969,#37970,#37971,#37972,#37973,#37974,#37975,#37976,#37977,
#37978,#37979,#37980,#37981,#37982),.UNSPECIFIED.,.F.,.F.,(4,3,3,3,3,3,
3,3,3,3,3,3,3,3,3,3,3,3,3,3,3,3,3,3,3,3,3,3,3,3,3,3,3,3,3,3,3,3,3,3,3,3,
3,3,3,3,3,3,3,3,3,3,3,3,3,3,3,3,4),(101.653706721334,101.768208363524,101.882752096176,
101.997465726927,102.112280389874,102.227321629928,102.252345220603,102.365824397664,
102.479101890253,102.59226731353,102.705365475974,102.81844108596,102.931620652592,
103.04485173605,103.158296524122,103.245086436337,103.358565613397,103.471843105984,
103.58500852926,103.698106691702,103.811182301686,103.924361868317,104.037592951773,
104.151037739844,104.237827652071,104.35130682914,104.464584321736,104.57774974502,
104.69084790747,104.803923517464,104.917103084102,105.030334167568,105.143778955646,
105.230568867805,105.344048044861,105.457325537444,105.570490960716,105.683589123154,
105.796664733135,105.909844299762,106.023075383215,106.136520171283,106.223310083539,
106.336789260589,106.450066753167,106.563232176432,106.676330338865,106.789405948839,
106.902585515459,107.015816598906,107.129261386967,107.216051299273,107.328469817482,
107.440722785259,107.552856842165,107.664943651989,107.777002830859,107.889130021498,
107.936892028514),.UNSPECIFIED.);
#328=B_SPLINE_CURVE_WITH_KNOTS('',3,(#37987,#37988,#37989,#37990,#37991,
#37992,#37993,#37994,#37995,#37996,#37997,#37998,#37999,#38000,#38001,#38002,
#38003,#38004,#38005,#38006,#38007,#38008,#38009,#38010,#38011,#38012,#38013,
#38014,#38015,#38016,#38017,#38018,#38019,#38020,#38021,#38022,#38023,#38024,
#38025,#38026,#38027,#38028,#38029,#38030,#38031,#38032,#38033,#38034,#38035,
#38036,#38037,#38038,#38039,#38040,#38041,#38042,#38043,#38044,#38045,#38046,
#38047,#38048,#38049,#38050,#38051,#38052,#38053,#38054,#38055,#38056,#38057,
#38058,#38059,#38060,#38061,#38062,#38063,#38064,#38065,#38066,#38067,#38068,
#38069,#38070,#38071,#38072,#38073,#38074,#38075,#38076,#38077,#38078,#38079,
#38080,#38081,#38082,#38083,#38084,#38085,#38086,#38087,#38088,#38089,#38090,
#38091,#38092,#38093,#38094,#38095,#38096,#38097,#38098,#38099,#38100,#38101,
#38102,#38103,#38104,#38105,#38106,#38107,#38108,#38109,#38110,#38111,#38112,
#38113,#38114,#38115,#38116,#38117,#38118,#38119,#38120,#38121,#38122,#38123,
#38124,#38125,#38126,#38127,#38128,#38129,#38130,#38131,#38132,#38133,#38134,
#38135,#38136,#38137,#38138,#38139,#38140,#38141,#38142,#38143,#38144,#38145,
#38146,#38147,#38148,#38149,#38150,#38151,#38152,#38153,#38154,#38155,#38156,
#38157,#38158),.UNSPECIFIED.,.F.,.F.,(4,3,3,3,3,3,3,3,3,3,3,3,3,3,3,3,3,
3,3,3,3,3,3,3,3,3,3,3,3,3,3,3,3,3,3,3,3,3,3,3,3,3,3,3,3,3,3,3,3,3,3,3,3,
3,3,3,3,4),(-117.189359049681,-117.143463456613,-117.029984262168,-116.916706751875,
-116.803541310712,-116.690443130233,-116.577367502095,-116.464187917276,
-116.350956815583,-116.237512009426,-116.150722240879,-116.037243064179,
-115.923965571878,-115.810800148842,-115.697701986594,-115.584626376755,
-115.471446810197,-115.35821572677,-115.244770938662,-115.157981025145,
-115.044501852382,-114.931224364215,-114.818058945434,-114.70496078755,
-114.59188518218,-114.478705620214,-114.365474541458,-114.252029758087,
-114.165239809411,-114.051760629865,-113.938483134742,-113.825317708902,
-113.712219543871,-113.599143931279,-113.485964362032,-113.37273327595,
-113.259288485273,-113.172498593677,-113.059019416883,-112.945741924558,
-112.832576501541,-112.719478339354,-112.606402729621,-112.493223163233,
-112.379992080016,-112.266547292174,-112.179757377943,-112.066278201375,
-111.953000709295,-111.839835286535,-111.726737124618,-111.613661515164,
-111.500481949072,-111.387250866159,-111.273806078632,-111.187016162209,
-111.04659495261,-110.906173743011),.UNSPECIFIED.);
#329=B_SPLINE_CURVE_WITH_KNOTS('',3,(#38159,#38160,#38161,#38162,#38163,
#38164,#38165,#38166,#38167,#38168,#38169,#38170,#38171,#38172,#38173,#38174,
#38175,#38176,#38177,#38178,#38179,#38180,#38181,#38182,#38183,#38184,#38185,
#38186,#38187,#38188,#38189,#38190,#38191,#38192,#38193,#38194,#38195,#38196,
#38197,#38198,#38199,#38200,#38201,#38202,#38203,#38204,#38205,#38206,#38207,
#38208,#38209,#38210,#38211,#38212,#38213,#38214,#38215,#38216,#38217,#38218,
#38219,#38220,#38221,#38222,#38223,#38224,#38225,#38226,#38227,#38228,#38229,
#38230,#38231,#38232,#38233,#38234,#38235,#38236,#38237,#38238,#38239,#38240,
#38241,#38242,#38243,#38244,#38245,#38246,#38247,#38248,#38249,#38250,#38251,
#38252,#38253,#38254,#38255,#38256,#38257,#38258,#38259,#38260,#38261,#38262,
#38263,#38264,#38265,#38266,#38267,#38268,#38269,#38270,#38271,#38272,#38273,
#38274,#38275,#38276,#38277,#38278,#38279,#38280,#38281,#38282,#38283,#38284,
#38285,#38286,#38287,#38288,#38289,#38290,#38291,#38292,#38293,#38294,#38295,
#38296,#38297,#38298,#38299,#38300,#38301,#38302,#38303,#38304,#38305,#38306,
#38307,#38308,#38309,#38310,#38311,#38312,#38313,#38314,#38315,#38316,#38317,
#38318,#38319,#38320,#38321,#38322,#38323,#38324,#38325,#38326,#38327,#38328,
#38329,#38330),.UNSPECIFIED.,.F.,.F.,(4,3,3,3,3,3,3,3,3,3,3,3,3,3,3,3,3,
3,3,3,3,3,3,3,3,3,3,3,3,3,3,3,3,3,3,3,3,3,3,3,3,3,3,3,3,3,3,3,3,3,3,3,3,
3,3,3,3,4),(107.936892028941,108.078296556603,108.208792515007,108.322271692009,
108.435549184539,108.548714607757,108.661812770142,108.774888380071,108.888067946647,
109.00129903005,109.114743818068,109.201533730741,109.315012907743,109.428290400271,
109.541455823486,109.654553985868,109.767629595792,109.88080916236,109.994040245755,
110.107485033765,110.194274946475,110.307754123899,110.42103161685,110.53419704049,
110.647295203295,110.760370813642,110.87355038063,110.986781464442,111.10022625286,
111.187016162209,111.300495338727,111.413772830776,111.526938253515,111.640036415426,
111.753112024883,111.866291590997,111.979522673944,112.092967461519,112.179757377943,
112.293236554778,112.40651404713,112.519679470164,112.632777632358,112.745853242091,
112.859032808463,112.972263891657,113.085708679464,113.172498593677,113.285977773331,
113.399255268519,113.512420694398,113.625518859441,113.73859447202,113.851774041214,
113.96500512722,114.078449917787,114.165239809411,114.220077335693),
 .UNSPECIFIED.);
#330=B_SPLINE_CURVE_WITH_KNOTS('',3,(#38335,#38336,#38337,#38338,#38339,
#38340,#38341,#38342,#38343,#38344,#38345,#38346,#38347,#38348,#38349,#38350,
#38351,#38352,#38353,#38354,#38355,#38356,#38357,#38358,#38359,#38360,#38361,
#38362,#38363,#38364,#38365,#38366,#38367,#38368,#38369,#38370,#38371,#38372,
#38373,#38374,#38375,#38376,#38377,#38378,#38379,#38380,#38381,#38382,#38383,
#38384,#38385,#38386,#38387,#38388,#38389,#38390,#38391,#38392,#38393,#38394,
#38395,#38396,#38397,#38398,#38399,#38400,#38401,#38402,#38403,#38404,#38405,
#38406,#38407,#38408,#38409,#38410,#38411,#38412,#38413,#38414,#38415,#38416,
#38417,#38418,#38419,#38420,#38421,#38422,#38423,#38424,#38425,#38426,#38427,
#38428,#38429,#38430,#38431,#38432,#38433,#38434,#38435,#38436,#38437,#38438,
#38439,#38440,#38441,#38442,#38443,#38444,#38445,#38446,#38447,#38448,#38449,
#38450,#38451,#38452,#38453,#38454,#38455,#38456,#38457,#38458,#38459,#38460,
#38461,#38462,#38463,#38464,#38465,#38466,#38467,#38468,#38469,#38470,#38471,
#38472,#38473,#38474,#38475,#38476,#38477,#38478,#38479,#38480,#38481,#38482,
#38483,#38484,#38485,#38486,#38487,#38488,#38489,#38490,#38491,#38492,#38493,
#38494,#38495,#38496,#38497,#38498,#38499,#38500,#38501,#38502,#38503,#38504,
#38505,#38506),.UNSPECIFIED.,.F.,.F.,(4,3,3,3,3,3,3,3,3,3,3,3,3,3,3,3,3,
3,3,3,3,3,3,3,3,3,3,3,3,3,3,3,3,3,3,3,3,3,3,3,3,3,3,3,3,3,3,3,3,3,3,3,3,
3,3,3,3,4),(-123.472544356421,-123.345470616914,-123.217416259133,-123.099910751017,
-122.986430819344,-122.873152561787,-122.759986367799,-122.646887430315,
-122.533811042367,-122.420630699507,-122.30739883959,-122.193953284424,
-122.107169535283,-121.993690187015,-121.880412514652,-121.767246906492,
-121.654148554392,-121.541072750307,-121.427892984211,-121.314661698002,
-121.201216704285,-121.114428319549,-121.000949433042,-120.887672238451,
-120.774507117501,-120.661409261157,-120.548333960498,-120.435154705727,
-120.321923936018,-120.208479460878,-120.121687103815,-120.008207809519,
-119.894930197774,-119.781764654257,-119.668666370711,-119.555590638977,
-119.442410950579,-119.329179745155,-119.21573483632,-119.128945888081,
-119.015466700982,-118.902189197496,-118.789023762804,-118.675925588448,
-118.562849966072,-118.449670386406,-118.336439289535,-118.222994487593,
-118.136204672347,-118.017848969589,-117.905379905631,-117.793018509986,
-117.680718661559,-117.568434336959,-117.456046233179,-117.34359766165,
-117.23095665154,-117.189359050281),.UNSPECIFIED.);
#331=B_SPLINE_CURVE_WITH_KNOTS('',3,(#38507,#38508,#38509,#38510,#38511,
#38512,#38513,#38514,#38515,#38516,#38517,#38518,#38519,#38520,#38521,#38522,
#38523,#38524,#38525,#38526,#38527,#38528,#38529,#38530,#38531,#38532,#38533,
#38534,#38535,#38536,#38537,#38538,#38539,#38540,#38541,#38542,#38543,#38544,
#38545,#38546,#38547,#38548,#38549,#38550,#38551,#38552,#38553,#38554,#38555,
#38556,#38557,#38558,#38559,#38560,#38561,#38562,#38563,#38564,#38565,#38566,
#38567,#38568,#38569,#38570,#38571,#38572,#38573,#38574,#38575,#38576,#38577,
#38578,#38579,#38580,#38581,#38582,#38583,#38584,#38585,#38586,#38587,#38588,
#38589,#38590,#38591,#38592,#38593,#38594,#38595,#38596,#38597,#38598,#38599,
#38600,#38601,#38602,#38603,#38604,#38605,#38606,#38607,#38608,#38609,#38610,
#38611,#38612,#38613,#38614,#38615,#38616,#38617,#38618,#38619,#38620,#38621,
#38622,#38623,#38624,#38625,#38626,#38627,#38628,#38629,#38630,#38631,#38632,
#38633,#38634,#38635,#38636,#38637,#38638,#38639,#38640,#38641,#38642,#38643,
#38644,#38645,#38646,#38647,#38648,#38649,#38650,#38651,#38652,#38653,#38654,
#38655,#38656,#38657,#38658,#38659,#38660,#38661,#38662,#38663,#38664,#38665,
#38666,#38667,#38668,#38669,#38670,#38671,#38672,#38673,#38674,#38675,#38676,
#38677,#38678),.UNSPECIFIED.,.F.,.F.,(4,3,3,3,3,3,3,3,3,3,3,3,3,3,3,3,3,
3,3,3,3,3,3,3,3,3,3,3,3,3,3,3,3,3,3,3,3,3,3,3,3,3,3,3,3,3,3,3,3,3,3,3,3,
3,3,3,3,4),(114.220077336359,114.337315297457,114.449646959165,114.561876301729,
114.674049612068,114.786213085774,114.898487007242,115.010826687181,115.1233612464,
115.157981025145,115.271460202267,115.384737694835,115.497903118042,115.611001280366,
115.724076890186,115.83725645658,115.950487539759,116.063932327492,116.150722240879,
116.264201435928,116.377478946583,116.49064438796,116.603742568506,116.716818196563,
116.829997781074,116.943228882334,117.056673687856,117.143463456613,117.256942594808,
117.370220048676,117.483385433349,117.596483557373,117.709559129191,117.822738658342,
117.935969704643,118.04941445655,118.136204672347,118.2496838634,118.362961369367,
118.476126805638,118.589224980674,118.702300602833,118.815480180898,118.928711275397,
119.042156073739,119.128945888081,119.242425185255,119.355702798712,119.468868343228,
119.581966627062,119.695042358373,119.808222045258,119.921453248561,120.034898154307,
120.121687103815,120.249019832346,120.376141237394,120.503262642443),
 .UNSPECIFIED.);
#332=B_SPLINE_CURVE_WITH_KNOTS('',3,(#38683,#38684,#38685,#38686,#38687,
#38688,#38689,#38690,#38691,#38692,#38693,#38694,#38695,#38696,#38697,#38698,
#38699,#38700,#38701,#38702,#38703,#38704,#38705,#38706,#38707,#38708,#38709,
#38710,#38711,#38712,#38713,#38714,#38715,#38716,#38717,#38718,#38719,#38720,
#38721,#38722,#38723,#38724,#38725,#38726,#38727,#38728,#38729,#38730,#38731,
#38732,#38733,#38734,#38735,#38736,#38737,#38738,#38739,#38740,#38741,#38742,
#38743,#38744,#38745,#38746,#38747,#38748,#38749,#38750,#38751,#38752,#38753,
#38754,#38755,#38756,#38757,#38758,#38759,#38760,#38761,#38762,#38763,#38764,
#38765,#38766,#38767,#38768,#38769,#38770,#38771,#38772,#38773,#38774,#38775,
#38776,#38777,#38778,#38779,#38780,#38781,#38782,#38783,#38784,#38785,#38786,
#38787,#38788,#38789,#38790,#38791,#38792,#38793,#38794,#38795,#38796,#38797,
#38798,#38799,#38800,#38801,#38802,#38803,#38804,#38805,#38806,#38807,#38808,
#38809,#38810,#38811,#38812,#38813,#38814,#38815,#38816,#38817,#38818,#38819,
#38820,#38821,#38822,#38823,#38824,#38825,#38826,#38827,#38828,#38829,#38830,
#38831,#38832,#38833,#38834,#38835,#38836,#38837,#38838,#38839,#38840,#38841,
#38842,#38843,#38844,#38845,#38846,#38847,#38848,#38849,#38850,#38851,#38852,
#38853,#38854,#38855,#38856,#38857),.UNSPECIFIED.,.F.,.F.,(4,3,3,3,3,3,
3,3,3,3,3,3,3,3,3,3,3,3,3,3,3,3,3,3,3,3,3,3,3,3,3,3,3,3,3,3,3,3,3,3,3,3,
3,3,3,3,3,3,3,3,3,3,3,3,3,3,3,3,4),(-129.75572966404,-129.643438869128,
-129.531194980693,-129.418952001974,-129.306589037397,-129.19415280237,
-129.081519012781,-129.056358045421,-128.94285419673,-128.829551963253,
-128.716361776385,-128.603238873322,-128.49013859133,-128.376934659812,
-128.263679344804,-128.150210849827,-128.063616829687,-127.950117757225,
-127.836819680326,-127.723633266823,-127.610513746718,-127.497416449608,
-127.384214857179,-127.270961525952,-127.157494402443,-127.070875613953,
-126.957413872304,-126.844154214211,-126.731006856018,-126.617926956249,
-126.504869773821,-126.391708743247,-126.278496284715,-126.165070034802,
-126.078134398219,-125.964650672452,-125.851368586728,-125.738198546723,
-125.625095752438,-125.512015503945,-125.398831325955,-125.285595639135,
-125.17214631871,-125.085393182485,-124.971912019062,-124.85863246125,-124.745464926045,
-124.632364608826,-124.519286805016,-124.406105001344,-124.292871653395,
-124.17942458386,-124.092651966751,-123.978244662877,-123.864025778459,
-123.74996712899,-123.636001849746,-123.522073439414,-123.472544356861),
 .UNSPECIFIED.);
#333=B_SPLINE_CURVE_WITH_KNOTS('',3,(#38858,#38859,#38860,#38861,#38862,
#38863,#38864,#38865,#38866,#38867,#38868,#38869,#38870,#38871,#38872,#38873,
#38874,#38875,#38876,#38877,#38878,#38879,#38880,#38881,#38882,#38883,#38884,
#38885,#38886,#38887,#38888,#38889,#38890,#38891,#38892,#38893,#38894,#38895,
#38896,#38897,#38898,#38899,#38900,#38901,#38902,#38903,#38904,#38905,#38906,
#38907,#38908,#38909,#38910,#38911,#38912,#38913,#38914,#38915,#38916,#38917,
#38918,#38919,#38920,#38921,#38922,#38923,#38924,#38925,#38926,#38927,#38928,
#38929,#38930,#38931,#38932,#38933,#38934,#38935,#38936,#38937,#38938,#38939,
#38940,#38941,#38942,#38943,#38944,#38945,#38946,#38947,#38948,#38949,#38950,
#38951,#38952,#38953,#38954,#38955,#38956,#38957,#38958,#38959,#38960,#38961,
#38962,#38963,#38964,#38965,#38966,#38967,#38968,#38969,#38970,#38971,#38972,
#38973,#38974,#38975,#38976,#38977,#38978,#38979,#38980,#38981,#38982,#38983,
#38984,#38985,#38986,#38987,#38988,#38989,#38990,#38991,#38992,#38993,#38994,
#38995,#38996,#38997,#38998,#38999,#39000,#39001,#39002,#39003,#39004,#39005,
#39006,#39007,#39008,#39009,#39010,#39011,#39012,#39013,#39014,#39015,#39016,
#39017,#39018,#39019,#39020,#39021,#39022,#39023,#39024,#39025,#39026,#39027,
#39028,#39029,#39030,#39031,#39032),.UNSPECIFIED.,.F.,.F.,(4,3,3,3,3,3,
3,3,3,3,3,3,3,3,3,3,3,3,3,3,3,3,3,3,3,3,3,3,3,3,3,3,3,3,3,3,3,3,3,3,3,3,
3,3,3,3,3,3,3,3,3,3,3,3,3,3,3,3,4),(120.503262642873,120.617419761429,120.731605283755,
120.845948024917,120.960381712593,121.075041343255,121.114428319549,121.227907702834,
121.341185397125,121.454351019198,121.567449377216,121.680525179237,121.793704930971,
121.906936195968,122.020381157543,122.107169535283,122.220649475003,122.333927737086,
122.447093933443,122.560192871148,122.673269257177,122.786449594829,122.899681447703,
123.013126992918,123.099910751017,123.213387493319,123.326662553936,123.439825548767,
123.552921290523,123.665994491818,123.77917168732,123.892400416852,124.005842908394,
124.092651966751,124.206133427493,124.319413171372,124.432580824504,124.545681191699,
124.658758977639,124.771940658917,124.88517382624,124.998620622273,125.085393182485,
125.198876862092,125.312158916064,125.425328933151,125.538431713338,125.651511956554,
125.764696142916,125.877931845702,125.991381194297,126.078134398219,126.19070721261,
126.303112647737,126.415397121371,126.527628178912,126.639829704837,126.752088559023,
126.786447950053),.UNSPECIFIED.);
#334=B_SPLINE_CURVE_WITH_KNOTS('',3,(#39035,#39036,#39037,#39038,#39039,
#39040,#39041,#39042,#39043),.UNSPECIFIED.,.F.,.F.,(4,1,1,1,1,1,4),(126.786452265782,
127.070875613953,128.063616829687,129.056358045421,130.049099261155,131.041840476889,
131.946420123781),.UNSPECIFIED.);
#335=B_SPLINE_CURVE_WITH_KNOTS('',3,(#39046,#39047,#39048,#39049,#39050,
#39051,#39052,#39053),.UNSPECIFIED.,.F.,.F.,(4,1,1,1,1,4),(-134.020064124091,
-133.027322908357,-132.034581692623,-131.041840476889,-130.049099261155,
-129.755734755382),.UNSPECIFIED.);
#336=B_SPLINE_CURVE_WITH_KNOTS('',3,(#39056,#39057,#39058,#39059,#39060,
#39061,#39062,#39063,#39064,#39065,#39066,#39067,#39068,#39069,#39070,#39071,
#39072,#39073,#39074,#39075,#39076,#39077,#39078,#39079,#39080,#39081,#39082,
#39083,#39084,#39085,#39086,#39087,#39088,#39089,#39090,#39091,#39092,#39093,
#39094,#39095,#39096,#39097,#39098,#39099,#39100,#39101,#39102,#39103,#39104,
#39105,#39106,#39107,#39108,#39109,#39110,#39111,#39112,#39113,#39114,#39115,
#39116,#39117,#39118,#39119,#39120,#39121,#39122,#39123,#39124,#39125,#39126,
#39127,#39128,#39129,#39130,#39131,#39132,#39133,#39134,#39135,#39136,#39137,
#39138,#39139,#39140,#39141,#39142,#39143,#39144,#39145,#39146,#39147,#39148,
#39149,#39150,#39151,#39152,#39153,#39154,#39155,#39156,#39157,#39158,#39159,
#39160,#39161,#39162,#39163,#39164,#39165,#39166,#39167,#39168,#39169,#39170,
#39171,#39172,#39173,#39174,#39175,#39176,#39177,#39178,#39179,#39180,#39181,
#39182,#39183,#39184,#39185,#39186,#39187,#39188,#39189,#39190,#39191),
 .UNSPECIFIED.,.F.,.F.,(4,2,2,2,2,2,2,2,2,2,2,2,2,2,2,2,2,2,2,2,2,2,2,2,
2,2,2,2,2,2,2,2,2,2,2,2,2,2,2,2,2,2,2,2,2,2,2,2,2,2,2,2,2,2,2,2,2,2,2,2,
2,2,2,2,2,2,2,4),(0.00176209102869683,0.0264792159075929,0.0438495035001408,
0.047196853344516,0.0491041638455065,0.0507593654656551,0.0527996174980107,
0.055933703762744,0.0773887891690063,0.0930730615746935,0.103703602775703,
0.105131654621243,0.106358820473087,0.107289652483095,0.108188731290211,
0.109716721408549,0.114294010565008,0.137364792206793,0.157768387434864,
0.162258303445078,0.164385196431052,0.166035036296661,0.16785737095035,
0.170863338665144,0.181256475004044,0.211502491183297,0.217990192922471,
0.222064946029316,0.223500893938311,0.224460509340364,0.225312359598861,
0.226476848011434,0.229387236392034,0.251300068517605,0.268671918259035,
0.274974946524858,0.279649189219162,0.281795639089747,0.283432322865378,
0.285211897940308,0.288082858824996,0.297378534974733,0.325457406778818,
0.334233111192271,0.33925061420772,0.340792180490021,0.341768645259298,
0.342704925578973,0.343859916723438,0.34670315133294,0.369996538171123,
0.393583849234611,0.397538297291555,0.39955751987109,0.401192543613393,
0.403072688240712,0.406275811733863,0.419846162533761,0.443546581920891,
0.455527205378817,0.457527376635214,0.458611298838436,0.459529650948841,
0.460708441669346,0.462624208690482,0.4766383722512,0.500757185256959,0.500786432389318),
 .UNSPECIFIED.);
#337=B_SPLINE_CURVE_WITH_KNOTS('',3,(#39195,#39196,#39197,#39198,#39199,
#39200,#39201,#39202,#39203,#39204,#39205,#39206,#39207,#39208,#39209,#39210,
#39211,#39212,#39213,#39214,#39215,#39216,#39217,#39218,#39219),
 .UNSPECIFIED.,.F.,.F.,(4,3,3,3,3,3,3,3,4),(141.371669412108,141.493689526562,
141.615502007272,141.737153936073,141.858692142336,141.980203542838,142.101690110534,
142.223281060979,142.322100278399),.UNSPECIFIED.);
#338=B_SPLINE_CURVE_WITH_KNOTS('',3,(#39220,#39221,#39222,#39223,#39224,
#39225,#39226,#39227,#39228,#39229,#39230,#39231,#39232,#39233,#39234,#39235,
#39236,#39237,#39238,#39239,#39240,#39241,#39242,#39243,#39244,#39245,#39246,
#39247,#39248,#39249,#39250,#39251,#39252,#39253,#39254,#39255,#39256,#39257,
#39258,#39259,#39260,#39261,#39262,#39263,#39264,#39265,#39266,#39267,#39268,
#39269,#39270,#39271,#39272,#39273,#39274,#39275,#39276,#39277,#39278,#39279,
#39280),.UNSPECIFIED.,.F.,.F.,(4,3,3,3,3,3,3,3,3,3,3,3,3,3,3,3,3,3,3,3,
4),(139.325788760491,139.343876631197,139.467969283164,139.587674259952,
139.707262751196,139.826787199013,139.946299934308,140.065935202646,140.185644425912,
140.30556889234,140.336617846931,140.460710498898,140.57912419592,140.697422046221,
140.815658774885,140.933888993062,141.052258648101,141.17071039991,141.289402107531,
141.329359062665,141.371669411541),.UNSPECIFIED.);
#339=B_SPLINE_CURVE_WITH_KNOTS('',3,(#39833,#39834,#39835,#39836,#39837,
#39838,#39839,#39840,#39841,#39842,#39843,#39844,#39845,#39846,#39847,#39848,
#39849,#39850,#39851,#39852,#39853,#39854,#39855,#39856,#39857,#39858,#39859,
#39860,#39861,#39862,#39863,#39864,#39865,#39866,#39867,#39868,#39869,#39870,
#39871,#39872,#39873,#39874,#39875,#39876,#39877,#39878,#39879,#39880,#39881,
#39882,#39883,#39884,#39885,#39886,#39887,#39888,#39889,#39890,#39891,#39892,
#39893,#39894,#39895,#39896,#39897,#39898,#39899,#39900,#39901,#39902,#39903,
#39904,#39905,#39906,#39907,#39908),.UNSPECIFIED.,.F.,.F.,(4,3,3,3,3,3,
3,3,3,3,3,3,3,3,3,3,3,3,3,3,3,3,3,3,3,4),(0.,0.0128630913698734,0.0303244724323763,
0.0454691953909234,0.0523699336523886,0.0555723769695474,0.058851428328098,
0.0758814661698019,0.0926327693964218,0.107460583641014,0.112206797292344,
0.128373668063903,0.144022366178101,0.151482256100753,0.160181126345686,
0.16370248329297,0.179587174239128,0.195601783608132,0.20580545806969,0.211151145077996,
0.214604522909917,0.230111340110616,0.242198051144648,0.246866712384057,
0.261749252048383,0.27663179171271),.UNSPECIFIED.);
#340=B_SPLINE_CURVE_WITH_KNOTS('',3,(#39910,#39911,#39912,#39913,#39914,
#39915,#39916,#39917,#39918,#39919,#39920,#39921,#39922,#39923,#39924,#39925,
#39926,#39927,#39928,#39929,#39930,#39931,#39932,#39933,#39934,#39935,#39936,
#39937,#39938,#39939,#39940,#39941,#39942,#39943,#39944,#39945,#39946,#39947,
#39948,#39949,#39950,#39951,#39952,#39953,#39954,#39955,#39956,#39957,#39958,
#39959,#39960,#39961,#39962,#39963,#39964,#39965,#39966,#39967,#39968,#39969,
#39970,#39971,#39972,#39973,#39974,#39975,#39976,#39977,#39978,#39979,#39980,
#39981,#39982,#39983,#39984,#39985,#39986,#39987,#39988),.UNSPECIFIED.,
 .F.,.F.,(4,3,3,3,3,3,3,3,3,3,3,3,3,3,3,3,3,3,3,3,3,3,3,3,3,3,4),(0.,0.0104682740580808,
0.0249726762435748,0.0388983633715248,0.0464392559381417,0.0494484513162411,
0.0648276131926065,0.0805461214315321,0.0952812770765815,0.0982282573713909,
0.114463949458838,0.130606063061321,0.136378173267175,0.141969567767405,
0.145793041159068,0.148766316560102,0.165124152230842,0.181481987901583,
0.193217024208496,0.197997620770074,0.201207739543446,0.218247298082551,
0.232526043151136,0.236419268721192,0.240186973323727,0.257774625840308,
0.275362278356888),.UNSPECIFIED.);
#341=B_SPLINE_CURVE_WITH_KNOTS('',3,(#39989,#39990,#39991,#39992),
 .UNSPECIFIED.,.F.,.F.,(4,4),(-0.0118538709981997,0.),.UNSPECIFIED.);
#342=B_SPLINE_CURVE_WITH_KNOTS('',3,(#40546,#40547,#40548,#40549,#40550,
#40551,#40552,#40553,#40554,#40555,#40556,#40557,#40558,#40559,#40560,#40561,
#40562,#40563,#40564,#40565,#40566,#40567,#40568,#40569,#40570,#40571,#40572,
#40573,#40574,#40575,#40576,#40577,#40578,#40579,#40580,#40581,#40582,#40583,
#40584,#40585,#40586,#40587,#40588,#40589,#40590,#40591,#40592,#40593,#40594,
#40595,#40596,#40597,#40598,#40599,#40600,#40601,#40602,#40603,#40604,#40605,
#40606,#40607,#40608,#40609,#40610,#40611,#40612,#40613,#40614,#40615,#40616,
#40617,#40618,#40619,#40620,#40621,#40622,#40623,#40624),.UNSPECIFIED.,
 .F.,.F.,(4,3,3,3,3,3,3,3,3,3,3,3,3,3,3,3,3,3,3,3,3,3,3,3,3,3,4),(0.,0.0104682740580829,
0.024972670333206,0.0388983581999524,0.0464392448908457,0.0494484486674944,
0.0648276069840781,0.0806079623489334,0.0952812647645025,0.0982282543159663,
0.114463946169951,0.130606059492799,0.136378173267178,0.141969568696793,
0.145793045570947,0.148766323848641,0.164775566334638,0.181332445677576,
0.193217026624088,0.197997633296994,0.201207746865786,0.218247303068156,
0.23252604689034,0.236419276828848,0.240186974613934,0.257774626485413,
0.275362278356893),.UNSPECIFIED.);
#343=B_SPLINE_CURVE_WITH_KNOTS('',3,(#40625,#40626,#40627,#40628),
 .UNSPECIFIED.,.F.,.F.,(4,4),(0.,0.012085325422919),.UNSPECIFIED.);
#344=B_SPLINE_CURVE_WITH_KNOTS('',3,(#40629,#40630,#40631,#40632,#40633,
#40634,#40635,#40636,#40637,#40638,#40639,#40640,#40641,#40642,#40643,#40644,
#40645,#40646,#40647,#40648,#40649,#40650,#40651,#40652,#40653,#40654,#40655,
#40656,#40657,#40658,#40659,#40660,#40661,#40662,#40663,#40664,#40665,#40666,
#40667,#40668,#40669,#40670,#40671,#40672,#40673,#40674,#40675,#40676,#40677,
#40678,#40679,#40680,#40681,#40682,#40683,#40684,#40685,#40686,#40687,#40688,
#40689,#40690,#40691,#40692,#40693,#40694,#40695,#40696,#40697,#40698,#40699,
#40700,#40701,#40702,#40703,#40704),.UNSPECIFIED.,.F.,.F.,(4,3,3,3,3,3,
3,3,3,3,3,3,3,3,3,3,3,3,3,3,3,3,3,3,3,4),(0.,0.0128630913698816,0.0303093412047053,
0.0454691954866925,0.0523699326729681,0.055572374082829,0.0588514270956641,
0.0758800910821112,0.0927866891993117,0.107460580924677,0.111898501539777,
0.128069590135318,0.144022356052112,0.151482256100771,0.160181127295678,
0.163702483665548,0.179663555189427,0.195687409679772,0.205805457433891,
0.211151145252578,0.214604523387748,0.230111340468992,0.242198051854846,
0.246866712599024,0.261749252155874,0.276631791712723),.UNSPECIFIED.);
#345=SHAPE_REPRESENTATION_RELATIONSHIP('SRR','None',#40766,#353);
#346=SHAPE_REPRESENTATION_RELATIONSHIP('SRR','None',#40767,#354);
#347=SHAPE_REPRESENTATION_RELATIONSHIP('SRR','None',#40768,#355);
#348=SHAPE_REPRESENTATION_RELATIONSHIP('SRR','None',#40769,#356);
#349=SHAPE_REPRESENTATION_RELATIONSHIP('SRR','None',#40770,#357);
#350=SHAPE_REPRESENTATION_RELATIONSHIP('SRR','None',#40771,#358);
#351=SHAPE_REPRESENTATION_RELATIONSHIP('SRR','None',#40772,#359);
#352=SHAPE_REPRESENTATION_RELATIONSHIP('SRR','None',#40773,#360);
#353=ADVANCED_BREP_SHAPE_REPRESENTATION('',(#370),#40726);
#354=ADVANCED_BREP_SHAPE_REPRESENTATION('',(#371),#40727);
#355=ADVANCED_BREP_SHAPE_REPRESENTATION('',(#372),#40728);
#356=ADVANCED_BREP_SHAPE_REPRESENTATION('',(#373),#40729);
#357=ADVANCED_BREP_SHAPE_REPRESENTATION('',(#374,#375),#40730);
#358=ADVANCED_BREP_SHAPE_REPRESENTATION('',(#376),#40731);
#359=ADVANCED_BREP_SHAPE_REPRESENTATION('',(#377),#40732);
#360=ADVANCED_BREP_SHAPE_REPRESENTATION('',(#378),#40733);
#361=STYLED_ITEM('',(#40815),#370);
#362=STYLED_ITEM('',(#40816),#371);
#363=STYLED_ITEM('',(#40815),#372);
#364=STYLED_ITEM('',(#40815),#373);
#365=STYLED_ITEM('',(#40816),#374);
#366=STYLED_ITEM('',(#40816),#375);
#367=STYLED_ITEM('',(#40815),#376);
#368=STYLED_ITEM('',(#40815),#377);
#369=STYLED_ITEM('',(#40815),#378);
#370=MANIFOLD_SOLID_BREP('Body1',#3166);
#371=MANIFOLD_SOLID_BREP('Body1',#3167);
#372=MANIFOLD_SOLID_BREP('Body1',#3168);
#373=MANIFOLD_SOLID_BREP('Body1',#3169);
#374=MANIFOLD_SOLID_BREP('Body1',#3170);
#375=MANIFOLD_SOLID_BREP('Body2',#3171);
#376=MANIFOLD_SOLID_BREP('Body1',#3172);
#377=MANIFOLD_SOLID_BREP('Body1',#3173);
#378=MANIFOLD_SOLID_BREP('Body1',#3174);
#379=SPHERICAL_SURFACE('',#3282,3.53951905042299);
#380=SPHERICAL_SURFACE('',#3338,3.53951905042299);
#381=FACE_BOUND('',#591,.T.);
#382=FACE_BOUND('',#596,.T.);
#383=FACE_BOUND('',#599,.T.);
#384=FACE_BOUND('',#604,.T.);
#385=FACE_BOUND('',#616,.T.);
#386=FACE_BOUND('',#624,.T.);
#387=FACE_BOUND('',#629,.T.);
#388=FACE_BOUND('',#634,.T.);
#389=FACE_BOUND('',#700,.T.);
#390=FACE_BOUND('',#708,.T.);
#391=TOROIDAL_SURFACE('',#3270,1.16126351211314,1.);
#392=TOROIDAL_SURFACE('',#3290,2.90634189295526,1.);
#393=TOROIDAL_SURFACE('',#3295,2.90634189295527,0.999999999999996);
#394=TOROIDAL_SURFACE('',#3325,1.16126351211314,1.);
#395=PLANE('',#3269);
#396=PLANE('',#3274);
#397=PLANE('',#3281);
#398=PLANE('',#3288);
#399=PLANE('',#3298);
#400=PLANE('',#3312);
#401=PLANE('',#3313);
#402=PLANE('',#3314);
#403=PLANE('',#3315);
#404=PLANE('',#3316);
#405=PLANE('',#3317);
#406=PLANE('',#3318);
#407=PLANE('',#3319);
#408=PLANE('',#3324);
#409=PLANE('',#3330);
#410=PLANE('',#3337);
#411=PLANE('',#3341);
#412=PLANE('',#3345);
#413=PLANE('',#3346);
#414=PLANE('',#3350);
#415=PLANE('',#3400);
#416=PLANE('',#3401);
#417=PLANE('',#3415);
#418=PLANE('',#3416);
#419=PLANE('',#3417);
#420=PLANE('',#3418);
#421=PLANE('',#3419);
#422=PLANE('',#3420);
#423=PLANE('',#3421);
#424=PLANE('',#3422);
#425=PLANE('',#3472);
#426=PLANE('',#3473);
#427=FACE_OUTER_BOUND('',#587,.T.);
#428=FACE_OUTER_BOUND('',#588,.T.);
#429=FACE_OUTER_BOUND('',#589,.T.);
#430=FACE_OUTER_BOUND('',#590,.T.);
#431=FACE_OUTER_BOUND('',#592,.T.);
#432=FACE_OUTER_BOUND('',#593,.T.);
#433=FACE_OUTER_BOUND('',#594,.T.);
#434=FACE_OUTER_BOUND('',#595,.T.);
#435=FACE_OUTER_BOUND('',#597,.T.);
#436=FACE_OUTER_BOUND('',#598,.T.);
#437=FACE_OUTER_BOUND('',#600,.T.);
#438=FACE_OUTER_BOUND('',#601,.T.);
#439=FACE_OUTER_BOUND('',#602,.T.);
#440=FACE_OUTER_BOUND('',#603,.T.);
#441=FACE_OUTER_BOUND('',#605,.T.);
#442=FACE_OUTER_BOUND('',#606,.T.);
#443=FACE_OUTER_BOUND('',#607,.T.);
#444=FACE_OUTER_BOUND('',#608,.T.);
#445=FACE_OUTER_BOUND('',#609,.T.);
#446=FACE_OUTER_BOUND('',#610,.T.);
#447=FACE_OUTER_BOUND('',#611,.T.);
#448=FACE_OUTER_BOUND('',#612,.T.);
#449=FACE_OUTER_BOUND('',#613,.T.);
#450=FACE_OUTER_BOUND('',#614,.T.);
#451=FACE_OUTER_BOUND('',#615,.T.);
#452=FACE_OUTER_BOUND('',#617,.T.);
#453=FACE_OUTER_BOUND('',#618,.T.);
#454=FACE_OUTER_BOUND('',#619,.T.);
#455=FACE_OUTER_BOUND('',#620,.T.);
#456=FACE_OUTER_BOUND('',#621,.T.);
#457=FACE_OUTER_BOUND('',#622,.T.);
#458=FACE_OUTER_BOUND('',#623,.T.);
#459=FACE_OUTER_BOUND('',#625,.T.);
#460=FACE_OUTER_BOUND('',#626,.T.);
#461=FACE_OUTER_BOUND('',#627,.T.);
#462=FACE_OUTER_BOUND('',#628,.T.);
#463=FACE_OUTER_BOUND('',#630,.T.);
#464=FACE_OUTER_BOUND('',#631,.T.);
#465=FACE_OUTER_BOUND('',#632,.T.);
#466=FACE_OUTER_BOUND('',#633,.T.);
#467=FACE_OUTER_BOUND('',#635,.T.);
#468=FACE_OUTER_BOUND('',#636,.T.);
#469=FACE_OUTER_BOUND('',#637,.T.);
#470=FACE_OUTER_BOUND('',#638,.T.);
#471=FACE_OUTER_BOUND('',#639,.T.);
#472=FACE_OUTER_BOUND('',#640,.T.);
#473=FACE_OUTER_BOUND('',#641,.T.);
#474=FACE_OUTER_BOUND('',#642,.T.);
#475=FACE_OUTER_BOUND('',#643,.T.);
#476=FACE_OUTER_BOUND('',#644,.T.);
#477=FACE_OUTER_BOUND('',#645,.T.);
#478=FACE_OUTER_BOUND('',#646,.T.);
#479=FACE_OUTER_BOUND('',#647,.T.);
#480=FACE_OUTER_BOUND('',#648,.T.);
#481=FACE_OUTER_BOUND('',#649,.T.);
#482=FACE_OUTER_BOUND('',#650,.T.);
#483=FACE_OUTER_BOUND('',#651,.T.);
#484=FACE_OUTER_BOUND('',#652,.T.);
#485=FACE_OUTER_BOUND('',#653,.T.);
#486=FACE_OUTER_BOUND('',#654,.T.);
#487=FACE_OUTER_BOUND('',#655,.T.);
#488=FACE_OUTER_BOUND('',#656,.T.);
#489=FACE_OUTER_BOUND('',#657,.T.);
#490=FACE_OUTER_BOUND('',#658,.T.);
#491=FACE_OUTER_BOUND('',#659,.T.);
#492=FACE_OUTER_BOUND('',#660,.T.);
#493=FACE_OUTER_BOUND('',#661,.T.);
#494=FACE_OUTER_BOUND('',#662,.T.);
#495=FACE_OUTER_BOUND('',#663,.T.);
#496=FACE_OUTER_BOUND('',#664,.T.);
#497=FACE_OUTER_BOUND('',#665,.T.);
#498=FACE_OUTER_BOUND('',#666,.T.);
#499=FACE_OUTER_BOUND('',#667,.T.);
#500=FACE_OUTER_BOUND('',#668,.T.);
#501=FACE_OUTER_BOUND('',#669,.T.);
#502=FACE_OUTER_BOUND('',#670,.T.);
#503=FACE_OUTER_BOUND('',#671,.T.);
#504=FACE_OUTER_BOUND('',#672,.T.);
#505=FACE_OUTER_BOUND('',#673,.T.);
#506=FACE_OUTER_BOUND('',#674,.T.);
#507=FACE_OUTER_BOUND('',#675,.T.);
#508=FACE_OUTER_BOUND('',#676,.T.);
#509=FACE_OUTER_BOUND('',#677,.T.);
#510=FACE_OUTER_BOUND('',#678,.T.);
#511=FACE_OUTER_BOUND('',#679,.T.);
#512=FACE_OUTER_BOUND('',#680,.T.);
#513=FACE_OUTER_BOUND('',#681,.T.);
#514=FACE_OUTER_BOUND('',#682,.T.);
#515=FACE_OUTER_BOUND('',#683,.T.);
#516=FACE_OUTER_BOUND('',#684,.T.);
#517=FACE_OUTER_BOUND('',#685,.T.);
#518=FACE_OUTER_BOUND('',#686,.T.);
#519=FACE_OUTER_BOUND('',#687,.T.);
#520=FACE_OUTER_BOUND('',#688,.T.);
#521=FACE_OUTER_BOUND('',#689,.T.);
#522=FACE_OUTER_BOUND('',#690,.T.);
#523=FACE_OUTER_BOUND('',#691,.T.);
#524=FACE_OUTER_BOUND('',#692,.T.);
#525=FACE_OUTER_BOUND('',#693,.T.);
#526=FACE_OUTER_BOUND('',#694,.T.);
#527=FACE_OUTER_BOUND('',#695,.T.);
#528=FACE_OUTER_BOUND('',#696,.T.);
#529=FACE_OUTER_BOUND('',#697,.T.);
#530=FACE_OUTER_BOUND('',#698,.T.);
#531=FACE_OUTER_BOUND('',#699,.T.);
#532=FACE_OUTER_BOUND('',#701,.T.);
#533=FACE_OUTER_BOUND('',#702,.T.);
#534=FACE_OUTER_BOUND('',#703,.T.);
#535=FACE_OUTER_BOUND('',#704,.T.);
#536=FACE_OUTER_BOUND('',#705,.T.);
#537=FACE_OUTER_BOUND('',#706,.T.);
#538=FACE_OUTER_BOUND('',#707,.T.);
#539=FACE_OUTER_BOUND('',#709,.T.);
#540=FACE_OUTER_BOUND('',#710,.T.);
#541=FACE_OUTER_BOUND('',#711,.T.);
#542=FACE_OUTER_BOUND('',#712,.T.);
#543=FACE_OUTER_BOUND('',#713,.T.);
#544=FACE_OUTER_BOUND('',#714,.T.);
#545=FACE_OUTER_BOUND('',#715,.T.);
#546=FACE_OUTER_BOUND('',#716,.T.);
#547=FACE_OUTER_BOUND('',#717,.T.);
#548=FACE_OUTER_BOUND('',#718,.T.);
#549=FACE_OUTER_BOUND('',#719,.T.);
#550=FACE_OUTER_BOUND('',#720,.T.);
#551=FACE_OUTER_BOUND('',#721,.T.);
#552=FACE_OUTER_BOUND('',#722,.T.);
#553=FACE_OUTER_BOUND('',#723,.T.);
#554=FACE_OUTER_BOUND('',#724,.T.);
#555=FACE_OUTER_BOUND('',#725,.T.);
#556=FACE_OUTER_BOUND('',#726,.T.);
#557=FACE_OUTER_BOUND('',#727,.T.);
#558=FACE_OUTER_BOUND('',#728,.T.);
#559=FACE_OUTER_BOUND('',#729,.T.);
#560=FACE_OUTER_BOUND('',#730,.T.);
#561=FACE_OUTER_BOUND('',#731,.T.);
#562=FACE_OUTER_BOUND('',#732,.T.);
#563=FACE_OUTER_BOUND('',#733,.T.);
#564=FACE_OUTER_BOUND('',#734,.T.);
#565=FACE_OUTER_BOUND('',#735,.T.);
#566=FACE_OUTER_BOUND('',#736,.T.);
#567=FACE_OUTER_BOUND('',#737,.T.);
#568=FACE_OUTER_BOUND('',#738,.T.);
#569=FACE_OUTER_BOUND('',#739,.T.);
#570=FACE_OUTER_BOUND('',#740,.T.);
#571=FACE_OUTER_BOUND('',#741,.T.);
#572=FACE_OUTER_BOUND('',#742,.T.);
#573=FACE_OUTER_BOUND('',#743,.T.);
#574=FACE_OUTER_BOUND('',#744,.T.);
#575=FACE_OUTER_BOUND('',#745,.T.);
#576=FACE_OUTER_BOUND('',#746,.T.);
#577=FACE_OUTER_BOUND('',#747,.T.);
#578=FACE_OUTER_BOUND('',#748,.T.);
#579=FACE_OUTER_BOUND('',#749,.T.);
#580=FACE_OUTER_BOUND('',#750,.T.);
#581=FACE_OUTER_BOUND('',#751,.T.);
#582=FACE_OUTER_BOUND('',#752,.T.);
#583=FACE_OUTER_BOUND('',#753,.T.);
#584=FACE_OUTER_BOUND('',#754,.T.);
#585=FACE_OUTER_BOUND('',#755,.T.);
#586=FACE_OUTER_BOUND('',#756,.T.);
#587=EDGE_LOOP('',(#1922,#1923,#1924,#1925));
#588=EDGE_LOOP('',(#1926));
#589=EDGE_LOOP('',(#1927,#1928,#1929,#1930));
#590=EDGE_LOOP('',(#1931));
#591=EDGE_LOOP('',(#1932));
#592=EDGE_LOOP('',(#1933,#1934,#1935,#1936,#1937));
#593=EDGE_LOOP('',(#1938,#1939,#1940,#1941));
#594=EDGE_LOOP('',(#1942));
#595=EDGE_LOOP('',(#1943,#1944,#1945,#1946));
#596=EDGE_LOOP('',(#1947));
#597=EDGE_LOOP('',(#1948,#1949,#1950,#1951));
#598=EDGE_LOOP('',(#1952));
#599=EDGE_LOOP('',(#1953));
#600=EDGE_LOOP('',(#1954,#1955,#1956,#1957));
#601=EDGE_LOOP('',(#1958,#1959,#1960,#1961));
#602=EDGE_LOOP('',(#1962,#1963,#1964,#1965));
#603=EDGE_LOOP('',(#1966));
#604=EDGE_LOOP('',(#1967));
#605=EDGE_LOOP('',(#1968,#1969,#1970,#1971));
#606=EDGE_LOOP('',(#1972,#1973,#1974,#1975,#1976,#1977));
#607=EDGE_LOOP('',(#1978,#1979,#1980,#1981,#1982,#1983));
#608=EDGE_LOOP('',(#1984,#1985,#1986,#1987,#1988));
#609=EDGE_LOOP('',(#1989,#1990,#1991,#1992,#1993,#1994));
#610=EDGE_LOOP('',(#1995,#1996,#1997,#1998));
#611=EDGE_LOOP('',(#1999,#2000,#2001,#2002,#2003,#2004));
#612=EDGE_LOOP('',(#2005,#2006,#2007,#2008,#2009,#2010));
#613=EDGE_LOOP('',(#2011,#2012,#2013,#2014,#2015,#2016,#2017,#2018,#2019,
#2020,#2021,#2022,#2023,#2024,#2025,#2026));
#614=EDGE_LOOP('',(#2027,#2028,#2029,#2030,#2031,#2032,#2033,#2034,#2035,
#2036,#2037,#2038,#2039,#2040,#2041,#2042));
#615=EDGE_LOOP('',(#2043,#2044,#2045,#2046,#2047,#2048));
#616=EDGE_LOOP('',(#2049,#2050,#2051,#2052));
#617=EDGE_LOOP('',(#2053,#2054,#2055,#2056));
#618=EDGE_LOOP('',(#2057,#2058,#2059,#2060));
#619=EDGE_LOOP('',(#2061,#2062,#2063,#2064));
#620=EDGE_LOOP('',(#2065,#2066,#2067,#2068));
#621=EDGE_LOOP('',(#2069,#2070,#2071,#2072));
#622=EDGE_LOOP('',(#2073,#2074,#2075,#2076));
#623=EDGE_LOOP('',(#2077,#2078,#2079,#2080,#2081,#2082));
#624=EDGE_LOOP('',(#2083,#2084,#2085,#2086,#2087));
#625=EDGE_LOOP('',(#2088,#2089,#2090,#2091));
#626=EDGE_LOOP('',(#2092));
#627=EDGE_LOOP('',(#2093,#2094,#2095,#2096,#2097));
#628=EDGE_LOOP('',(#2098));
#629=EDGE_LOOP('',(#2099));
#630=EDGE_LOOP('',(#2100,#2101,#2102,#2103,#2104,#2105));
#631=EDGE_LOOP('',(#2106,#2107,#2108,#2109));
#632=EDGE_LOOP('',(#2110));
#633=EDGE_LOOP('',(#2111,#2112,#2113,#2114));
#634=EDGE_LOOP('',(#2115));
#635=EDGE_LOOP('',(#2116));
#636=EDGE_LOOP('',(#2117,#2118,#2119,#2120));
#637=EDGE_LOOP('',(#2121));
#638=EDGE_LOOP('',(#2122));
#639=EDGE_LOOP('',(#2123,#2124,#2125,#2126));
#640=EDGE_LOOP('',(#2127));
#641=EDGE_LOOP('',(#2128,#2129,#2130,#2131));
#642=EDGE_LOOP('',(#2132,#2133,#2134,#2135,#2136));
#643=EDGE_LOOP('',(#2137,#2138,#2139,#2140,#2141));
#644=EDGE_LOOP('',(#2142,#2143,#2144,#2145,#2146));
#645=EDGE_LOOP('',(#2147,#2148,#2149,#2150,#2151));
#646=EDGE_LOOP('',(#2152,#2153,#2154,#2155,#2156));
#647=EDGE_LOOP('',(#2157,#2158,#2159,#2160,#2161));
#648=EDGE_LOOP('',(#2162,#2163,#2164,#2165,#2166));
#649=EDGE_LOOP('',(#2167,#2168,#2169,#2170,#2171));
#650=EDGE_LOOP('',(#2172,#2173,#2174,#2175,#2176));
#651=EDGE_LOOP('',(#2177,#2178,#2179,#2180,#2181));
#652=EDGE_LOOP('',(#2182,#2183,#2184,#2185,#2186));
#653=EDGE_LOOP('',(#2187,#2188,#2189,#2190,#2191));
#654=EDGE_LOOP('',(#2192,#2193,#2194,#2195,#2196));
#655=EDGE_LOOP('',(#2197,#2198,#2199,#2200,#2201));
#656=EDGE_LOOP('',(#2202,#2203,#2204,#2205,#2206));
#657=EDGE_LOOP('',(#2207,#2208,#2209,#2210,#2211));
#658=EDGE_LOOP('',(#2212,#2213,#2214,#2215,#2216));
#659=EDGE_LOOP('',(#2217,#2218,#2219,#2220,#2221));
#660=EDGE_LOOP('',(#2222,#2223,#2224,#2225,#2226));
#661=EDGE_LOOP('',(#2227,#2228,#2229,#2230,#2231,#2232));
#662=EDGE_LOOP('',(#2233,#2234,#2235,#2236));
#663=EDGE_LOOP('',(#2237,#2238,#2239,#2240));
#664=EDGE_LOOP('',(#2241,#2242,#2243,#2244));
#665=EDGE_LOOP('',(#2245,#2246,#2247,#2248));
#666=EDGE_LOOP('',(#2249,#2250,#2251,#2252));
#667=EDGE_LOOP('',(#2253,#2254,#2255,#2256));
#668=EDGE_LOOP('',(#2257,#2258,#2259,#2260));
#669=EDGE_LOOP('',(#2261,#2262,#2263,#2264));
#670=EDGE_LOOP('',(#2265,#2266,#2267,#2268));
#671=EDGE_LOOP('',(#2269,#2270,#2271,#2272));
#672=EDGE_LOOP('',(#2273,#2274,#2275,#2276));
#673=EDGE_LOOP('',(#2277,#2278,#2279,#2280));
#674=EDGE_LOOP('',(#2281,#2282,#2283,#2284));
#675=EDGE_LOOP('',(#2285,#2286,#2287,#2288));
#676=EDGE_LOOP('',(#2289,#2290,#2291,#2292));
#677=EDGE_LOOP('',(#2293,#2294,#2295,#2296));
#678=EDGE_LOOP('',(#2297,#2298,#2299,#2300));
#679=EDGE_LOOP('',(#2301,#2302,#2303,#2304));
#680=EDGE_LOOP('',(#2305,#2306,#2307,#2308));
#681=EDGE_LOOP('',(#2309,#2310,#2311,#2312));
#682=EDGE_LOOP('',(#2313,#2314,#2315,#2316));
#683=EDGE_LOOP('',(#2317,#2318,#2319,#2320));
#684=EDGE_LOOP('',(#2321,#2322,#2323,#2324,#2325));
#685=EDGE_LOOP('',(#2326,#2327,#2328,#2329,#2330,#2331,#2332,#2333,#2334,
#2335,#2336,#2337,#2338,#2339,#2340,#2341,#2342,#2343,#2344,#2345,#2346,
#2347,#2348,#2349,#2350,#2351,#2352,#2353,#2354,#2355,#2356,#2357,#2358,
#2359,#2360,#2361,#2362,#2363,#2364,#2365,#2366,#2367,#2368,#2369,#2370,
#2371,#2372,#2373,#2374,#2375,#2376,#2377,#2378,#2379,#2380,#2381,#2382,
#2383));
#686=EDGE_LOOP('',(#2384,#2385,#2386,#2387,#2388,#2389,#2390,#2391,#2392,
#2393,#2394,#2395,#2396,#2397,#2398,#2399,#2400,#2401,#2402,#2403,#2404,
#2405,#2406,#2407,#2408,#2409,#2410,#2411,#2412,#2413,#2414,#2415,#2416,
#2417,#2418,#2419,#2420,#2421,#2422,#2423,#2424,#2425,#2426,#2427,#2428,
#2429,#2430,#2431,#2432,#2433,#2434,#2435,#2436,#2437,#2438,#2439,#2440,
#2441));
#687=EDGE_LOOP('',(#2442,#2443,#2444,#2445,#2446));
#688=EDGE_LOOP('',(#2447,#2448,#2449,#2450,#2451));
#689=EDGE_LOOP('',(#2452,#2453,#2454,#2455));
#690=EDGE_LOOP('',(#2456,#2457,#2458,#2459,#2460,#2461));
#691=EDGE_LOOP('',(#2462,#2463,#2464,#2465,#2466,#2467));
#692=EDGE_LOOP('',(#2468,#2469,#2470,#2471,#2472));
#693=EDGE_LOOP('',(#2473,#2474,#2475,#2476,#2477));
#694=EDGE_LOOP('',(#2478,#2479,#2480,#2481));
#695=EDGE_LOOP('',(#2482,#2483,#2484,#2485,#2486));
#696=EDGE_LOOP('',(#2487,#2488,#2489,#2490,#2491,#2492));
#697=EDGE_LOOP('',(#2493,#2494,#2495,#2496,#2497,#2498,#2499,#2500,#2501,
#2502,#2503,#2504,#2505,#2506));
#698=EDGE_LOOP('',(#2507,#2508,#2509,#2510,#2511,#2512,#2513,#2514,#2515,
#2516,#2517,#2518,#2519,#2520,#2521,#2522));
#699=EDGE_LOOP('',(#2523,#2524,#2525,#2526,#2527,#2528));
#700=EDGE_LOOP('',(#2529,#2530,#2531,#2532));
#701=EDGE_LOOP('',(#2533,#2534,#2535,#2536));
#702=EDGE_LOOP('',(#2537,#2538,#2539,#2540));
#703=EDGE_LOOP('',(#2541,#2542,#2543,#2544));
#704=EDGE_LOOP('',(#2545,#2546,#2547,#2548));
#705=EDGE_LOOP('',(#2549,#2550,#2551,#2552));
#706=EDGE_LOOP('',(#2553,#2554,#2555,#2556));
#707=EDGE_LOOP('',(#2557,#2558,#2559,#2560,#2561,#2562));
#708=EDGE_LOOP('',(#2563,#2564,#2565,#2566,#2567));
#709=EDGE_LOOP('',(#2568,#2569,#2570,#2571));
#710=EDGE_LOOP('',(#2572,#2573,#2574,#2575,#2576));
#711=EDGE_LOOP('',(#2577,#2578,#2579,#2580,#2581));
#712=EDGE_LOOP('',(#2582,#2583,#2584,#2585,#2586));
#713=EDGE_LOOP('',(#2587,#2588,#2589,#2590,#2591));
#714=EDGE_LOOP('',(#2592,#2593,#2594,#2595,#2596));
#715=EDGE_LOOP('',(#2597,#2598,#2599,#2600,#2601));
#716=EDGE_LOOP('',(#2602,#2603,#2604,#2605,#2606));
#717=EDGE_LOOP('',(#2607,#2608,#2609,#2610,#2611));
#718=EDGE_LOOP('',(#2612,#2613,#2614,#2615,#2616));
#719=EDGE_LOOP('',(#2617,#2618,#2619,#2620,#2621));
#720=EDGE_LOOP('',(#2622,#2623,#2624,#2625,#2626));
#721=EDGE_LOOP('',(#2627,#2628,#2629,#2630,#2631));
#722=EDGE_LOOP('',(#2632,#2633,#2634,#2635,#2636));
#723=EDGE_LOOP('',(#2637,#2638,#2639,#2640,#2641));
#724=EDGE_LOOP('',(#2642,#2643,#2644,#2645,#2646));
#725=EDGE_LOOP('',(#2647,#2648,#2649,#2650,#2651));
#726=EDGE_LOOP('',(#2652,#2653,#2654,#2655,#2656));
#727=EDGE_LOOP('',(#2657,#2658,#2659,#2660,#2661));
#728=EDGE_LOOP('',(#2662,#2663,#2664,#2665,#2666));
#729=EDGE_LOOP('',(#2667,#2668,#2669,#2670,#2671,#2672));
#730=EDGE_LOOP('',(#2673,#2674,#2675,#2676));
#731=EDGE_LOOP('',(#2677,#2678,#2679,#2680));
#732=EDGE_LOOP('',(#2681,#2682,#2683,#2684));
#733=EDGE_LOOP('',(#2685,#2686,#2687,#2688));
#734=EDGE_LOOP('',(#2689,#2690,#2691,#2692));
#735=EDGE_LOOP('',(#2693,#2694,#2695,#2696));
#736=EDGE_LOOP('',(#2697,#2698,#2699,#2700));
#737=EDGE_LOOP('',(#2701,#2702,#2703,#2704));
#738=EDGE_LOOP('',(#2705,#2706,#2707,#2708));
#739=EDGE_LOOP('',(#2709,#2710,#2711,#2712));
#740=EDGE_LOOP('',(#2713,#2714,#2715,#2716));
#741=EDGE_LOOP('',(#2717,#2718,#2719,#2720));
#742=EDGE_LOOP('',(#2721,#2722,#2723,#2724));
#743=EDGE_LOOP('',(#2725,#2726,#2727,#2728));
#744=EDGE_LOOP('',(#2729,#2730,#2731,#2732));
#745=EDGE_LOOP('',(#2733,#2734,#2735,#2736));
#746=EDGE_LOOP('',(#2737,#2738,#2739,#2740));
#747=EDGE_LOOP('',(#2741,#2742,#2743,#2744));
#748=EDGE_LOOP('',(#2745,#2746,#2747,#2748));
#749=EDGE_LOOP('',(#2749,#2750,#2751,#2752));
#750=EDGE_LOOP('',(#2753,#2754,#2755,#2756));
#751=EDGE_LOOP('',(#2757,#2758,#2759,#2760));
#752=EDGE_LOOP('',(#2761,#2762,#2763,#2764,#2765));
#753=EDGE_LOOP('',(#2766,#2767,#2768,#2769,#2770,#2771,#2772,#2773,#2774,
#2775,#2776,#2777,#2778,#2779,#2780,#2781,#2782,#2783,#2784,#2785,#2786,
#2787,#2788,#2789,#2790,#2791,#2792,#2793,#2794,#2795,#2796,#2797,#2798,
#2799,#2800,#2801,#2802,#2803,#2804,#2805,#2806,#2807,#2808,#2809,#2810,
#2811,#2812,#2813,#2814,#2815,#2816,#2817,#2818,#2819,#2820,#2821,#2822,
#2823));
#754=EDGE_LOOP('',(#2824,#2825,#2826,#2827,#2828,#2829,#2830,#2831,#2832,
#2833,#2834,#2835,#2836,#2837,#2838,#2839,#2840,#2841,#2842,#2843,#2844,
#2845,#2846,#2847,#2848,#2849,#2850,#2851,#2852,#2853,#2854,#2855,#2856,
#2857,#2858,#2859,#2860,#2861,#2862,#2863,#2864,#2865,#2866,#2867,#2868,
#2869,#2870,#2871,#2872,#2873,#2874,#2875,#2876,#2877,#2878,#2879,#2880,
#2881));
#755=EDGE_LOOP('',(#2882,#2883,#2884,#2885,#2886));
#756=EDGE_LOOP('',(#2887,#2888,#2889,#2890,#2891));
#757=LINE('',#4066,#899);
#758=LINE('',#4078,#900);
#759=LINE('',#4086,#901);
#760=LINE('',#4097,#902);
#761=LINE('',#4109,#903);
#762=LINE('',#4119,#904);
#763=LINE('',#4208,#905);
#764=LINE('',#4511,#906);
#765=LINE('',#4645,#907);
#766=LINE('',#4801,#908);
#767=LINE('',#5118,#909);
#768=LINE('',#6399,#910);
#769=LINE('',#6401,#911);
#770=LINE('',#6403,#912);
#771=LINE('',#6405,#913);
#772=LINE('',#6407,#914);
#773=LINE('',#6408,#915);
#774=LINE('',#6411,#916);
#775=LINE('',#6413,#917);
#776=LINE('',#6414,#918);
#777=LINE('',#6417,#919);
#778=LINE('',#6418,#920);
#779=LINE('',#6421,#921);
#780=LINE('',#6422,#922);
#781=LINE('',#6425,#923);
#782=LINE('',#6426,#924);
#783=LINE('',#6429,#925);
#784=LINE('',#6430,#926);
#785=LINE('',#6432,#927);
#786=LINE('',#6439,#928);
#787=LINE('',#6453,#929);
#788=LINE('',#6461,#930);
#789=LINE('',#6473,#931);
#790=LINE('',#6481,#932);
#791=LINE('',#6488,#933);
#792=LINE('',#6654,#934);
#793=LINE('',#7082,#935);
#794=LINE('',#7529,#936);
#795=LINE('',#7976,#937);
#796=LINE('',#8421,#938);
#797=LINE('',#8870,#939);
#798=LINE('',#9311,#940);
#799=LINE('',#9758,#941);
#800=LINE('',#10209,#942);
#801=LINE('',#10646,#943);
#802=LINE('',#11121,#944);
#803=LINE('',#11574,#945);
#804=LINE('',#12023,#946);
#805=LINE('',#12470,#947);
#806=LINE('',#12923,#948);
#807=LINE('',#13400,#949);
#808=LINE('',#13855,#950);
#809=LINE('',#14326,#951);
#810=LINE('',#14763,#952);
#811=LINE('',#15181,#953);
#812=LINE('',#15634,#954);
#813=LINE('',#15652,#955);
#814=LINE('',#15838,#956);
#815=LINE('',#16024,#957);
#816=LINE('',#16372,#958);
#817=LINE('',#16396,#959);
#818=LINE('',#16420,#960);
#819=LINE('',#16607,#961);
#820=LINE('',#16955,#962);
#821=LINE('',#16979,#963);
#822=LINE('',#17005,#964);
#823=LINE('',#17191,#965);
#824=LINE('',#17539,#966);
#825=LINE('',#17565,#967);
#826=LINE('',#17589,#968);
#827=LINE('',#17775,#969);
#828=LINE('',#18123,#970);
#829=LINE('',#18147,#971);
#830=LINE('',#18171,#972);
#831=LINE('',#18358,#973);
#832=LINE('',#18706,#974);
#833=LINE('',#20489,#975);
#834=LINE('',#20578,#976);
#835=LINE('',#20881,#977);
#836=LINE('',#21101,#978);
#837=LINE('',#21255,#979);
#838=LINE('',#21550,#980);
#839=LINE('',#22856,#981);
#840=LINE('',#22858,#982);
#841=LINE('',#22860,#983);
#842=LINE('',#22862,#984);
#843=LINE('',#22864,#985);
#844=LINE('',#22865,#986);
#845=LINE('',#22868,#987);
#846=LINE('',#22870,#988);
#847=LINE('',#22871,#989);
#848=LINE('',#22874,#990);
#849=LINE('',#22875,#991);
#850=LINE('',#22878,#992);
#851=LINE('',#22879,#993);
#852=LINE('',#22882,#994);
#853=LINE('',#22883,#995);
#854=LINE('',#22886,#996);
#855=LINE('',#22887,#997);
#856=LINE('',#22889,#998);
#857=LINE('',#22895,#999);
#858=LINE('',#23067,#1000);
#859=LINE('',#23487,#1001);
#860=LINE('',#23934,#1002);
#861=LINE('',#24387,#1003);
#862=LINE('',#24838,#1004);
#863=LINE('',#25321,#1005);
#864=LINE('',#25876,#1006);
#865=LINE('',#26325,#1007);
#866=LINE('',#26776,#1008);
#867=LINE('',#27215,#1009);
#868=LINE('',#27656,#1010);
#869=LINE('',#28135,#1011);
#870=LINE('',#28610,#1012);
#871=LINE('',#29133,#1013);
#872=LINE('',#29586,#1014);
#873=LINE('',#30023,#1015);
#874=LINE('',#30482,#1016);
#875=LINE('',#30943,#1017);
#876=LINE('',#31370,#1018);
#877=LINE('',#31798,#1019);
#878=LINE('',#32199,#1020);
#879=LINE('',#32217,#1021);
#880=LINE('',#32403,#1022);
#881=LINE('',#32751,#1023);
#882=LINE('',#33099,#1024);
#883=LINE('',#33447,#1025);
#884=LINE('',#33795,#1026);
#885=LINE('',#34143,#1027);
#886=LINE('',#34491,#1028);
#887=LINE('',#34839,#1029);
#888=LINE('',#35187,#1030);
#889=LINE('',#35535,#1031);
#890=LINE('',#35883,#1032);
#891=LINE('',#36231,#1033);
#892=LINE('',#36582,#1034);
#893=LINE('',#36933,#1035);
#894=LINE('',#37281,#1036);
#895=LINE('',#37632,#1037);
#896=LINE('',#37986,#1038);
#897=LINE('',#38334,#1039);
#898=LINE('',#38682,#1040);
#899=VECTOR('',#3490,1.08063175605657);
#900=VECTOR('',#3507,2.16126351211314);
#901=VECTOR('',#3516,2.5);
#902=VECTOR('',#3531,1.08063175605657);
#903=VECTOR('',#3548,3.90634189295527);
#904=VECTOR('',#3561,1.543);
#905=VECTOR('',#3566,1.543);
#906=VECTOR('',#3569,1.543);
#907=VECTOR('',#3574,1.2645);
#908=VECTOR('',#3579,1.2645);
#909=VECTOR('',#3582,1.2645);
#910=VECTOR('',#3591,10.);
#911=VECTOR('',#3592,9.99999999999999);
#912=VECTOR('',#3593,10.);
#913=VECTOR('',#3594,10.);
#914=VECTOR('',#3595,10.);
#915=VECTOR('',#3596,10.);
#916=VECTOR('',#3599,10.);
#917=VECTOR('',#3600,9.99999999999999);
#918=VECTOR('',#3601,10.);
#919=VECTOR('',#3604,10.);
#920=VECTOR('',#3605,10.);
#921=VECTOR('',#3608,10.);
#922=VECTOR('',#3609,10.);
#923=VECTOR('',#3612,10.);
#924=VECTOR('',#3613,10.);
#925=VECTOR('',#3616,10.);
#926=VECTOR('',#3617,10.);
#927=VECTOR('',#3620,10.);
#928=VECTOR('',#3629,1.08063175605657);
#929=VECTOR('',#3648,2.16126351211314);
#930=VECTOR('',#3657,2.5);
#931=VECTOR('',#3674,1.08063175605657);
#932=VECTOR('',#3685,1.08063175605657);
#933=VECTOR('',#3694,1.17775);
#934=VECTOR('',#3699,1.17775);
#935=VECTOR('',#3702,1.17775);
#936=VECTOR('',#3705,1.17775);
#937=VECTOR('',#3708,1.17775);
#938=VECTOR('',#3711,1.17775);
#939=VECTOR('',#3714,1.17775);
#940=VECTOR('',#3717,1.17775);
#941=VECTOR('',#3720,1.17775);
#942=VECTOR('',#3723,1.17775);
#943=VECTOR('',#3726,1.17775);
#944=VECTOR('',#3729,1.17775);
#945=VECTOR('',#3732,1.17775);
#946=VECTOR('',#3735,1.17775);
#947=VECTOR('',#3738,1.17775);
#948=VECTOR('',#3741,1.17775);
#949=VECTOR('',#3744,1.17775);
#950=VECTOR('',#3747,1.17775);
#951=VECTOR('',#3750,1.17775);
#952=VECTOR('',#3753,1.17775);
#953=VECTOR('',#3756,1.17775);
#954=VECTOR('',#3759,1.4635);
#955=VECTOR('',#3764,1.4635);
#956=VECTOR('',#3767,1.4635);
#957=VECTOR('',#3770,1.4635);
#958=VECTOR('',#3773,1.4635);
#959=VECTOR('',#3776,1.4635);
#960=VECTOR('',#3779,1.4635);
#961=VECTOR('',#3782,1.4635);
#962=VECTOR('',#3785,1.4635);
#963=VECTOR('',#3788,1.4635);
#964=VECTOR('',#3791,1.4635);
#965=VECTOR('',#3794,1.4635);
#966=VECTOR('',#3797,1.4635);
#967=VECTOR('',#3800,1.4635);
#968=VECTOR('',#3803,1.4635);
#969=VECTOR('',#3806,1.4635);
#970=VECTOR('',#3809,1.4635);
#971=VECTOR('',#3812,1.4635);
#972=VECTOR('',#3815,1.4635);
#973=VECTOR('',#3818,1.4635);
#974=VECTOR('',#3821,1.4635);
#975=VECTOR('',#3838,1.543);
#976=VECTOR('',#3843,1.543);
#977=VECTOR('',#3846,1.543);
#978=VECTOR('',#3851,1.2645);
#979=VECTOR('',#3856,1.2645);
#980=VECTOR('',#3859,1.2645);
#981=VECTOR('',#3868,10.);
#982=VECTOR('',#3869,9.99999999999999);
#983=VECTOR('',#3870,10.);
#984=VECTOR('',#3871,10.);
#985=VECTOR('',#3872,10.);
#986=VECTOR('',#3873,10.);
#987=VECTOR('',#3876,10.);
#988=VECTOR('',#3877,9.99999999999999);
#989=VECTOR('',#3878,10.);
#990=VECTOR('',#3881,10.);
#991=VECTOR('',#3882,10.);
#992=VECTOR('',#3885,10.);
#993=VECTOR('',#3886,10.);
#994=VECTOR('',#3889,10.);
#995=VECTOR('',#3890,10.);
#996=VECTOR('',#3893,10.);
#997=VECTOR('',#3894,10.);
#998=VECTOR('',#3897,10.);
#999=VECTOR('',#3904,1.17775);
#1000=VECTOR('',#3909,1.17775);
#1001=VECTOR('',#3912,1.17775);
#1002=VECTOR('',#3915,1.17775);
#1003=VECTOR('',#3918,1.17775);
#1004=VECTOR('',#3921,1.17775);
#1005=VECTOR('',#3924,1.17775);
#1006=VECTOR('',#3927,1.17775);
#1007=VECTOR('',#3930,1.17775);
#1008=VECTOR('',#3933,1.17775);
#1009=VECTOR('',#3936,1.17775);
#1010=VECTOR('',#3939,1.17775);
#1011=VECTOR('',#3942,1.17775);
#1012=VECTOR('',#3945,1.17775);
#1013=VECTOR('',#3948,1.17775);
#1014=VECTOR('',#3951,1.17775);
#1015=VECTOR('',#3954,1.17775);
#1016=VECTOR('',#3957,1.17775);
#1017=VECTOR('',#3960,1.17775);
#1018=VECTOR('',#3963,1.17775);
#1019=VECTOR('',#3966,1.17775);
#1020=VECTOR('',#3969,1.4635);
#1021=VECTOR('',#3974,1.4635);
#1022=VECTOR('',#3977,1.4635);
#1023=VECTOR('',#3980,1.4635);
#1024=VECTOR('',#3983,1.4635);
#1025=VECTOR('',#3986,1.4635);
#1026=VECTOR('',#3989,1.4635);
#1027=VECTOR('',#3992,1.4635);
#1028=VECTOR('',#3995,1.4635);
#1029=VECTOR('',#3998,1.4635);
#1030=VECTOR('',#4001,1.4635);
#1031=VECTOR('',#4004,1.4635);
#1032=VECTOR('',#4007,1.4635);
#1033=VECTOR('',#4010,1.4635);
#1034=VECTOR('',#4013,1.4635);
#1035=VECTOR('',#4016,1.4635);
#1036=VECTOR('',#4019,1.4635);
#1037=VECTOR('',#4022,1.4635);
#1038=VECTOR('',#4025,1.4635);
#1039=VECTOR('',#4028,1.4635);
#1040=VECTOR('',#4031,1.4635);
#1041=CIRCLE('',#3267,1.08063175605657);
#1042=CIRCLE('',#3268,1.08063175605657);
#1043=CIRCLE('',#3271,1.16126351211314);
#1044=CIRCLE('',#3272,1.);
#1045=CIRCLE('',#3273,2.16126351211314);
#1046=CIRCLE('',#3276,2.16126351211314);
#1047=CIRCLE('',#3277,2.16126351211314);
#1048=CIRCLE('',#3279,2.5);
#1049=CIRCLE('',#3280,2.5);
#1050=CIRCLE('',#3283,3.53951905042299);
#1051=CIRCLE('',#3286,1.08063175605657);
#1052=CIRCLE('',#3287,1.08063175605657);
#1053=CIRCLE('',#3289,2.90634189295526);
#1054=CIRCLE('',#3291,3.90634189295526);
#1055=CIRCLE('',#3292,1.);
#1056=CIRCLE('',#3294,3.90634189295527);
#1057=CIRCLE('',#3296,2.90634189295526);
#1058=CIRCLE('',#3297,0.999999999999996);
#1059=CIRCLE('',#3301,1.543);
#1060=CIRCLE('',#3304,1.543);
#1061=CIRCLE('',#3306,1.2645);
#1062=CIRCLE('',#3309,1.2645);
#1063=CIRCLE('',#3322,1.08063175605657);
#1064=CIRCLE('',#3323,1.08063175605657);
#1065=CIRCLE('',#3326,1.16126351211314);
#1066=CIRCLE('',#3327,1.);
#1067=CIRCLE('',#3328,2.16126351211314);
#1068=CIRCLE('',#3329,2.16126351211314);
#1069=CIRCLE('',#3332,2.16126351211314);
#1070=CIRCLE('',#3333,2.16126351211314);
#1071=CIRCLE('',#3335,2.5);
#1072=CIRCLE('',#3336,2.5);
#1073=CIRCLE('',#3339,3.53951905042299);
#1074=CIRCLE('',#3342,1.08063175605657);
#1075=CIRCLE('',#3344,1.08063175605657);
#1076=CIRCLE('',#3347,1.08063175605657);
#1077=CIRCLE('',#3349,1.08063175605657);
#1078=CIRCLE('',#3353,1.17775);
#1079=CIRCLE('',#3375,1.4635);
#1080=CIRCLE('',#3397,1.4635);
#1081=CIRCLE('',#3399,1.17775);
#1082=CIRCLE('',#3404,1.543);
#1083=CIRCLE('',#3407,1.543);
#1084=CIRCLE('',#3409,1.2645);
#1085=CIRCLE('',#3412,1.2645);
#1086=CIRCLE('',#3425,1.17775);
#1087=CIRCLE('',#3447,1.4635);
#1088=CIRCLE('',#3469,1.4635);
#1089=CIRCLE('',#3471,1.17775);
#1090=VERTEX_POINT('',#4063);
#1091=VERTEX_POINT('',#4065);
#1092=VERTEX_POINT('',#4070);
#1093=VERTEX_POINT('',#4072);
#1094=VERTEX_POINT('',#4077);
#1095=VERTEX_POINT('',#4079);
#1096=VERTEX_POINT('',#4083);
#1097=VERTEX_POINT('',#4085);
#1098=VERTEX_POINT('',#4090);
#1099=VERTEX_POINT('',#4094);
#1100=VERTEX_POINT('',#4096);
#1101=VERTEX_POINT('',#4100);
#1102=VERTEX_POINT('',#4103);
#1103=VERTEX_POINT('',#4107);
#1104=VERTEX_POINT('',#4111);
#1105=VERTEX_POINT('',#4117);
#1106=VERTEX_POINT('',#4118);
#1107=VERTEX_POINT('',#4120);
#1108=VERTEX_POINT('',#4127);
#1109=VERTEX_POINT('',#4206);
#1110=VERTEX_POINT('',#4207);
#1111=VERTEX_POINT('',#4209);
#1112=VERTEX_POINT('',#4328);
#1113=VERTEX_POINT('',#4509);
#1114=VERTEX_POINT('',#4510);
#1115=VERTEX_POINT('',#4512);
#1116=VERTEX_POINT('',#4574);
#1117=VERTEX_POINT('',#4580);
#1118=VERTEX_POINT('',#4582);
#1119=VERTEX_POINT('',#4643);
#1120=VERTEX_POINT('',#4644);
#1121=VERTEX_POINT('',#4646);
#1122=VERTEX_POINT('',#4699);
#1123=VERTEX_POINT('',#4714);
#1124=VERTEX_POINT('',#4799);
#1125=VERTEX_POINT('',#4800);
#1126=VERTEX_POINT('',#4802);
#1127=VERTEX_POINT('',#4979);
#1128=VERTEX_POINT('',#5116);
#1129=VERTEX_POINT('',#5117);
#1130=VERTEX_POINT('',#5119);
#1131=VERTEX_POINT('',#5172);
#1132=VERTEX_POINT('',#5275);
#1133=VERTEX_POINT('',#5452);
#1134=VERTEX_POINT('',#5630);
#1135=VERTEX_POINT('',#5703);
#1136=VERTEX_POINT('',#5973);
#1137=VERTEX_POINT('',#6397);
#1138=VERTEX_POINT('',#6398);
#1139=VERTEX_POINT('',#6400);
#1140=VERTEX_POINT('',#6402);
#1141=VERTEX_POINT('',#6404);
#1142=VERTEX_POINT('',#6406);
#1143=VERTEX_POINT('',#6410);
#1144=VERTEX_POINT('',#6412);
#1145=VERTEX_POINT('',#6416);
#1146=VERTEX_POINT('',#6420);
#1147=VERTEX_POINT('',#6424);
#1148=VERTEX_POINT('',#6428);
#1149=VERTEX_POINT('',#6436);
#1150=VERTEX_POINT('',#6438);
#1151=VERTEX_POINT('',#6443);
#1152=VERTEX_POINT('',#6445);
#1153=VERTEX_POINT('',#6447);
#1154=VERTEX_POINT('',#6452);
#1155=VERTEX_POINT('',#6454);
#1156=VERTEX_POINT('',#6458);
#1157=VERTEX_POINT('',#6460);
#1158=VERTEX_POINT('',#6465);
#1159=VERTEX_POINT('',#6469);
#1160=VERTEX_POINT('',#6472);
#1161=VERTEX_POINT('',#6477);
#1162=VERTEX_POINT('',#6480);
#1163=VERTEX_POINT('',#6486);
#1164=VERTEX_POINT('',#6487);
#1165=VERTEX_POINT('',#6489);
#1166=VERTEX_POINT('',#6594);
#1167=VERTEX_POINT('',#6652);
#1168=VERTEX_POINT('',#6653);
#1169=VERTEX_POINT('',#6875);
#1170=VERTEX_POINT('',#7080);
#1171=VERTEX_POINT('',#7081);
#1172=VERTEX_POINT('',#7083);
#1173=VERTEX_POINT('',#7527);
#1174=VERTEX_POINT('',#7528);
#1175=VERTEX_POINT('',#7748);
#1176=VERTEX_POINT('',#7974);
#1177=VERTEX_POINT('',#7975);
#1178=VERTEX_POINT('',#7977);
#1179=VERTEX_POINT('',#8419);
#1180=VERTEX_POINT('',#8420);
#1181=VERTEX_POINT('',#8642);
#1182=VERTEX_POINT('',#8868);
#1183=VERTEX_POINT('',#8869);
#1184=VERTEX_POINT('',#8871);
#1185=VERTEX_POINT('',#9309);
#1186=VERTEX_POINT('',#9310);
#1187=VERTEX_POINT('',#9534);
#1188=VERTEX_POINT('',#9756);
#1189=VERTEX_POINT('',#9757);
#1190=VERTEX_POINT('',#9759);
#1191=VERTEX_POINT('',#10207);
#1192=VERTEX_POINT('',#10208);
#1193=VERTEX_POINT('',#10420);
#1194=VERTEX_POINT('',#10644);
#1195=VERTEX_POINT('',#10645);
#1196=VERTEX_POINT('',#10647);
#1197=VERTEX_POINT('',#11119);
#1198=VERTEX_POINT('',#11120);
#1199=VERTEX_POINT('',#11338);
#1200=VERTEX_POINT('',#11572);
#1201=VERTEX_POINT('',#11573);
#1202=VERTEX_POINT('',#11575);
#1203=VERTEX_POINT('',#12021);
#1204=VERTEX_POINT('',#12022);
#1205=VERTEX_POINT('',#12246);
#1206=VERTEX_POINT('',#12468);
#1207=VERTEX_POINT('',#12469);
#1208=VERTEX_POINT('',#12471);
#1209=VERTEX_POINT('',#12921);
#1210=VERTEX_POINT('',#12922);
#1211=VERTEX_POINT('',#13132);
#1212=VERTEX_POINT('',#13398);
#1213=VERTEX_POINT('',#13399);
#1214=VERTEX_POINT('',#13401);
#1215=VERTEX_POINT('',#13853);
#1216=VERTEX_POINT('',#13854);
#1217=VERTEX_POINT('',#14068);
#1218=VERTEX_POINT('',#14324);
#1219=VERTEX_POINT('',#14325);
#1220=VERTEX_POINT('',#14327);
#1221=VERTEX_POINT('',#14761);
#1222=VERTEX_POINT('',#14762);
#1223=VERTEX_POINT('',#14980);
#1224=VERTEX_POINT('',#15179);
#1225=VERTEX_POINT('',#15180);
#1226=VERTEX_POINT('',#15182);
#1227=VERTEX_POINT('',#15399);
#1228=VERTEX_POINT('',#15632);
#1229=VERTEX_POINT('',#15633);
#1230=VERTEX_POINT('',#15635);
#1231=VERTEX_POINT('',#15642);
#1232=VERTEX_POINT('',#15650);
#1233=VERTEX_POINT('',#15651);
#1234=VERTEX_POINT('',#15836);
#1235=VERTEX_POINT('',#15837);
#1236=VERTEX_POINT('',#16022);
#1237=VERTEX_POINT('',#16023);
#1238=VERTEX_POINT('',#16370);
#1239=VERTEX_POINT('',#16371);
#1240=VERTEX_POINT('',#16394);
#1241=VERTEX_POINT('',#16395);
#1242=VERTEX_POINT('',#16418);
#1243=VERTEX_POINT('',#16419);
#1244=VERTEX_POINT('',#16605);
#1245=VERTEX_POINT('',#16606);
#1246=VERTEX_POINT('',#16953);
#1247=VERTEX_POINT('',#16954);
#1248=VERTEX_POINT('',#16977);
#1249=VERTEX_POINT('',#16978);
#1250=VERTEX_POINT('',#17003);
#1251=VERTEX_POINT('',#17004);
#1252=VERTEX_POINT('',#17189);
#1253=VERTEX_POINT('',#17190);
#1254=VERTEX_POINT('',#17537);
#1255=VERTEX_POINT('',#17538);
#1256=VERTEX_POINT('',#17563);
#1257=VERTEX_POINT('',#17564);
#1258=VERTEX_POINT('',#17587);
#1259=VERTEX_POINT('',#17588);
#1260=VERTEX_POINT('',#17773);
#1261=VERTEX_POINT('',#17774);
#1262=VERTEX_POINT('',#18121);
#1263=VERTEX_POINT('',#18122);
#1264=VERTEX_POINT('',#18145);
#1265=VERTEX_POINT('',#18146);
#1266=VERTEX_POINT('',#18169);
#1267=VERTEX_POINT('',#18170);
#1268=VERTEX_POINT('',#18356);
#1269=VERTEX_POINT('',#18357);
#1270=VERTEX_POINT('',#18704);
#1271=VERTEX_POINT('',#18705);
#1272=VERTEX_POINT('',#18728);
#1273=VERTEX_POINT('',#18738);
#1274=VERTEX_POINT('',#18749);
#1275=VERTEX_POINT('',#18970);
#1276=VERTEX_POINT('',#18972);
#1277=VERTEX_POINT('',#19690);
#1278=VERTEX_POINT('',#20326);
#1279=VERTEX_POINT('',#20487);
#1280=VERTEX_POINT('',#20488);
#1281=VERTEX_POINT('',#20490);
#1282=VERTEX_POINT('',#20497);
#1283=VERTEX_POINT('',#20576);
#1284=VERTEX_POINT('',#20577);
#1285=VERTEX_POINT('',#20579);
#1286=VERTEX_POINT('',#20698);
#1287=VERTEX_POINT('',#20879);
#1288=VERTEX_POINT('',#20880);
#1289=VERTEX_POINT('',#20882);
#1290=VERTEX_POINT('',#20944);
#1291=VERTEX_POINT('',#20982);
#1292=VERTEX_POINT('',#20984);
#1293=VERTEX_POINT('',#21099);
#1294=VERTEX_POINT('',#21100);
#1295=VERTEX_POINT('',#21102);
#1296=VERTEX_POINT('',#21155);
#1297=VERTEX_POINT('',#21170);
#1298=VERTEX_POINT('',#21253);
#1299=VERTEX_POINT('',#21254);
#1300=VERTEX_POINT('',#21256);
#1301=VERTEX_POINT('',#21548);
#1302=VERTEX_POINT('',#21549);
#1303=VERTEX_POINT('',#21551);
#1304=VERTEX_POINT('',#21586);
#1305=VERTEX_POINT('',#21689);
#1306=VERTEX_POINT('',#21983);
#1307=VERTEX_POINT('',#22160);
#1308=VERTEX_POINT('',#22430);
#1309=VERTEX_POINT('',#22854);
#1310=VERTEX_POINT('',#22855);
#1311=VERTEX_POINT('',#22857);
#1312=VERTEX_POINT('',#22859);
#1313=VERTEX_POINT('',#22861);
#1314=VERTEX_POINT('',#22863);
#1315=VERTEX_POINT('',#22867);
#1316=VERTEX_POINT('',#22869);
#1317=VERTEX_POINT('',#22873);
#1318=VERTEX_POINT('',#22877);
#1319=VERTEX_POINT('',#22881);
#1320=VERTEX_POINT('',#22885);
#1321=VERTEX_POINT('',#22893);
#1322=VERTEX_POINT('',#22894);
#1323=VERTEX_POINT('',#22896);
#1324=VERTEX_POINT('',#23007);
#1325=VERTEX_POINT('',#23065);
#1326=VERTEX_POINT('',#23066);
#1327=VERTEX_POINT('',#23288);
#1328=VERTEX_POINT('',#23485);
#1329=VERTEX_POINT('',#23486);
#1330=VERTEX_POINT('',#23488);
#1331=VERTEX_POINT('',#23932);
#1332=VERTEX_POINT('',#23933);
#1333=VERTEX_POINT('',#24153);
#1334=VERTEX_POINT('',#24385);
#1335=VERTEX_POINT('',#24386);
#1336=VERTEX_POINT('',#24388);
#1337=VERTEX_POINT('',#24836);
#1338=VERTEX_POINT('',#24837);
#1339=VERTEX_POINT('',#25059);
#1340=VERTEX_POINT('',#25319);
#1341=VERTEX_POINT('',#25320);
#1342=VERTEX_POINT('',#25322);
#1343=VERTEX_POINT('',#25874);
#1344=VERTEX_POINT('',#25875);
#1345=VERTEX_POINT('',#26097);
#1346=VERTEX_POINT('',#26323);
#1347=VERTEX_POINT('',#26324);
#1348=VERTEX_POINT('',#26326);
#1349=VERTEX_POINT('',#26774);
#1350=VERTEX_POINT('',#26775);
#1351=VERTEX_POINT('',#26985);
#1352=VERTEX_POINT('',#27213);
#1353=VERTEX_POINT('',#27214);
#1354=VERTEX_POINT('',#27216);
#1355=VERTEX_POINT('',#27654);
#1356=VERTEX_POINT('',#27655);
#1357=VERTEX_POINT('',#27877);
#1358=VERTEX_POINT('',#28133);
#1359=VERTEX_POINT('',#28134);
#1360=VERTEX_POINT('',#28136);
#1361=VERTEX_POINT('',#28608);
#1362=VERTEX_POINT('',#28609);
#1363=VERTEX_POINT('',#28835);
#1364=VERTEX_POINT('',#29131);
#1365=VERTEX_POINT('',#29132);
#1366=VERTEX_POINT('',#29134);
#1367=VERTEX_POINT('',#29584);
#1368=VERTEX_POINT('',#29585);
#1369=VERTEX_POINT('',#29799);
#1370=VERTEX_POINT('',#30021);
#1371=VERTEX_POINT('',#30022);
#1372=VERTEX_POINT('',#30024);
#1373=VERTEX_POINT('',#30480);
#1374=VERTEX_POINT('',#30481);
#1375=VERTEX_POINT('',#30695);
#1376=VERTEX_POINT('',#30941);
#1377=VERTEX_POINT('',#30942);
#1378=VERTEX_POINT('',#30944);
#1379=VERTEX_POINT('',#31368);
#1380=VERTEX_POINT('',#31369);
#1381=VERTEX_POINT('',#31591);
#1382=VERTEX_POINT('',#31796);
#1383=VERTEX_POINT('',#31797);
#1384=VERTEX_POINT('',#31799);
#1385=VERTEX_POINT('',#31986);
#1386=VERTEX_POINT('',#32197);
#1387=VERTEX_POINT('',#32198);
#1388=VERTEX_POINT('',#32200);
#1389=VERTEX_POINT('',#32207);
#1390=VERTEX_POINT('',#32215);
#1391=VERTEX_POINT('',#32216);
#1392=VERTEX_POINT('',#32401);
#1393=VERTEX_POINT('',#32402);
#1394=VERTEX_POINT('',#32749);
#1395=VERTEX_POINT('',#32750);
#1396=VERTEX_POINT('',#33097);
#1397=VERTEX_POINT('',#33098);
#1398=VERTEX_POINT('',#33445);
#1399=VERTEX_POINT('',#33446);
#1400=VERTEX_POINT('',#33793);
#1401=VERTEX_POINT('',#33794);
#1402=VERTEX_POINT('',#34141);
#1403=VERTEX_POINT('',#34142);
#1404=VERTEX_POINT('',#34489);
#1405=VERTEX_POINT('',#34490);
#1406=VERTEX_POINT('',#34837);
#1407=VERTEX_POINT('',#34838);
#1408=VERTEX_POINT('',#35185);
#1409=VERTEX_POINT('',#35186);
#1410=VERTEX_POINT('',#35533);
#1411=VERTEX_POINT('',#35534);
#1412=VERTEX_POINT('',#35881);
#1413=VERTEX_POINT('',#35882);
#1414=VERTEX_POINT('',#36229);
#1415=VERTEX_POINT('',#36230);
#1416=VERTEX_POINT('',#36580);
#1417=VERTEX_POINT('',#36581);
#1418=VERTEX_POINT('',#36931);
#1419=VERTEX_POINT('',#36932);
#1420=VERTEX_POINT('',#37279);
#1421=VERTEX_POINT('',#37280);
#1422=VERTEX_POINT('',#37630);
#1423=VERTEX_POINT('',#37631);
#1424=VERTEX_POINT('',#37984);
#1425=VERTEX_POINT('',#37985);
#1426=VERTEX_POINT('',#38332);
#1427=VERTEX_POINT('',#38333);
#1428=VERTEX_POINT('',#38680);
#1429=VERTEX_POINT('',#38681);
#1430=VERTEX_POINT('',#39034);
#1431=VERTEX_POINT('',#39044);
#1432=VERTEX_POINT('',#39055);
#1433=VERTEX_POINT('',#39192);
#1434=VERTEX_POINT('',#39194);
#1435=VERTEX_POINT('',#39909);
#1436=VERTEX_POINT('',#40545);
#1437=EDGE_CURVE('',#1090,#1090,#1041,.T.);
#1438=EDGE_CURVE('',#1090,#1091,#757,.T.);
#1439=EDGE_CURVE('',#1091,#1091,#1042,.T.);
#1440=EDGE_CURVE('',#1092,#1092,#1043,.T.);
#1441=EDGE_CURVE('',#1092,#1093,#1044,.T.);
#1442=EDGE_CURVE('',#1093,#1093,#1045,.T.);
#1443=EDGE_CURVE('',#1093,#1094,#758,.T.);
#1444=EDGE_CURVE('',#1094,#1095,#1046,.T.);
#1445=EDGE_CURVE('',#1095,#1094,#1047,.T.);
#1446=EDGE_CURVE('',#1096,#1096,#1048,.T.);
#1447=EDGE_CURVE('',#1096,#1097,#759,.T.);
#1448=EDGE_CURVE('',#1097,#1097,#1049,.T.);
#1449=EDGE_CURVE('',#1095,#1098,#1050,.T.);
#1450=EDGE_CURVE('',#1099,#1099,#1051,.T.);
#1451=EDGE_CURVE('',#1099,#1100,#760,.T.);
#1452=EDGE_CURVE('',#1100,#1100,#1052,.T.);
#1453=EDGE_CURVE('',#1101,#1101,#1053,.T.);
#1454=EDGE_CURVE('',#1102,#1102,#1054,.T.);
#1455=EDGE_CURVE('',#1102,#1101,#1055,.T.);
#1456=EDGE_CURVE('',#1103,#1103,#1056,.T.);
#1457=EDGE_CURVE('',#1103,#1102,#761,.T.);
#1458=EDGE_CURVE('',#1104,#1104,#1057,.T.);
#1459=EDGE_CURVE('',#1104,#1103,#1058,.T.);
#1460=EDGE_CURVE('',#1105,#1106,#762,.T.);
#1461=EDGE_CURVE('',#1106,#1107,#51,.T.);
#1462=EDGE_CURVE('',#1108,#1107,#1059,.T.);
#1463=EDGE_CURVE('',#1105,#1108,#52,.T.);
#1464=EDGE_CURVE('',#1109,#1110,#763,.T.);
#1465=EDGE_CURVE('',#1110,#1111,#53,.T.);
#1466=EDGE_CURVE('',#1111,#1106,#54,.T.);
#1467=EDGE_CURVE('',#1112,#1105,#55,.T.);
#1468=EDGE_CURVE('',#1109,#1112,#56,.T.);
#1469=EDGE_CURVE('',#1113,#1114,#764,.T.);
#1470=EDGE_CURVE('',#1115,#1113,#57,.T.);
#1471=EDGE_CURVE('',#1116,#1115,#58,.T.);
#1472=EDGE_CURVE('',#1117,#1116,#1060,.T.);
#1473=EDGE_CURVE('',#1117,#1118,#59,.T.);
#1474=EDGE_CURVE('',#1118,#1114,#60,.T.);
#1475=EDGE_CURVE('',#1119,#1120,#765,.T.);
#1476=EDGE_CURVE('',#1120,#1121,#61,.T.);
#1477=EDGE_CURVE('',#1121,#1122,#62,.T.);
#1478=EDGE_CURVE('',#1123,#1122,#1061,.T.);
#1479=EDGE_CURVE('',#1123,#1119,#63,.T.);
#1480=EDGE_CURVE('',#1124,#1125,#766,.T.);
#1481=EDGE_CURVE('',#1125,#1126,#64,.T.);
#1482=EDGE_CURVE('',#1126,#1120,#65,.T.);
#1483=EDGE_CURVE('',#1119,#1127,#66,.T.);
#1484=EDGE_CURVE('',#1127,#1124,#67,.T.);
#1485=EDGE_CURVE('',#1128,#1129,#767,.T.);
#1486=EDGE_CURVE('',#1128,#1130,#68,.T.);
#1487=EDGE_CURVE('',#1131,#1130,#1062,.F.);
#1488=EDGE_CURVE('',#1131,#1129,#69,.T.);
#1489=EDGE_CURVE('',#1129,#1132,#70,.T.);
#1490=EDGE_CURVE('',#1132,#1125,#71,.T.);
#1491=EDGE_CURVE('',#1124,#1133,#72,.T.);
#1492=EDGE_CURVE('',#1133,#1128,#73,.T.);
#1493=EDGE_CURVE('',#1114,#1134,#74,.T.);
#1494=EDGE_CURVE('',#1134,#1110,#75,.T.);
#1495=EDGE_CURVE('',#1135,#1109,#76,.T.);
#1496=EDGE_CURVE('',#1113,#1135,#77,.T.);
#1497=EDGE_CURVE('',#1107,#1136,#78,.T.);
#1498=EDGE_CURVE('',#1130,#1117,#79,.T.);
#1499=EDGE_CURVE('',#1136,#1123,#80,.T.);
#1500=EDGE_CURVE('',#1122,#1108,#81,.T.);
#1501=EDGE_CURVE('',#1116,#1131,#82,.T.);
#1502=EDGE_CURVE('',#1137,#1138,#768,.T.);
#1503=EDGE_CURVE('',#1138,#1139,#769,.T.);
#1504=EDGE_CURVE('',#1139,#1140,#770,.T.);
#1505=EDGE_CURVE('',#1140,#1141,#771,.T.);
#1506=EDGE_CURVE('',#1141,#1142,#772,.T.);
#1507=EDGE_CURVE('',#1142,#1137,#773,.T.);
#1508=EDGE_CURVE('',#1138,#1143,#774,.T.);
#1509=EDGE_CURVE('',#1144,#1143,#775,.T.);
#1510=EDGE_CURVE('',#1139,#1144,#776,.T.);
#1511=EDGE_CURVE('',#1145,#1144,#777,.T.);
#1512=EDGE_CURVE('',#1140,#1145,#778,.T.);
#1513=EDGE_CURVE('',#1146,#1145,#779,.T.);
#1514=EDGE_CURVE('',#1141,#1146,#780,.T.);
#1515=EDGE_CURVE('',#1147,#1146,#781,.T.);
#1516=EDGE_CURVE('',#1142,#1147,#782,.T.);
#1517=EDGE_CURVE('',#1148,#1147,#783,.T.);
#1518=EDGE_CURVE('',#1137,#1148,#784,.T.);
#1519=EDGE_CURVE('',#1143,#1148,#785,.T.);
#1520=EDGE_CURVE('',#1149,#1149,#1063,.T.);
#1521=EDGE_CURVE('',#1149,#1150,#786,.T.);
#1522=EDGE_CURVE('',#1150,#1150,#1064,.T.);
#1523=EDGE_CURVE('',#1151,#1151,#1065,.T.);
#1524=EDGE_CURVE('',#1151,#1152,#1066,.T.);
#1525=EDGE_CURVE('',#1152,#1153,#1067,.T.);
#1526=EDGE_CURVE('',#1153,#1152,#1068,.T.);
#1527=EDGE_CURVE('',#1153,#1154,#787,.T.);
#1528=EDGE_CURVE('',#1154,#1155,#1069,.T.);
#1529=EDGE_CURVE('',#1155,#1154,#1070,.T.);
#1530=EDGE_CURVE('',#1156,#1156,#1071,.T.);
#1531=EDGE_CURVE('',#1156,#1157,#788,.T.);
#1532=EDGE_CURVE('',#1157,#1157,#1072,.T.);
#1533=EDGE_CURVE('',#1155,#1158,#1073,.T.);
#1534=EDGE_CURVE('',#1159,#1159,#1074,.T.);
#1535=EDGE_CURVE('',#1159,#1160,#789,.T.);
#1536=EDGE_CURVE('',#1160,#1160,#1075,.T.);
#1537=EDGE_CURVE('',#1161,#1161,#1076,.T.);
#1538=EDGE_CURVE('',#1161,#1162,#790,.T.);
#1539=EDGE_CURVE('',#1162,#1162,#1077,.T.);
#1540=EDGE_CURVE('',#1163,#1164,#791,.T.);
#1541=EDGE_CURVE('',#1165,#1163,#83,.F.);
#1542=EDGE_CURVE('',#1166,#1165,#1078,.T.);
#1543=EDGE_CURVE('',#1166,#1164,#84,.T.);
#1544=EDGE_CURVE('',#1167,#1168,#792,.T.);
#1545=EDGE_CURVE('',#1163,#1167,#85,.F.);
#1546=EDGE_CURVE('',#1164,#1169,#86,.T.);
#1547=EDGE_CURVE('',#1169,#1168,#87,.T.);
#1548=EDGE_CURVE('',#1170,#1171,#793,.T.);
#1549=EDGE_CURVE('',#1172,#1170,#88,.F.);
#1550=EDGE_CURVE('',#1167,#1172,#89,.F.);
#1551=EDGE_CURVE('',#1168,#1171,#90,.T.);
#1552=EDGE_CURVE('',#1173,#1174,#794,.T.);
#1553=EDGE_CURVE('',#1170,#1173,#91,.F.);
#1554=EDGE_CURVE('',#1171,#1175,#92,.T.);
#1555=EDGE_CURVE('',#1175,#1174,#93,.T.);
#1556=EDGE_CURVE('',#1176,#1177,#795,.T.);
#1557=EDGE_CURVE('',#1178,#1176,#94,.F.);
#1558=EDGE_CURVE('',#1173,#1178,#95,.F.);
#1559=EDGE_CURVE('',#1174,#1177,#96,.T.);
#1560=EDGE_CURVE('',#1179,#1180,#796,.T.);
#1561=EDGE_CURVE('',#1176,#1179,#97,.F.);
#1562=EDGE_CURVE('',#1177,#1181,#98,.T.);
#1563=EDGE_CURVE('',#1181,#1180,#99,.T.);
#1564=EDGE_CURVE('',#1182,#1183,#797,.T.);
#1565=EDGE_CURVE('',#1184,#1182,#100,.F.);
#1566=EDGE_CURVE('',#1179,#1184,#101,.F.);
#1567=EDGE_CURVE('',#1180,#1183,#102,.T.);
#1568=EDGE_CURVE('',#1185,#1186,#798,.T.);
#1569=EDGE_CURVE('',#1182,#1185,#103,.F.);
#1570=EDGE_CURVE('',#1183,#1187,#104,.T.);
#1571=EDGE_CURVE('',#1187,#1186,#105,.T.);
#1572=EDGE_CURVE('',#1188,#1189,#799,.T.);
#1573=EDGE_CURVE('',#1190,#1188,#106,.F.);
#1574=EDGE_CURVE('',#1185,#1190,#107,.F.);
#1575=EDGE_CURVE('',#1186,#1189,#108,.T.);
#1576=EDGE_CURVE('',#1191,#1192,#800,.T.);
#1577=EDGE_CURVE('',#1188,#1191,#109,.F.);
#1578=EDGE_CURVE('',#1189,#1193,#110,.T.);
#1579=EDGE_CURVE('',#1193,#1192,#111,.T.);
#1580=EDGE_CURVE('',#1194,#1195,#801,.T.);
#1581=EDGE_CURVE('',#1196,#1194,#112,.F.);
#1582=EDGE_CURVE('',#1191,#1196,#113,.F.);
#1583=EDGE_CURVE('',#1192,#1195,#114,.T.);
#1584=EDGE_CURVE('',#1197,#1198,#802,.T.);
#1585=EDGE_CURVE('',#1194,#1197,#115,.F.);
#1586=EDGE_CURVE('',#1195,#1199,#116,.T.);
#1587=EDGE_CURVE('',#1199,#1198,#117,.T.);
#1588=EDGE_CURVE('',#1200,#1201,#803,.T.);
#1589=EDGE_CURVE('',#1202,#1200,#118,.F.);
#1590=EDGE_CURVE('',#1197,#1202,#119,.F.);
#1591=EDGE_CURVE('',#1198,#1201,#120,.T.);
#1592=EDGE_CURVE('',#1203,#1204,#804,.T.);
#1593=EDGE_CURVE('',#1200,#1203,#121,.F.);
#1594=EDGE_CURVE('',#1201,#1205,#122,.T.);
#1595=EDGE_CURVE('',#1205,#1204,#123,.T.);
#1596=EDGE_CURVE('',#1206,#1207,#805,.T.);
#1597=EDGE_CURVE('',#1208,#1206,#124,.F.);
#1598=EDGE_CURVE('',#1203,#1208,#125,.F.);
#1599=EDGE_CURVE('',#1204,#1207,#126,.T.);
#1600=EDGE_CURVE('',#1209,#1210,#806,.T.);
#1601=EDGE_CURVE('',#1206,#1209,#127,.F.);
#1602=EDGE_CURVE('',#1207,#1211,#128,.T.);
#1603=EDGE_CURVE('',#1211,#1210,#129,.T.);
#1604=EDGE_CURVE('',#1212,#1213,#807,.T.);
#1605=EDGE_CURVE('',#1214,#1212,#130,.F.);
#1606=EDGE_CURVE('',#1209,#1214,#131,.F.);
#1607=EDGE_CURVE('',#1210,#1213,#132,.T.);
#1608=EDGE_CURVE('',#1215,#1216,#808,.T.);
#1609=EDGE_CURVE('',#1212,#1215,#133,.F.);
#1610=EDGE_CURVE('',#1213,#1217,#134,.T.);
#1611=EDGE_CURVE('',#1217,#1216,#135,.T.);
#1612=EDGE_CURVE('',#1218,#1219,#809,.T.);
#1613=EDGE_CURVE('',#1220,#1218,#136,.F.);
#1614=EDGE_CURVE('',#1215,#1220,#137,.F.);
#1615=EDGE_CURVE('',#1216,#1219,#138,.T.);
#1616=EDGE_CURVE('',#1221,#1222,#810,.T.);
#1617=EDGE_CURVE('',#1218,#1221,#139,.F.);
#1618=EDGE_CURVE('',#1219,#1223,#140,.T.);
#1619=EDGE_CURVE('',#1223,#1222,#141,.T.);
#1620=EDGE_CURVE('',#1224,#1225,#811,.T.);
#1621=EDGE_CURVE('',#1226,#1224,#142,.T.);
#1622=EDGE_CURVE('',#1221,#1226,#143,.F.);
#1623=EDGE_CURVE('',#1222,#1227,#144,.T.);
#1624=EDGE_CURVE('',#1227,#1225,#145,.F.);
#1625=EDGE_CURVE('',#1228,#1229,#812,.T.);
#1626=EDGE_CURVE('',#1228,#1230,#146,.T.);
#1627=EDGE_CURVE('',#1231,#1230,#1079,.F.);
#1628=EDGE_CURVE('',#1231,#1229,#147,.T.);
#1629=EDGE_CURVE('',#1232,#1233,#813,.T.);
#1630=EDGE_CURVE('',#1232,#1228,#148,.T.);
#1631=EDGE_CURVE('',#1229,#1233,#149,.T.);
#1632=EDGE_CURVE('',#1234,#1235,#814,.T.);
#1633=EDGE_CURVE('',#1234,#1232,#150,.T.);
#1634=EDGE_CURVE('',#1233,#1235,#151,.T.);
#1635=EDGE_CURVE('',#1236,#1237,#815,.T.);
#1636=EDGE_CURVE('',#1236,#1234,#152,.T.);
#1637=EDGE_CURVE('',#1235,#1237,#153,.T.);
#1638=EDGE_CURVE('',#1238,#1239,#816,.T.);
#1639=EDGE_CURVE('',#1238,#1236,#154,.T.);
#1640=EDGE_CURVE('',#1237,#1239,#155,.T.);
#1641=EDGE_CURVE('',#1240,#1241,#817,.T.);
#1642=EDGE_CURVE('',#1240,#1238,#156,.T.);
#1643=EDGE_CURVE('',#1239,#1241,#157,.T.);
#1644=EDGE_CURVE('',#1242,#1243,#818,.T.);
#1645=EDGE_CURVE('',#1242,#1240,#158,.T.);
#1646=EDGE_CURVE('',#1241,#1243,#159,.T.);
#1647=EDGE_CURVE('',#1244,#1245,#819,.T.);
#1648=EDGE_CURVE('',#1244,#1242,#160,.T.);
#1649=EDGE_CURVE('',#1243,#1245,#161,.T.);
#1650=EDGE_CURVE('',#1246,#1247,#820,.T.);
#1651=EDGE_CURVE('',#1246,#1244,#162,.T.);
#1652=EDGE_CURVE('',#1245,#1247,#163,.T.);
#1653=EDGE_CURVE('',#1248,#1249,#821,.T.);
#1654=EDGE_CURVE('',#1248,#1246,#164,.T.);
#1655=EDGE_CURVE('',#1247,#1249,#165,.T.);
#1656=EDGE_CURVE('',#1250,#1251,#822,.T.);
#1657=EDGE_CURVE('',#1250,#1248,#166,.T.);
#1658=EDGE_CURVE('',#1249,#1251,#167,.T.);
#1659=EDGE_CURVE('',#1252,#1253,#823,.T.);
#1660=EDGE_CURVE('',#1252,#1250,#168,.T.);
#1661=EDGE_CURVE('',#1251,#1253,#169,.T.);
#1662=EDGE_CURVE('',#1254,#1255,#824,.T.);
#1663=EDGE_CURVE('',#1254,#1252,#170,.T.);
#1664=EDGE_CURVE('',#1253,#1255,#171,.T.);
#1665=EDGE_CURVE('',#1256,#1257,#825,.T.);
#1666=EDGE_CURVE('',#1256,#1254,#172,.T.);
#1667=EDGE_CURVE('',#1255,#1257,#173,.T.);
#1668=EDGE_CURVE('',#1258,#1259,#826,.T.);
#1669=EDGE_CURVE('',#1258,#1256,#174,.T.);
#1670=EDGE_CURVE('',#1257,#1259,#175,.T.);
#1671=EDGE_CURVE('',#1260,#1261,#827,.T.);
#1672=EDGE_CURVE('',#1260,#1258,#176,.T.);
#1673=EDGE_CURVE('',#1259,#1261,#177,.T.);
#1674=EDGE_CURVE('',#1262,#1263,#828,.T.);
#1675=EDGE_CURVE('',#1262,#1260,#178,.T.);
#1676=EDGE_CURVE('',#1261,#1263,#179,.T.);
#1677=EDGE_CURVE('',#1264,#1265,#829,.T.);
#1678=EDGE_CURVE('',#1264,#1262,#180,.T.);
#1679=EDGE_CURVE('',#1263,#1265,#181,.T.);
#1680=EDGE_CURVE('',#1266,#1267,#830,.T.);
#1681=EDGE_CURVE('',#1266,#1264,#182,.T.);
#1682=EDGE_CURVE('',#1265,#1267,#183,.T.);
#1683=EDGE_CURVE('',#1268,#1269,#831,.T.);
#1684=EDGE_CURVE('',#1268,#1266,#184,.T.);
#1685=EDGE_CURVE('',#1267,#1269,#185,.T.);
#1686=EDGE_CURVE('',#1270,#1271,#832,.T.);
#1687=EDGE_CURVE('',#1270,#1268,#186,.T.);
#1688=EDGE_CURVE('',#1269,#1271,#187,.T.);
#1689=EDGE_CURVE('',#1271,#1272,#188,.T.);
#1690=EDGE_CURVE('',#1273,#1272,#1080,.T.);
#1691=EDGE_CURVE('',#1273,#1270,#189,.T.);
#1692=EDGE_CURVE('',#1225,#1274,#190,.F.);
#1693=EDGE_CURVE('',#1275,#1274,#1081,.T.);
#1694=EDGE_CURVE('',#1276,#1275,#191,.T.);
#1695=EDGE_CURVE('',#1224,#1276,#192,.T.);
#1696=EDGE_CURVE('',#1272,#1275,#193,.T.);
#1697=EDGE_CURVE('',#1277,#1231,#194,.T.);
#1698=EDGE_CURVE('',#1277,#1165,#195,.T.);
#1699=EDGE_CURVE('',#1278,#1273,#196,.T.);
#1700=EDGE_CURVE('',#1274,#1278,#197,.T.);
#1701=EDGE_CURVE('',#1230,#1166,#198,.T.);
#1702=EDGE_CURVE('',#1279,#1280,#833,.T.);
#1703=EDGE_CURVE('',#1280,#1281,#199,.T.);
#1704=EDGE_CURVE('',#1282,#1281,#1082,.T.);
#1705=EDGE_CURVE('',#1279,#1282,#200,.T.);
#1706=EDGE_CURVE('',#1283,#1284,#834,.T.);
#1707=EDGE_CURVE('',#1284,#1285,#201,.T.);
#1708=EDGE_CURVE('',#1285,#1280,#202,.T.);
#1709=EDGE_CURVE('',#1286,#1279,#203,.T.);
#1710=EDGE_CURVE('',#1283,#1286,#204,.T.);
#1711=EDGE_CURVE('',#1287,#1288,#835,.T.);
#1712=EDGE_CURVE('',#1289,#1287,#205,.T.);
#1713=EDGE_CURVE('',#1290,#1289,#206,.T.);
#1714=EDGE_CURVE('',#1291,#1290,#1083,.T.);
#1715=EDGE_CURVE('',#1291,#1292,#207,.T.);
#1716=EDGE_CURVE('',#1292,#1288,#208,.T.);
#1717=EDGE_CURVE('',#1293,#1294,#836,.T.);
#1718=EDGE_CURVE('',#1294,#1295,#209,.T.);
#1719=EDGE_CURVE('',#1295,#1296,#210,.T.);
#1720=EDGE_CURVE('',#1297,#1296,#1084,.T.);
#1721=EDGE_CURVE('',#1297,#1293,#211,.T.);
#1722=EDGE_CURVE('',#1298,#1299,#837,.T.);
#1723=EDGE_CURVE('',#1299,#1300,#212,.T.);
#1724=EDGE_CURVE('',#1300,#1294,#213,.T.);
#1725=EDGE_CURVE('',#1293,#1298,#214,.T.);
#1726=EDGE_CURVE('',#1301,#1302,#838,.T.);
#1727=EDGE_CURVE('',#1301,#1303,#215,.T.);
#1728=EDGE_CURVE('',#1304,#1303,#1085,.F.);
#1729=EDGE_CURVE('',#1304,#1302,#216,.T.);
#1730=EDGE_CURVE('',#1302,#1305,#217,.T.);
#1731=EDGE_CURVE('',#1305,#1299,#218,.T.);
#1732=EDGE_CURVE('',#1298,#1301,#219,.T.);
#1733=EDGE_CURVE('',#1288,#1306,#220,.T.);
#1734=EDGE_CURVE('',#1306,#1284,#221,.T.);
#1735=EDGE_CURVE('',#1307,#1283,#222,.T.);
#1736=EDGE_CURVE('',#1287,#1307,#223,.T.);
#1737=EDGE_CURVE('',#1281,#1308,#224,.T.);
#1738=EDGE_CURVE('',#1303,#1291,#225,.T.);
#1739=EDGE_CURVE('',#1308,#1297,#226,.T.);
#1740=EDGE_CURVE('',#1296,#1282,#227,.T.);
#1741=EDGE_CURVE('',#1290,#1304,#228,.T.);
#1742=EDGE_CURVE('',#1309,#1310,#839,.T.);
#1743=EDGE_CURVE('',#1310,#1311,#840,.T.);
#1744=EDGE_CURVE('',#1311,#1312,#841,.T.);
#1745=EDGE_CURVE('',#1312,#1313,#842,.T.);
#1746=EDGE_CURVE('',#1313,#1314,#843,.T.);
#1747=EDGE_CURVE('',#1314,#1309,#844,.T.);
#1748=EDGE_CURVE('',#1310,#1315,#845,.T.);
#1749=EDGE_CURVE('',#1316,#1315,#846,.T.);
#1750=EDGE_CURVE('',#1311,#1316,#847,.T.);
#1751=EDGE_CURVE('',#1317,#1316,#848,.T.);
#1752=EDGE_CURVE('',#1312,#1317,#849,.T.);
#1753=EDGE_CURVE('',#1318,#1317,#850,.T.);
#1754=EDGE_CURVE('',#1313,#1318,#851,.T.);
#1755=EDGE_CURVE('',#1319,#1318,#852,.T.);
#1756=EDGE_CURVE('',#1314,#1319,#853,.T.);
#1757=EDGE_CURVE('',#1320,#1319,#854,.T.);
#1758=EDGE_CURVE('',#1309,#1320,#855,.T.);
#1759=EDGE_CURVE('',#1315,#1320,#856,.T.);
#1760=EDGE_CURVE('',#1321,#1322,#857,.T.);
#1761=EDGE_CURVE('',#1323,#1321,#229,.F.);
#1762=EDGE_CURVE('',#1324,#1323,#1086,.T.);
#1763=EDGE_CURVE('',#1324,#1322,#230,.T.);
#1764=EDGE_CURVE('',#1325,#1326,#858,.T.);
#1765=EDGE_CURVE('',#1321,#1325,#231,.F.);
#1766=EDGE_CURVE('',#1322,#1327,#232,.T.);
#1767=EDGE_CURVE('',#1327,#1326,#233,.T.);
#1768=EDGE_CURVE('',#1328,#1329,#859,.T.);
#1769=EDGE_CURVE('',#1330,#1328,#234,.F.);
#1770=EDGE_CURVE('',#1325,#1330,#235,.F.);
#1771=EDGE_CURVE('',#1326,#1329,#236,.T.);
#1772=EDGE_CURVE('',#1331,#1332,#860,.T.);
#1773=EDGE_CURVE('',#1328,#1331,#237,.F.);
#1774=EDGE_CURVE('',#1329,#1333,#238,.T.);
#1775=EDGE_CURVE('',#1333,#1332,#239,.T.);
#1776=EDGE_CURVE('',#1334,#1335,#861,.T.);
#1777=EDGE_CURVE('',#1336,#1334,#240,.F.);
#1778=EDGE_CURVE('',#1331,#1336,#241,.F.);
#1779=EDGE_CURVE('',#1332,#1335,#242,.T.);
#1780=EDGE_CURVE('',#1337,#1338,#862,.T.);
#1781=EDGE_CURVE('',#1334,#1337,#243,.F.);
#1782=EDGE_CURVE('',#1335,#1339,#244,.T.);
#1783=EDGE_CURVE('',#1339,#1338,#245,.T.);
#1784=EDGE_CURVE('',#1340,#1341,#863,.T.);
#1785=EDGE_CURVE('',#1342,#1340,#246,.F.);
#1786=EDGE_CURVE('',#1337,#1342,#247,.F.);
#1787=EDGE_CURVE('',#1338,#1341,#248,.T.);
#1788=EDGE_CURVE('',#1343,#1344,#864,.T.);
#1789=EDGE_CURVE('',#1340,#1343,#249,.F.);
#1790=EDGE_CURVE('',#1341,#1345,#250,.T.);
#1791=EDGE_CURVE('',#1345,#1344,#251,.T.);
#1792=EDGE_CURVE('',#1346,#1347,#865,.T.);
#1793=EDGE_CURVE('',#1348,#1346,#252,.F.);
#1794=EDGE_CURVE('',#1343,#1348,#253,.F.);
#1795=EDGE_CURVE('',#1344,#1347,#254,.T.);
#1796=EDGE_CURVE('',#1349,#1350,#866,.T.);
#1797=EDGE_CURVE('',#1346,#1349,#255,.F.);
#1798=EDGE_CURVE('',#1347,#1351,#256,.T.);
#1799=EDGE_CURVE('',#1351,#1350,#257,.T.);
#1800=EDGE_CURVE('',#1352,#1353,#867,.T.);
#1801=EDGE_CURVE('',#1354,#1352,#258,.F.);
#1802=EDGE_CURVE('',#1349,#1354,#259,.F.);
#1803=EDGE_CURVE('',#1350,#1353,#260,.T.);
#1804=EDGE_CURVE('',#1355,#1356,#868,.T.);
#1805=EDGE_CURVE('',#1352,#1355,#261,.F.);
#1806=EDGE_CURVE('',#1353,#1357,#262,.T.);
#1807=EDGE_CURVE('',#1357,#1356,#263,.T.);
#1808=EDGE_CURVE('',#1358,#1359,#869,.T.);
#1809=EDGE_CURVE('',#1360,#1358,#264,.F.);
#1810=EDGE_CURVE('',#1355,#1360,#265,.F.);
#1811=EDGE_CURVE('',#1356,#1359,#266,.T.);
#1812=EDGE_CURVE('',#1361,#1362,#870,.T.);
#1813=EDGE_CURVE('',#1358,#1361,#267,.F.);
#1814=EDGE_CURVE('',#1359,#1363,#268,.T.);
#1815=EDGE_CURVE('',#1363,#1362,#269,.T.);
#1816=EDGE_CURVE('',#1364,#1365,#871,.T.);
#1817=EDGE_CURVE('',#1366,#1364,#270,.F.);
#1818=EDGE_CURVE('',#1361,#1366,#271,.F.);
#1819=EDGE_CURVE('',#1362,#1365,#272,.T.);
#1820=EDGE_CURVE('',#1367,#1368,#872,.T.);
#1821=EDGE_CURVE('',#1364,#1367,#273,.F.);
#1822=EDGE_CURVE('',#1365,#1369,#274,.T.);
#1823=EDGE_CURVE('',#1369,#1368,#275,.T.);
#1824=EDGE_CURVE('',#1370,#1371,#873,.T.);
#1825=EDGE_CURVE('',#1372,#1370,#276,.F.);
#1826=EDGE_CURVE('',#1367,#1372,#277,.F.);
#1827=EDGE_CURVE('',#1368,#1371,#278,.T.);
#1828=EDGE_CURVE('',#1373,#1374,#874,.T.);
#1829=EDGE_CURVE('',#1370,#1373,#279,.F.);
#1830=EDGE_CURVE('',#1371,#1375,#280,.T.);
#1831=EDGE_CURVE('',#1375,#1374,#281,.T.);
#1832=EDGE_CURVE('',#1376,#1377,#875,.T.);
#1833=EDGE_CURVE('',#1378,#1376,#282,.F.);
#1834=EDGE_CURVE('',#1373,#1378,#283,.F.);
#1835=EDGE_CURVE('',#1374,#1377,#284,.T.);
#1836=EDGE_CURVE('',#1379,#1380,#876,.T.);
#1837=EDGE_CURVE('',#1376,#1379,#285,.F.);
#1838=EDGE_CURVE('',#1377,#1381,#286,.T.);
#1839=EDGE_CURVE('',#1381,#1380,#287,.T.);
#1840=EDGE_CURVE('',#1382,#1383,#877,.T.);
#1841=EDGE_CURVE('',#1384,#1382,#288,.T.);
#1842=EDGE_CURVE('',#1379,#1384,#289,.F.);
#1843=EDGE_CURVE('',#1380,#1385,#290,.T.);
#1844=EDGE_CURVE('',#1385,#1383,#291,.F.);
#1845=EDGE_CURVE('',#1386,#1387,#878,.T.);
#1846=EDGE_CURVE('',#1386,#1388,#292,.T.);
#1847=EDGE_CURVE('',#1389,#1388,#1087,.F.);
#1848=EDGE_CURVE('',#1389,#1387,#293,.T.);
#1849=EDGE_CURVE('',#1390,#1391,#879,.T.);
#1850=EDGE_CURVE('',#1390,#1386,#294,.T.);
#1851=EDGE_CURVE('',#1387,#1391,#295,.T.);
#1852=EDGE_CURVE('',#1392,#1393,#880,.T.);
#1853=EDGE_CURVE('',#1392,#1390,#296,.T.);
#1854=EDGE_CURVE('',#1391,#1393,#297,.T.);
#1855=EDGE_CURVE('',#1394,#1395,#881,.T.);
#1856=EDGE_CURVE('',#1394,#1392,#298,.T.);
#1857=EDGE_CURVE('',#1393,#1395,#299,.T.);
#1858=EDGE_CURVE('',#1396,#1397,#882,.T.);
#1859=EDGE_CURVE('',#1396,#1394,#300,.T.);
#1860=EDGE_CURVE('',#1395,#1397,#301,.T.);
#1861=EDGE_CURVE('',#1398,#1399,#883,.T.);
#1862=EDGE_CURVE('',#1398,#1396,#302,.T.);
#1863=EDGE_CURVE('',#1397,#1399,#303,.T.);
#1864=EDGE_CURVE('',#1400,#1401,#884,.T.);
#1865=EDGE_CURVE('',#1400,#1398,#304,.T.);
#1866=EDGE_CURVE('',#1399,#1401,#305,.T.);
#1867=EDGE_CURVE('',#1402,#1403,#885,.T.);
#1868=EDGE_CURVE('',#1402,#1400,#306,.T.);
#1869=EDGE_CURVE('',#1401,#1403,#307,.T.);
#1870=EDGE_CURVE('',#1404,#1405,#886,.T.);
#1871=EDGE_CURVE('',#1404,#1402,#308,.T.);
#1872=EDGE_CURVE('',#1403,#1405,#309,.T.);
#1873=EDGE_CURVE('',#1406,#1407,#887,.T.);
#1874=EDGE_CURVE('',#1406,#1404,#310,.T.);
#1875=EDGE_CURVE('',#1405,#1407,#311,.T.);
#1876=EDGE_CURVE('',#1408,#1409,#888,.T.);
#1877=EDGE_CURVE('',#1408,#1406,#312,.T.);
#1878=EDGE_CURVE('',#1407,#1409,#313,.T.);
#1879=EDGE_CURVE('',#1410,#1411,#889,.T.);
#1880=EDGE_CURVE('',#1410,#1408,#314,.T.);
#1881=EDGE_CURVE('',#1409,#1411,#315,.T.);
#1882=EDGE_CURVE('',#1412,#1413,#890,.T.);
#1883=EDGE_CURVE('',#1412,#1410,#316,.T.);
#1884=EDGE_CURVE('',#1411,#1413,#317,.T.);
#1885=EDGE_CURVE('',#1414,#1415,#891,.T.);
#1886=EDGE_CURVE('',#1414,#1412,#318,.T.);
#1887=EDGE_CURVE('',#1413,#1415,#319,.T.);
#1888=EDGE_CURVE('',#1416,#1417,#892,.T.);
#1889=EDGE_CURVE('',#1416,#1414,#320,.T.);
#1890=EDGE_CURVE('',#1415,#1417,#321,.T.);
#1891=EDGE_CURVE('',#1418,#1419,#893,.T.);
#1892=EDGE_CURVE('',#1418,#1416,#322,.T.);
#1893=EDGE_CURVE('',#1417,#1419,#323,.T.);
#1894=EDGE_CURVE('',#1420,#1421,#894,.T.);
#1895=EDGE_CURVE('',#1420,#1418,#324,.T.);
#1896=EDGE_CURVE('',#1419,#1421,#325,.T.);
#1897=EDGE_CURVE('',#1422,#1423,#895,.T.);
#1898=EDGE_CURVE('',#1422,#1420,#326,.T.);
#1899=EDGE_CURVE('',#1421,#1423,#327,.T.);
#1900=EDGE_CURVE('',#1424,#1425,#896,.T.);
#1901=EDGE_CURVE('',#1424,#1422,#328,.T.);
#1902=EDGE_CURVE('',#1423,#1425,#329,.T.);
#1903=EDGE_CURVE('',#1426,#1427,#897,.T.);
#1904=EDGE_CURVE('',#1426,#1424,#330,.T.);
#1905=EDGE_CURVE('',#1425,#1427,#331,.T.);
#1906=EDGE_CURVE('',#1428,#1429,#898,.T.);
#1907=EDGE_CURVE('',#1428,#1426,#332,.T.);
#1908=EDGE_CURVE('',#1427,#1429,#333,.T.);
#1909=EDGE_CURVE('',#1429,#1430,#334,.T.);
#1910=EDGE_CURVE('',#1431,#1430,#1088,.T.);
#1911=EDGE_CURVE('',#1431,#1428,#335,.T.);
#1912=EDGE_CURVE('',#1383,#1432,#336,.F.);
#1913=EDGE_CURVE('',#1433,#1432,#1089,.T.);
#1914=EDGE_CURVE('',#1434,#1433,#337,.T.);
#1915=EDGE_CURVE('',#1382,#1434,#338,.T.);
#1916=EDGE_CURVE('',#1430,#1433,#339,.T.);
#1917=EDGE_CURVE('',#1435,#1389,#340,.T.);
#1918=EDGE_CURVE('',#1435,#1323,#341,.T.);
#1919=EDGE_CURVE('',#1436,#1431,#342,.T.);
#1920=EDGE_CURVE('',#1432,#1436,#343,.T.);
#1921=EDGE_CURVE('',#1388,#1324,#344,.T.);
#1922=ORIENTED_EDGE('',*,*,#1437,.F.);
#1923=ORIENTED_EDGE('',*,*,#1438,.T.);
#1924=ORIENTED_EDGE('',*,*,#1439,.T.);
#1925=ORIENTED_EDGE('',*,*,#1438,.F.);
#1926=ORIENTED_EDGE('',*,*,#1439,.F.);
#1927=ORIENTED_EDGE('',*,*,#1440,.T.);
#1928=ORIENTED_EDGE('',*,*,#1441,.T.);
#1929=ORIENTED_EDGE('',*,*,#1442,.T.);
#1930=ORIENTED_EDGE('',*,*,#1441,.F.);
#1931=ORIENTED_EDGE('',*,*,#1440,.F.);
#1932=ORIENTED_EDGE('',*,*,#1437,.T.);
#1933=ORIENTED_EDGE('',*,*,#1442,.F.);
#1934=ORIENTED_EDGE('',*,*,#1443,.T.);
#1935=ORIENTED_EDGE('',*,*,#1444,.T.);
#1936=ORIENTED_EDGE('',*,*,#1445,.T.);
#1937=ORIENTED_EDGE('',*,*,#1443,.F.);
#1938=ORIENTED_EDGE('',*,*,#1446,.T.);
#1939=ORIENTED_EDGE('',*,*,#1447,.T.);
#1940=ORIENTED_EDGE('',*,*,#1448,.F.);
#1941=ORIENTED_EDGE('',*,*,#1447,.F.);
#1942=ORIENTED_EDGE('',*,*,#1446,.F.);
#1943=ORIENTED_EDGE('',*,*,#1445,.F.);
#1944=ORIENTED_EDGE('',*,*,#1449,.T.);
#1945=ORIENTED_EDGE('',*,*,#1449,.F.);
#1946=ORIENTED_EDGE('',*,*,#1444,.F.);
#1947=ORIENTED_EDGE('',*,*,#1448,.T.);
#1948=ORIENTED_EDGE('',*,*,#1450,.F.);
#1949=ORIENTED_EDGE('',*,*,#1451,.T.);
#1950=ORIENTED_EDGE('',*,*,#1452,.F.);
#1951=ORIENTED_EDGE('',*,*,#1451,.F.);
#1952=ORIENTED_EDGE('',*,*,#1453,.F.);
#1953=ORIENTED_EDGE('',*,*,#1452,.T.);
#1954=ORIENTED_EDGE('',*,*,#1454,.F.);
#1955=ORIENTED_EDGE('',*,*,#1455,.T.);
#1956=ORIENTED_EDGE('',*,*,#1453,.T.);
#1957=ORIENTED_EDGE('',*,*,#1455,.F.);
#1958=ORIENTED_EDGE('',*,*,#1456,.F.);
#1959=ORIENTED_EDGE('',*,*,#1457,.T.);
#1960=ORIENTED_EDGE('',*,*,#1454,.T.);
#1961=ORIENTED_EDGE('',*,*,#1457,.F.);
#1962=ORIENTED_EDGE('',*,*,#1458,.F.);
#1963=ORIENTED_EDGE('',*,*,#1459,.T.);
#1964=ORIENTED_EDGE('',*,*,#1456,.T.);
#1965=ORIENTED_EDGE('',*,*,#1459,.F.);
#1966=ORIENTED_EDGE('',*,*,#1458,.T.);
#1967=ORIENTED_EDGE('',*,*,#1450,.T.);
#1968=ORIENTED_EDGE('',*,*,#1460,.T.);
#1969=ORIENTED_EDGE('',*,*,#1461,.T.);
#1970=ORIENTED_EDGE('',*,*,#1462,.F.);
#1971=ORIENTED_EDGE('',*,*,#1463,.F.);
#1972=ORIENTED_EDGE('',*,*,#1464,.T.);
#1973=ORIENTED_EDGE('',*,*,#1465,.T.);
#1974=ORIENTED_EDGE('',*,*,#1466,.T.);
#1975=ORIENTED_EDGE('',*,*,#1460,.F.);
#1976=ORIENTED_EDGE('',*,*,#1467,.F.);
#1977=ORIENTED_EDGE('',*,*,#1468,.F.);
#1978=ORIENTED_EDGE('',*,*,#1469,.F.);
#1979=ORIENTED_EDGE('',*,*,#1470,.F.);
#1980=ORIENTED_EDGE('',*,*,#1471,.F.);
#1981=ORIENTED_EDGE('',*,*,#1472,.F.);
#1982=ORIENTED_EDGE('',*,*,#1473,.T.);
#1983=ORIENTED_EDGE('',*,*,#1474,.T.);
#1984=ORIENTED_EDGE('',*,*,#1475,.T.);
#1985=ORIENTED_EDGE('',*,*,#1476,.T.);
#1986=ORIENTED_EDGE('',*,*,#1477,.T.);
#1987=ORIENTED_EDGE('',*,*,#1478,.F.);
#1988=ORIENTED_EDGE('',*,*,#1479,.T.);
#1989=ORIENTED_EDGE('',*,*,#1480,.T.);
#1990=ORIENTED_EDGE('',*,*,#1481,.T.);
#1991=ORIENTED_EDGE('',*,*,#1482,.T.);
#1992=ORIENTED_EDGE('',*,*,#1475,.F.);
#1993=ORIENTED_EDGE('',*,*,#1483,.T.);
#1994=ORIENTED_EDGE('',*,*,#1484,.T.);
#1995=ORIENTED_EDGE('',*,*,#1485,.F.);
#1996=ORIENTED_EDGE('',*,*,#1486,.T.);
#1997=ORIENTED_EDGE('',*,*,#1487,.F.);
#1998=ORIENTED_EDGE('',*,*,#1488,.T.);
#1999=ORIENTED_EDGE('',*,*,#1485,.T.);
#2000=ORIENTED_EDGE('',*,*,#1489,.T.);
#2001=ORIENTED_EDGE('',*,*,#1490,.T.);
#2002=ORIENTED_EDGE('',*,*,#1480,.F.);
#2003=ORIENTED_EDGE('',*,*,#1491,.T.);
#2004=ORIENTED_EDGE('',*,*,#1492,.T.);
#2005=ORIENTED_EDGE('',*,*,#1469,.T.);
#2006=ORIENTED_EDGE('',*,*,#1493,.T.);
#2007=ORIENTED_EDGE('',*,*,#1494,.T.);
#2008=ORIENTED_EDGE('',*,*,#1464,.F.);
#2009=ORIENTED_EDGE('',*,*,#1495,.F.);
#2010=ORIENTED_EDGE('',*,*,#1496,.F.);
#2011=ORIENTED_EDGE('',*,*,#1497,.F.);
#2012=ORIENTED_EDGE('',*,*,#1461,.F.);
#2013=ORIENTED_EDGE('',*,*,#1466,.F.);
#2014=ORIENTED_EDGE('',*,*,#1465,.F.);
#2015=ORIENTED_EDGE('',*,*,#1494,.F.);
#2016=ORIENTED_EDGE('',*,*,#1493,.F.);
#2017=ORIENTED_EDGE('',*,*,#1474,.F.);
#2018=ORIENTED_EDGE('',*,*,#1473,.F.);
#2019=ORIENTED_EDGE('',*,*,#1498,.F.);
#2020=ORIENTED_EDGE('',*,*,#1486,.F.);
#2021=ORIENTED_EDGE('',*,*,#1492,.F.);
#2022=ORIENTED_EDGE('',*,*,#1491,.F.);
#2023=ORIENTED_EDGE('',*,*,#1484,.F.);
#2024=ORIENTED_EDGE('',*,*,#1483,.F.);
#2025=ORIENTED_EDGE('',*,*,#1479,.F.);
#2026=ORIENTED_EDGE('',*,*,#1499,.F.);
#2027=ORIENTED_EDGE('',*,*,#1500,.F.);
#2028=ORIENTED_EDGE('',*,*,#1477,.F.);
#2029=ORIENTED_EDGE('',*,*,#1476,.F.);
#2030=ORIENTED_EDGE('',*,*,#1482,.F.);
#2031=ORIENTED_EDGE('',*,*,#1481,.F.);
#2032=ORIENTED_EDGE('',*,*,#1490,.F.);
#2033=ORIENTED_EDGE('',*,*,#1489,.F.);
#2034=ORIENTED_EDGE('',*,*,#1488,.F.);
#2035=ORIENTED_EDGE('',*,*,#1501,.F.);
#2036=ORIENTED_EDGE('',*,*,#1471,.T.);
#2037=ORIENTED_EDGE('',*,*,#1470,.T.);
#2038=ORIENTED_EDGE('',*,*,#1496,.T.);
#2039=ORIENTED_EDGE('',*,*,#1495,.T.);
#2040=ORIENTED_EDGE('',*,*,#1468,.T.);
#2041=ORIENTED_EDGE('',*,*,#1467,.T.);
#2042=ORIENTED_EDGE('',*,*,#1463,.T.);
#2043=ORIENTED_EDGE('',*,*,#1502,.T.);
#2044=ORIENTED_EDGE('',*,*,#1503,.T.);
#2045=ORIENTED_EDGE('',*,*,#1504,.T.);
#2046=ORIENTED_EDGE('',*,*,#1505,.T.);
#2047=ORIENTED_EDGE('',*,*,#1506,.T.);
#2048=ORIENTED_EDGE('',*,*,#1507,.T.);
#2049=ORIENTED_EDGE('',*,*,#1498,.T.);
#2050=ORIENTED_EDGE('',*,*,#1472,.T.);
#2051=ORIENTED_EDGE('',*,*,#1501,.T.);
#2052=ORIENTED_EDGE('',*,*,#1487,.T.);
#2053=ORIENTED_EDGE('',*,*,#1503,.F.);
#2054=ORIENTED_EDGE('',*,*,#1508,.T.);
#2055=ORIENTED_EDGE('',*,*,#1509,.F.);
#2056=ORIENTED_EDGE('',*,*,#1510,.F.);
#2057=ORIENTED_EDGE('',*,*,#1504,.F.);
#2058=ORIENTED_EDGE('',*,*,#1510,.T.);
#2059=ORIENTED_EDGE('',*,*,#1511,.F.);
#2060=ORIENTED_EDGE('',*,*,#1512,.F.);
#2061=ORIENTED_EDGE('',*,*,#1505,.F.);
#2062=ORIENTED_EDGE('',*,*,#1512,.T.);
#2063=ORIENTED_EDGE('',*,*,#1513,.F.);
#2064=ORIENTED_EDGE('',*,*,#1514,.F.);
#2065=ORIENTED_EDGE('',*,*,#1506,.F.);
#2066=ORIENTED_EDGE('',*,*,#1514,.T.);
#2067=ORIENTED_EDGE('',*,*,#1515,.F.);
#2068=ORIENTED_EDGE('',*,*,#1516,.F.);
#2069=ORIENTED_EDGE('',*,*,#1507,.F.);
#2070=ORIENTED_EDGE('',*,*,#1516,.T.);
#2071=ORIENTED_EDGE('',*,*,#1517,.F.);
#2072=ORIENTED_EDGE('',*,*,#1518,.F.);
#2073=ORIENTED_EDGE('',*,*,#1502,.F.);
#2074=ORIENTED_EDGE('',*,*,#1518,.T.);
#2075=ORIENTED_EDGE('',*,*,#1519,.F.);
#2076=ORIENTED_EDGE('',*,*,#1508,.F.);
#2077=ORIENTED_EDGE('',*,*,#1519,.T.);
#2078=ORIENTED_EDGE('',*,*,#1517,.T.);
#2079=ORIENTED_EDGE('',*,*,#1515,.T.);
#2080=ORIENTED_EDGE('',*,*,#1513,.T.);
#2081=ORIENTED_EDGE('',*,*,#1511,.T.);
#2082=ORIENTED_EDGE('',*,*,#1509,.T.);
#2083=ORIENTED_EDGE('',*,*,#1497,.T.);
#2084=ORIENTED_EDGE('',*,*,#1499,.T.);
#2085=ORIENTED_EDGE('',*,*,#1478,.T.);
#2086=ORIENTED_EDGE('',*,*,#1500,.T.);
#2087=ORIENTED_EDGE('',*,*,#1462,.T.);
#2088=ORIENTED_EDGE('',*,*,#1520,.F.);
#2089=ORIENTED_EDGE('',*,*,#1521,.T.);
#2090=ORIENTED_EDGE('',*,*,#1522,.T.);
#2091=ORIENTED_EDGE('',*,*,#1521,.F.);
#2092=ORIENTED_EDGE('',*,*,#1522,.F.);
#2093=ORIENTED_EDGE('',*,*,#1523,.T.);
#2094=ORIENTED_EDGE('',*,*,#1524,.T.);
#2095=ORIENTED_EDGE('',*,*,#1525,.T.);
#2096=ORIENTED_EDGE('',*,*,#1526,.T.);
#2097=ORIENTED_EDGE('',*,*,#1524,.F.);
#2098=ORIENTED_EDGE('',*,*,#1523,.F.);
#2099=ORIENTED_EDGE('',*,*,#1520,.T.);
#2100=ORIENTED_EDGE('',*,*,#1526,.F.);
#2101=ORIENTED_EDGE('',*,*,#1527,.T.);
#2102=ORIENTED_EDGE('',*,*,#1528,.T.);
#2103=ORIENTED_EDGE('',*,*,#1529,.T.);
#2104=ORIENTED_EDGE('',*,*,#1527,.F.);
#2105=ORIENTED_EDGE('',*,*,#1525,.F.);
#2106=ORIENTED_EDGE('',*,*,#1530,.T.);
#2107=ORIENTED_EDGE('',*,*,#1531,.T.);
#2108=ORIENTED_EDGE('',*,*,#1532,.F.);
#2109=ORIENTED_EDGE('',*,*,#1531,.F.);
#2110=ORIENTED_EDGE('',*,*,#1530,.F.);
#2111=ORIENTED_EDGE('',*,*,#1529,.F.);
#2112=ORIENTED_EDGE('',*,*,#1533,.T.);
#2113=ORIENTED_EDGE('',*,*,#1533,.F.);
#2114=ORIENTED_EDGE('',*,*,#1528,.F.);
#2115=ORIENTED_EDGE('',*,*,#1532,.T.);
#2116=ORIENTED_EDGE('',*,*,#1534,.F.);
#2117=ORIENTED_EDGE('',*,*,#1534,.T.);
#2118=ORIENTED_EDGE('',*,*,#1535,.T.);
#2119=ORIENTED_EDGE('',*,*,#1536,.T.);
#2120=ORIENTED_EDGE('',*,*,#1535,.F.);
#2121=ORIENTED_EDGE('',*,*,#1536,.F.);
#2122=ORIENTED_EDGE('',*,*,#1537,.T.);
#2123=ORIENTED_EDGE('',*,*,#1537,.F.);
#2124=ORIENTED_EDGE('',*,*,#1538,.T.);
#2125=ORIENTED_EDGE('',*,*,#1539,.T.);
#2126=ORIENTED_EDGE('',*,*,#1538,.F.);
#2127=ORIENTED_EDGE('',*,*,#1539,.F.);
#2128=ORIENTED_EDGE('',*,*,#1540,.F.);
#2129=ORIENTED_EDGE('',*,*,#1541,.F.);
#2130=ORIENTED_EDGE('',*,*,#1542,.F.);
#2131=ORIENTED_EDGE('',*,*,#1543,.T.);
#2132=ORIENTED_EDGE('',*,*,#1544,.F.);
#2133=ORIENTED_EDGE('',*,*,#1545,.F.);
#2134=ORIENTED_EDGE('',*,*,#1540,.T.);
#2135=ORIENTED_EDGE('',*,*,#1546,.T.);
#2136=ORIENTED_EDGE('',*,*,#1547,.T.);
#2137=ORIENTED_EDGE('',*,*,#1548,.F.);
#2138=ORIENTED_EDGE('',*,*,#1549,.F.);
#2139=ORIENTED_EDGE('',*,*,#1550,.F.);
#2140=ORIENTED_EDGE('',*,*,#1544,.T.);
#2141=ORIENTED_EDGE('',*,*,#1551,.T.);
#2142=ORIENTED_EDGE('',*,*,#1552,.F.);
#2143=ORIENTED_EDGE('',*,*,#1553,.F.);
#2144=ORIENTED_EDGE('',*,*,#1548,.T.);
#2145=ORIENTED_EDGE('',*,*,#1554,.T.);
#2146=ORIENTED_EDGE('',*,*,#1555,.T.);
#2147=ORIENTED_EDGE('',*,*,#1556,.F.);
#2148=ORIENTED_EDGE('',*,*,#1557,.F.);
#2149=ORIENTED_EDGE('',*,*,#1558,.F.);
#2150=ORIENTED_EDGE('',*,*,#1552,.T.);
#2151=ORIENTED_EDGE('',*,*,#1559,.T.);
#2152=ORIENTED_EDGE('',*,*,#1560,.F.);
#2153=ORIENTED_EDGE('',*,*,#1561,.F.);
#2154=ORIENTED_EDGE('',*,*,#1556,.T.);
#2155=ORIENTED_EDGE('',*,*,#1562,.T.);
#2156=ORIENTED_EDGE('',*,*,#1563,.T.);
#2157=ORIENTED_EDGE('',*,*,#1564,.F.);
#2158=ORIENTED_EDGE('',*,*,#1565,.F.);
#2159=ORIENTED_EDGE('',*,*,#1566,.F.);
#2160=ORIENTED_EDGE('',*,*,#1560,.T.);
#2161=ORIENTED_EDGE('',*,*,#1567,.T.);
#2162=ORIENTED_EDGE('',*,*,#1568,.F.);
#2163=ORIENTED_EDGE('',*,*,#1569,.F.);
#2164=ORIENTED_EDGE('',*,*,#1564,.T.);
#2165=ORIENTED_EDGE('',*,*,#1570,.T.);
#2166=ORIENTED_EDGE('',*,*,#1571,.T.);
#2167=ORIENTED_EDGE('',*,*,#1572,.F.);
#2168=ORIENTED_EDGE('',*,*,#1573,.F.);
#2169=ORIENTED_EDGE('',*,*,#1574,.F.);
#2170=ORIENTED_EDGE('',*,*,#1568,.T.);
#2171=ORIENTED_EDGE('',*,*,#1575,.T.);
#2172=ORIENTED_EDGE('',*,*,#1576,.F.);
#2173=ORIENTED_EDGE('',*,*,#1577,.F.);
#2174=ORIENTED_EDGE('',*,*,#1572,.T.);
#2175=ORIENTED_EDGE('',*,*,#1578,.T.);
#2176=ORIENTED_EDGE('',*,*,#1579,.T.);
#2177=ORIENTED_EDGE('',*,*,#1580,.F.);
#2178=ORIENTED_EDGE('',*,*,#1581,.F.);
#2179=ORIENTED_EDGE('',*,*,#1582,.F.);
#2180=ORIENTED_EDGE('',*,*,#1576,.T.);
#2181=ORIENTED_EDGE('',*,*,#1583,.T.);
#2182=ORIENTED_EDGE('',*,*,#1584,.F.);
#2183=ORIENTED_EDGE('',*,*,#1585,.F.);
#2184=ORIENTED_EDGE('',*,*,#1580,.T.);
#2185=ORIENTED_EDGE('',*,*,#1586,.T.);
#2186=ORIENTED_EDGE('',*,*,#1587,.T.);
#2187=ORIENTED_EDGE('',*,*,#1588,.F.);
#2188=ORIENTED_EDGE('',*,*,#1589,.F.);
#2189=ORIENTED_EDGE('',*,*,#1590,.F.);
#2190=ORIENTED_EDGE('',*,*,#1584,.T.);
#2191=ORIENTED_EDGE('',*,*,#1591,.T.);
#2192=ORIENTED_EDGE('',*,*,#1592,.F.);
#2193=ORIENTED_EDGE('',*,*,#1593,.F.);
#2194=ORIENTED_EDGE('',*,*,#1588,.T.);
#2195=ORIENTED_EDGE('',*,*,#1594,.T.);
#2196=ORIENTED_EDGE('',*,*,#1595,.T.);
#2197=ORIENTED_EDGE('',*,*,#1596,.F.);
#2198=ORIENTED_EDGE('',*,*,#1597,.F.);
#2199=ORIENTED_EDGE('',*,*,#1598,.F.);
#2200=ORIENTED_EDGE('',*,*,#1592,.T.);
#2201=ORIENTED_EDGE('',*,*,#1599,.T.);
#2202=ORIENTED_EDGE('',*,*,#1600,.F.);
#2203=ORIENTED_EDGE('',*,*,#1601,.F.);
#2204=ORIENTED_EDGE('',*,*,#1596,.T.);
#2205=ORIENTED_EDGE('',*,*,#1602,.T.);
#2206=ORIENTED_EDGE('',*,*,#1603,.T.);
#2207=ORIENTED_EDGE('',*,*,#1604,.F.);
#2208=ORIENTED_EDGE('',*,*,#1605,.F.);
#2209=ORIENTED_EDGE('',*,*,#1606,.F.);
#2210=ORIENTED_EDGE('',*,*,#1600,.T.);
#2211=ORIENTED_EDGE('',*,*,#1607,.T.);
#2212=ORIENTED_EDGE('',*,*,#1608,.F.);
#2213=ORIENTED_EDGE('',*,*,#1609,.F.);
#2214=ORIENTED_EDGE('',*,*,#1604,.T.);
#2215=ORIENTED_EDGE('',*,*,#1610,.T.);
#2216=ORIENTED_EDGE('',*,*,#1611,.T.);
#2217=ORIENTED_EDGE('',*,*,#1612,.F.);
#2218=ORIENTED_EDGE('',*,*,#1613,.F.);
#2219=ORIENTED_EDGE('',*,*,#1614,.F.);
#2220=ORIENTED_EDGE('',*,*,#1608,.T.);
#2221=ORIENTED_EDGE('',*,*,#1615,.T.);
#2222=ORIENTED_EDGE('',*,*,#1616,.F.);
#2223=ORIENTED_EDGE('',*,*,#1617,.F.);
#2224=ORIENTED_EDGE('',*,*,#1612,.T.);
#2225=ORIENTED_EDGE('',*,*,#1618,.T.);
#2226=ORIENTED_EDGE('',*,*,#1619,.T.);
#2227=ORIENTED_EDGE('',*,*,#1620,.F.);
#2228=ORIENTED_EDGE('',*,*,#1621,.F.);
#2229=ORIENTED_EDGE('',*,*,#1622,.F.);
#2230=ORIENTED_EDGE('',*,*,#1616,.T.);
#2231=ORIENTED_EDGE('',*,*,#1623,.T.);
#2232=ORIENTED_EDGE('',*,*,#1624,.T.);
#2233=ORIENTED_EDGE('',*,*,#1625,.F.);
#2234=ORIENTED_EDGE('',*,*,#1626,.T.);
#2235=ORIENTED_EDGE('',*,*,#1627,.F.);
#2236=ORIENTED_EDGE('',*,*,#1628,.T.);
#2237=ORIENTED_EDGE('',*,*,#1629,.F.);
#2238=ORIENTED_EDGE('',*,*,#1630,.T.);
#2239=ORIENTED_EDGE('',*,*,#1625,.T.);
#2240=ORIENTED_EDGE('',*,*,#1631,.T.);
#2241=ORIENTED_EDGE('',*,*,#1632,.F.);
#2242=ORIENTED_EDGE('',*,*,#1633,.T.);
#2243=ORIENTED_EDGE('',*,*,#1629,.T.);
#2244=ORIENTED_EDGE('',*,*,#1634,.T.);
#2245=ORIENTED_EDGE('',*,*,#1635,.F.);
#2246=ORIENTED_EDGE('',*,*,#1636,.T.);
#2247=ORIENTED_EDGE('',*,*,#1632,.T.);
#2248=ORIENTED_EDGE('',*,*,#1637,.T.);
#2249=ORIENTED_EDGE('',*,*,#1638,.F.);
#2250=ORIENTED_EDGE('',*,*,#1639,.T.);
#2251=ORIENTED_EDGE('',*,*,#1635,.T.);
#2252=ORIENTED_EDGE('',*,*,#1640,.T.);
#2253=ORIENTED_EDGE('',*,*,#1641,.F.);
#2254=ORIENTED_EDGE('',*,*,#1642,.T.);
#2255=ORIENTED_EDGE('',*,*,#1638,.T.);
#2256=ORIENTED_EDGE('',*,*,#1643,.T.);
#2257=ORIENTED_EDGE('',*,*,#1644,.F.);
#2258=ORIENTED_EDGE('',*,*,#1645,.T.);
#2259=ORIENTED_EDGE('',*,*,#1641,.T.);
#2260=ORIENTED_EDGE('',*,*,#1646,.T.);
#2261=ORIENTED_EDGE('',*,*,#1647,.F.);
#2262=ORIENTED_EDGE('',*,*,#1648,.T.);
#2263=ORIENTED_EDGE('',*,*,#1644,.T.);
#2264=ORIENTED_EDGE('',*,*,#1649,.T.);
#2265=ORIENTED_EDGE('',*,*,#1650,.F.);
#2266=ORIENTED_EDGE('',*,*,#1651,.T.);
#2267=ORIENTED_EDGE('',*,*,#1647,.T.);
#2268=ORIENTED_EDGE('',*,*,#1652,.T.);
#2269=ORIENTED_EDGE('',*,*,#1653,.F.);
#2270=ORIENTED_EDGE('',*,*,#1654,.T.);
#2271=ORIENTED_EDGE('',*,*,#1650,.T.);
#2272=ORIENTED_EDGE('',*,*,#1655,.T.);
#2273=ORIENTED_EDGE('',*,*,#1656,.F.);
#2274=ORIENTED_EDGE('',*,*,#1657,.T.);
#2275=ORIENTED_EDGE('',*,*,#1653,.T.);
#2276=ORIENTED_EDGE('',*,*,#1658,.T.);
#2277=ORIENTED_EDGE('',*,*,#1659,.F.);
#2278=ORIENTED_EDGE('',*,*,#1660,.T.);
#2279=ORIENTED_EDGE('',*,*,#1656,.T.);
#2280=ORIENTED_EDGE('',*,*,#1661,.T.);
#2281=ORIENTED_EDGE('',*,*,#1662,.F.);
#2282=ORIENTED_EDGE('',*,*,#1663,.T.);
#2283=ORIENTED_EDGE('',*,*,#1659,.T.);
#2284=ORIENTED_EDGE('',*,*,#1664,.T.);
#2285=ORIENTED_EDGE('',*,*,#1665,.F.);
#2286=ORIENTED_EDGE('',*,*,#1666,.T.);
#2287=ORIENTED_EDGE('',*,*,#1662,.T.);
#2288=ORIENTED_EDGE('',*,*,#1667,.T.);
#2289=ORIENTED_EDGE('',*,*,#1668,.F.);
#2290=ORIENTED_EDGE('',*,*,#1669,.T.);
#2291=ORIENTED_EDGE('',*,*,#1665,.T.);
#2292=ORIENTED_EDGE('',*,*,#1670,.T.);
#2293=ORIENTED_EDGE('',*,*,#1671,.F.);
#2294=ORIENTED_EDGE('',*,*,#1672,.T.);
#2295=ORIENTED_EDGE('',*,*,#1668,.T.);
#2296=ORIENTED_EDGE('',*,*,#1673,.T.);
#2297=ORIENTED_EDGE('',*,*,#1674,.F.);
#2298=ORIENTED_EDGE('',*,*,#1675,.T.);
#2299=ORIENTED_EDGE('',*,*,#1671,.T.);
#2300=ORIENTED_EDGE('',*,*,#1676,.T.);
#2301=ORIENTED_EDGE('',*,*,#1677,.F.);
#2302=ORIENTED_EDGE('',*,*,#1678,.T.);
#2303=ORIENTED_EDGE('',*,*,#1674,.T.);
#2304=ORIENTED_EDGE('',*,*,#1679,.T.);
#2305=ORIENTED_EDGE('',*,*,#1680,.F.);
#2306=ORIENTED_EDGE('',*,*,#1681,.T.);
#2307=ORIENTED_EDGE('',*,*,#1677,.T.);
#2308=ORIENTED_EDGE('',*,*,#1682,.T.);
#2309=ORIENTED_EDGE('',*,*,#1683,.F.);
#2310=ORIENTED_EDGE('',*,*,#1684,.T.);
#2311=ORIENTED_EDGE('',*,*,#1680,.T.);
#2312=ORIENTED_EDGE('',*,*,#1685,.T.);
#2313=ORIENTED_EDGE('',*,*,#1686,.F.);
#2314=ORIENTED_EDGE('',*,*,#1687,.T.);
#2315=ORIENTED_EDGE('',*,*,#1683,.T.);
#2316=ORIENTED_EDGE('',*,*,#1688,.T.);
#2317=ORIENTED_EDGE('',*,*,#1686,.T.);
#2318=ORIENTED_EDGE('',*,*,#1689,.T.);
#2319=ORIENTED_EDGE('',*,*,#1690,.F.);
#2320=ORIENTED_EDGE('',*,*,#1691,.T.);
#2321=ORIENTED_EDGE('',*,*,#1620,.T.);
#2322=ORIENTED_EDGE('',*,*,#1692,.T.);
#2323=ORIENTED_EDGE('',*,*,#1693,.F.);
#2324=ORIENTED_EDGE('',*,*,#1694,.F.);
#2325=ORIENTED_EDGE('',*,*,#1695,.F.);
#2326=ORIENTED_EDGE('',*,*,#1696,.F.);
#2327=ORIENTED_EDGE('',*,*,#1689,.F.);
#2328=ORIENTED_EDGE('',*,*,#1688,.F.);
#2329=ORIENTED_EDGE('',*,*,#1685,.F.);
#2330=ORIENTED_EDGE('',*,*,#1682,.F.);
#2331=ORIENTED_EDGE('',*,*,#1679,.F.);
#2332=ORIENTED_EDGE('',*,*,#1676,.F.);
#2333=ORIENTED_EDGE('',*,*,#1673,.F.);
#2334=ORIENTED_EDGE('',*,*,#1670,.F.);
#2335=ORIENTED_EDGE('',*,*,#1667,.F.);
#2336=ORIENTED_EDGE('',*,*,#1664,.F.);
#2337=ORIENTED_EDGE('',*,*,#1661,.F.);
#2338=ORIENTED_EDGE('',*,*,#1658,.F.);
#2339=ORIENTED_EDGE('',*,*,#1655,.F.);
#2340=ORIENTED_EDGE('',*,*,#1652,.F.);
#2341=ORIENTED_EDGE('',*,*,#1649,.F.);
#2342=ORIENTED_EDGE('',*,*,#1646,.F.);
#2343=ORIENTED_EDGE('',*,*,#1643,.F.);
#2344=ORIENTED_EDGE('',*,*,#1640,.F.);
#2345=ORIENTED_EDGE('',*,*,#1637,.F.);
#2346=ORIENTED_EDGE('',*,*,#1634,.F.);
#2347=ORIENTED_EDGE('',*,*,#1631,.F.);
#2348=ORIENTED_EDGE('',*,*,#1628,.F.);
#2349=ORIENTED_EDGE('',*,*,#1697,.F.);
#2350=ORIENTED_EDGE('',*,*,#1698,.T.);
#2351=ORIENTED_EDGE('',*,*,#1541,.T.);
#2352=ORIENTED_EDGE('',*,*,#1545,.T.);
#2353=ORIENTED_EDGE('',*,*,#1550,.T.);
#2354=ORIENTED_EDGE('',*,*,#1549,.T.);
#2355=ORIENTED_EDGE('',*,*,#1553,.T.);
#2356=ORIENTED_EDGE('',*,*,#1558,.T.);
#2357=ORIENTED_EDGE('',*,*,#1557,.T.);
#2358=ORIENTED_EDGE('',*,*,#1561,.T.);
#2359=ORIENTED_EDGE('',*,*,#1566,.T.);
#2360=ORIENTED_EDGE('',*,*,#1565,.T.);
#2361=ORIENTED_EDGE('',*,*,#1569,.T.);
#2362=ORIENTED_EDGE('',*,*,#1574,.T.);
#2363=ORIENTED_EDGE('',*,*,#1573,.T.);
#2364=ORIENTED_EDGE('',*,*,#1577,.T.);
#2365=ORIENTED_EDGE('',*,*,#1582,.T.);
#2366=ORIENTED_EDGE('',*,*,#1581,.T.);
#2367=ORIENTED_EDGE('',*,*,#1585,.T.);
#2368=ORIENTED_EDGE('',*,*,#1590,.T.);
#2369=ORIENTED_EDGE('',*,*,#1589,.T.);
#2370=ORIENTED_EDGE('',*,*,#1593,.T.);
#2371=ORIENTED_EDGE('',*,*,#1598,.T.);
#2372=ORIENTED_EDGE('',*,*,#1597,.T.);
#2373=ORIENTED_EDGE('',*,*,#1601,.T.);
#2374=ORIENTED_EDGE('',*,*,#1606,.T.);
#2375=ORIENTED_EDGE('',*,*,#1605,.T.);
#2376=ORIENTED_EDGE('',*,*,#1609,.T.);
#2377=ORIENTED_EDGE('',*,*,#1614,.T.);
#2378=ORIENTED_EDGE('',*,*,#1613,.T.);
#2379=ORIENTED_EDGE('',*,*,#1617,.T.);
#2380=ORIENTED_EDGE('',*,*,#1622,.T.);
#2381=ORIENTED_EDGE('',*,*,#1621,.T.);
#2382=ORIENTED_EDGE('',*,*,#1695,.T.);
#2383=ORIENTED_EDGE('',*,*,#1694,.T.);
#2384=ORIENTED_EDGE('',*,*,#1699,.F.);
#2385=ORIENTED_EDGE('',*,*,#1700,.F.);
#2386=ORIENTED_EDGE('',*,*,#1692,.F.);
#2387=ORIENTED_EDGE('',*,*,#1624,.F.);
#2388=ORIENTED_EDGE('',*,*,#1623,.F.);
#2389=ORIENTED_EDGE('',*,*,#1619,.F.);
#2390=ORIENTED_EDGE('',*,*,#1618,.F.);
#2391=ORIENTED_EDGE('',*,*,#1615,.F.);
#2392=ORIENTED_EDGE('',*,*,#1611,.F.);
#2393=ORIENTED_EDGE('',*,*,#1610,.F.);
#2394=ORIENTED_EDGE('',*,*,#1607,.F.);
#2395=ORIENTED_EDGE('',*,*,#1603,.F.);
#2396=ORIENTED_EDGE('',*,*,#1602,.F.);
#2397=ORIENTED_EDGE('',*,*,#1599,.F.);
#2398=ORIENTED_EDGE('',*,*,#1595,.F.);
#2399=ORIENTED_EDGE('',*,*,#1594,.F.);
#2400=ORIENTED_EDGE('',*,*,#1591,.F.);
#2401=ORIENTED_EDGE('',*,*,#1587,.F.);
#2402=ORIENTED_EDGE('',*,*,#1586,.F.);
#2403=ORIENTED_EDGE('',*,*,#1583,.F.);
#2404=ORIENTED_EDGE('',*,*,#1579,.F.);
#2405=ORIENTED_EDGE('',*,*,#1578,.F.);
#2406=ORIENTED_EDGE('',*,*,#1575,.F.);
#2407=ORIENTED_EDGE('',*,*,#1571,.F.);
#2408=ORIENTED_EDGE('',*,*,#1570,.F.);
#2409=ORIENTED_EDGE('',*,*,#1567,.F.);
#2410=ORIENTED_EDGE('',*,*,#1563,.F.);
#2411=ORIENTED_EDGE('',*,*,#1562,.F.);
#2412=ORIENTED_EDGE('',*,*,#1559,.F.);
#2413=ORIENTED_EDGE('',*,*,#1555,.F.);
#2414=ORIENTED_EDGE('',*,*,#1554,.F.);
#2415=ORIENTED_EDGE('',*,*,#1551,.F.);
#2416=ORIENTED_EDGE('',*,*,#1547,.F.);
#2417=ORIENTED_EDGE('',*,*,#1546,.F.);
#2418=ORIENTED_EDGE('',*,*,#1543,.F.);
#2419=ORIENTED_EDGE('',*,*,#1701,.F.);
#2420=ORIENTED_EDGE('',*,*,#1626,.F.);
#2421=ORIENTED_EDGE('',*,*,#1630,.F.);
#2422=ORIENTED_EDGE('',*,*,#1633,.F.);
#2423=ORIENTED_EDGE('',*,*,#1636,.F.);
#2424=ORIENTED_EDGE('',*,*,#1639,.F.);
#2425=ORIENTED_EDGE('',*,*,#1642,.F.);
#2426=ORIENTED_EDGE('',*,*,#1645,.F.);
#2427=ORIENTED_EDGE('',*,*,#1648,.F.);
#2428=ORIENTED_EDGE('',*,*,#1651,.F.);
#2429=ORIENTED_EDGE('',*,*,#1654,.F.);
#2430=ORIENTED_EDGE('',*,*,#1657,.F.);
#2431=ORIENTED_EDGE('',*,*,#1660,.F.);
#2432=ORIENTED_EDGE('',*,*,#1663,.F.);
#2433=ORIENTED_EDGE('',*,*,#1666,.F.);
#2434=ORIENTED_EDGE('',*,*,#1669,.F.);
#2435=ORIENTED_EDGE('',*,*,#1672,.F.);
#2436=ORIENTED_EDGE('',*,*,#1675,.F.);
#2437=ORIENTED_EDGE('',*,*,#1678,.F.);
#2438=ORIENTED_EDGE('',*,*,#1681,.F.);
#2439=ORIENTED_EDGE('',*,*,#1684,.F.);
#2440=ORIENTED_EDGE('',*,*,#1687,.F.);
#2441=ORIENTED_EDGE('',*,*,#1691,.F.);
#2442=ORIENTED_EDGE('',*,*,#1696,.T.);
#2443=ORIENTED_EDGE('',*,*,#1693,.T.);
#2444=ORIENTED_EDGE('',*,*,#1700,.T.);
#2445=ORIENTED_EDGE('',*,*,#1699,.T.);
#2446=ORIENTED_EDGE('',*,*,#1690,.T.);
#2447=ORIENTED_EDGE('',*,*,#1697,.T.);
#2448=ORIENTED_EDGE('',*,*,#1627,.T.);
#2449=ORIENTED_EDGE('',*,*,#1701,.T.);
#2450=ORIENTED_EDGE('',*,*,#1542,.T.);
#2451=ORIENTED_EDGE('',*,*,#1698,.F.);
#2452=ORIENTED_EDGE('',*,*,#1702,.T.);
#2453=ORIENTED_EDGE('',*,*,#1703,.T.);
#2454=ORIENTED_EDGE('',*,*,#1704,.F.);
#2455=ORIENTED_EDGE('',*,*,#1705,.F.);
#2456=ORIENTED_EDGE('',*,*,#1706,.T.);
#2457=ORIENTED_EDGE('',*,*,#1707,.T.);
#2458=ORIENTED_EDGE('',*,*,#1708,.T.);
#2459=ORIENTED_EDGE('',*,*,#1702,.F.);
#2460=ORIENTED_EDGE('',*,*,#1709,.F.);
#2461=ORIENTED_EDGE('',*,*,#1710,.F.);
#2462=ORIENTED_EDGE('',*,*,#1711,.F.);
#2463=ORIENTED_EDGE('',*,*,#1712,.F.);
#2464=ORIENTED_EDGE('',*,*,#1713,.F.);
#2465=ORIENTED_EDGE('',*,*,#1714,.F.);
#2466=ORIENTED_EDGE('',*,*,#1715,.T.);
#2467=ORIENTED_EDGE('',*,*,#1716,.T.);
#2468=ORIENTED_EDGE('',*,*,#1717,.T.);
#2469=ORIENTED_EDGE('',*,*,#1718,.T.);
#2470=ORIENTED_EDGE('',*,*,#1719,.T.);
#2471=ORIENTED_EDGE('',*,*,#1720,.F.);
#2472=ORIENTED_EDGE('',*,*,#1721,.T.);
#2473=ORIENTED_EDGE('',*,*,#1722,.T.);
#2474=ORIENTED_EDGE('',*,*,#1723,.T.);
#2475=ORIENTED_EDGE('',*,*,#1724,.T.);
#2476=ORIENTED_EDGE('',*,*,#1717,.F.);
#2477=ORIENTED_EDGE('',*,*,#1725,.T.);
#2478=ORIENTED_EDGE('',*,*,#1726,.F.);
#2479=ORIENTED_EDGE('',*,*,#1727,.T.);
#2480=ORIENTED_EDGE('',*,*,#1728,.F.);
#2481=ORIENTED_EDGE('',*,*,#1729,.T.);
#2482=ORIENTED_EDGE('',*,*,#1726,.T.);
#2483=ORIENTED_EDGE('',*,*,#1730,.T.);
#2484=ORIENTED_EDGE('',*,*,#1731,.T.);
#2485=ORIENTED_EDGE('',*,*,#1722,.F.);
#2486=ORIENTED_EDGE('',*,*,#1732,.T.);
#2487=ORIENTED_EDGE('',*,*,#1711,.T.);
#2488=ORIENTED_EDGE('',*,*,#1733,.T.);
#2489=ORIENTED_EDGE('',*,*,#1734,.T.);
#2490=ORIENTED_EDGE('',*,*,#1706,.F.);
#2491=ORIENTED_EDGE('',*,*,#1735,.F.);
#2492=ORIENTED_EDGE('',*,*,#1736,.F.);
#2493=ORIENTED_EDGE('',*,*,#1737,.F.);
#2494=ORIENTED_EDGE('',*,*,#1703,.F.);
#2495=ORIENTED_EDGE('',*,*,#1708,.F.);
#2496=ORIENTED_EDGE('',*,*,#1707,.F.);
#2497=ORIENTED_EDGE('',*,*,#1734,.F.);
#2498=ORIENTED_EDGE('',*,*,#1733,.F.);
#2499=ORIENTED_EDGE('',*,*,#1716,.F.);
#2500=ORIENTED_EDGE('',*,*,#1715,.F.);
#2501=ORIENTED_EDGE('',*,*,#1738,.F.);
#2502=ORIENTED_EDGE('',*,*,#1727,.F.);
#2503=ORIENTED_EDGE('',*,*,#1732,.F.);
#2504=ORIENTED_EDGE('',*,*,#1725,.F.);
#2505=ORIENTED_EDGE('',*,*,#1721,.F.);
#2506=ORIENTED_EDGE('',*,*,#1739,.F.);
#2507=ORIENTED_EDGE('',*,*,#1740,.F.);
#2508=ORIENTED_EDGE('',*,*,#1719,.F.);
#2509=ORIENTED_EDGE('',*,*,#1718,.F.);
#2510=ORIENTED_EDGE('',*,*,#1724,.F.);
#2511=ORIENTED_EDGE('',*,*,#1723,.F.);
#2512=ORIENTED_EDGE('',*,*,#1731,.F.);
#2513=ORIENTED_EDGE('',*,*,#1730,.F.);
#2514=ORIENTED_EDGE('',*,*,#1729,.F.);
#2515=ORIENTED_EDGE('',*,*,#1741,.F.);
#2516=ORIENTED_EDGE('',*,*,#1713,.T.);
#2517=ORIENTED_EDGE('',*,*,#1712,.T.);
#2518=ORIENTED_EDGE('',*,*,#1736,.T.);
#2519=ORIENTED_EDGE('',*,*,#1735,.T.);
#2520=ORIENTED_EDGE('',*,*,#1710,.T.);
#2521=ORIENTED_EDGE('',*,*,#1709,.T.);
#2522=ORIENTED_EDGE('',*,*,#1705,.T.);
#2523=ORIENTED_EDGE('',*,*,#1742,.T.);
#2524=ORIENTED_EDGE('',*,*,#1743,.T.);
#2525=ORIENTED_EDGE('',*,*,#1744,.T.);
#2526=ORIENTED_EDGE('',*,*,#1745,.T.);
#2527=ORIENTED_EDGE('',*,*,#1746,.T.);
#2528=ORIENTED_EDGE('',*,*,#1747,.T.);
#2529=ORIENTED_EDGE('',*,*,#1738,.T.);
#2530=ORIENTED_EDGE('',*,*,#1714,.T.);
#2531=ORIENTED_EDGE('',*,*,#1741,.T.);
#2532=ORIENTED_EDGE('',*,*,#1728,.T.);
#2533=ORIENTED_EDGE('',*,*,#1743,.F.);
#2534=ORIENTED_EDGE('',*,*,#1748,.T.);
#2535=ORIENTED_EDGE('',*,*,#1749,.F.);
#2536=ORIENTED_EDGE('',*,*,#1750,.F.);
#2537=ORIENTED_EDGE('',*,*,#1744,.F.);
#2538=ORIENTED_EDGE('',*,*,#1750,.T.);
#2539=ORIENTED_EDGE('',*,*,#1751,.F.);
#2540=ORIENTED_EDGE('',*,*,#1752,.F.);
#2541=ORIENTED_EDGE('',*,*,#1745,.F.);
#2542=ORIENTED_EDGE('',*,*,#1752,.T.);
#2543=ORIENTED_EDGE('',*,*,#1753,.F.);
#2544=ORIENTED_EDGE('',*,*,#1754,.F.);
#2545=ORIENTED_EDGE('',*,*,#1746,.F.);
#2546=ORIENTED_EDGE('',*,*,#1754,.T.);
#2547=ORIENTED_EDGE('',*,*,#1755,.F.);
#2548=ORIENTED_EDGE('',*,*,#1756,.F.);
#2549=ORIENTED_EDGE('',*,*,#1747,.F.);
#2550=ORIENTED_EDGE('',*,*,#1756,.T.);
#2551=ORIENTED_EDGE('',*,*,#1757,.F.);
#2552=ORIENTED_EDGE('',*,*,#1758,.F.);
#2553=ORIENTED_EDGE('',*,*,#1742,.F.);
#2554=ORIENTED_EDGE('',*,*,#1758,.T.);
#2555=ORIENTED_EDGE('',*,*,#1759,.F.);
#2556=ORIENTED_EDGE('',*,*,#1748,.F.);
#2557=ORIENTED_EDGE('',*,*,#1759,.T.);
#2558=ORIENTED_EDGE('',*,*,#1757,.T.);
#2559=ORIENTED_EDGE('',*,*,#1755,.T.);
#2560=ORIENTED_EDGE('',*,*,#1753,.T.);
#2561=ORIENTED_EDGE('',*,*,#1751,.T.);
#2562=ORIENTED_EDGE('',*,*,#1749,.T.);
#2563=ORIENTED_EDGE('',*,*,#1737,.T.);
#2564=ORIENTED_EDGE('',*,*,#1739,.T.);
#2565=ORIENTED_EDGE('',*,*,#1720,.T.);
#2566=ORIENTED_EDGE('',*,*,#1740,.T.);
#2567=ORIENTED_EDGE('',*,*,#1704,.T.);
#2568=ORIENTED_EDGE('',*,*,#1760,.F.);
#2569=ORIENTED_EDGE('',*,*,#1761,.F.);
#2570=ORIENTED_EDGE('',*,*,#1762,.F.);
#2571=ORIENTED_EDGE('',*,*,#1763,.T.);
#2572=ORIENTED_EDGE('',*,*,#1764,.F.);
#2573=ORIENTED_EDGE('',*,*,#1765,.F.);
#2574=ORIENTED_EDGE('',*,*,#1760,.T.);
#2575=ORIENTED_EDGE('',*,*,#1766,.T.);
#2576=ORIENTED_EDGE('',*,*,#1767,.T.);
#2577=ORIENTED_EDGE('',*,*,#1768,.F.);
#2578=ORIENTED_EDGE('',*,*,#1769,.F.);
#2579=ORIENTED_EDGE('',*,*,#1770,.F.);
#2580=ORIENTED_EDGE('',*,*,#1764,.T.);
#2581=ORIENTED_EDGE('',*,*,#1771,.T.);
#2582=ORIENTED_EDGE('',*,*,#1772,.F.);
#2583=ORIENTED_EDGE('',*,*,#1773,.F.);
#2584=ORIENTED_EDGE('',*,*,#1768,.T.);
#2585=ORIENTED_EDGE('',*,*,#1774,.T.);
#2586=ORIENTED_EDGE('',*,*,#1775,.T.);
#2587=ORIENTED_EDGE('',*,*,#1776,.F.);
#2588=ORIENTED_EDGE('',*,*,#1777,.F.);
#2589=ORIENTED_EDGE('',*,*,#1778,.F.);
#2590=ORIENTED_EDGE('',*,*,#1772,.T.);
#2591=ORIENTED_EDGE('',*,*,#1779,.T.);
#2592=ORIENTED_EDGE('',*,*,#1780,.F.);
#2593=ORIENTED_EDGE('',*,*,#1781,.F.);
#2594=ORIENTED_EDGE('',*,*,#1776,.T.);
#2595=ORIENTED_EDGE('',*,*,#1782,.T.);
#2596=ORIENTED_EDGE('',*,*,#1783,.T.);
#2597=ORIENTED_EDGE('',*,*,#1784,.F.);
#2598=ORIENTED_EDGE('',*,*,#1785,.F.);
#2599=ORIENTED_EDGE('',*,*,#1786,.F.);
#2600=ORIENTED_EDGE('',*,*,#1780,.T.);
#2601=ORIENTED_EDGE('',*,*,#1787,.T.);
#2602=ORIENTED_EDGE('',*,*,#1788,.F.);
#2603=ORIENTED_EDGE('',*,*,#1789,.F.);
#2604=ORIENTED_EDGE('',*,*,#1784,.T.);
#2605=ORIENTED_EDGE('',*,*,#1790,.T.);
#2606=ORIENTED_EDGE('',*,*,#1791,.T.);
#2607=ORIENTED_EDGE('',*,*,#1792,.F.);
#2608=ORIENTED_EDGE('',*,*,#1793,.F.);
#2609=ORIENTED_EDGE('',*,*,#1794,.F.);
#2610=ORIENTED_EDGE('',*,*,#1788,.T.);
#2611=ORIENTED_EDGE('',*,*,#1795,.T.);
#2612=ORIENTED_EDGE('',*,*,#1796,.F.);
#2613=ORIENTED_EDGE('',*,*,#1797,.F.);
#2614=ORIENTED_EDGE('',*,*,#1792,.T.);
#2615=ORIENTED_EDGE('',*,*,#1798,.T.);
#2616=ORIENTED_EDGE('',*,*,#1799,.T.);
#2617=ORIENTED_EDGE('',*,*,#1800,.F.);
#2618=ORIENTED_EDGE('',*,*,#1801,.F.);
#2619=ORIENTED_EDGE('',*,*,#1802,.F.);
#2620=ORIENTED_EDGE('',*,*,#1796,.T.);
#2621=ORIENTED_EDGE('',*,*,#1803,.T.);
#2622=ORIENTED_EDGE('',*,*,#1804,.F.);
#2623=ORIENTED_EDGE('',*,*,#1805,.F.);
#2624=ORIENTED_EDGE('',*,*,#1800,.T.);
#2625=ORIENTED_EDGE('',*,*,#1806,.T.);
#2626=ORIENTED_EDGE('',*,*,#1807,.T.);
#2627=ORIENTED_EDGE('',*,*,#1808,.F.);
#2628=ORIENTED_EDGE('',*,*,#1809,.F.);
#2629=ORIENTED_EDGE('',*,*,#1810,.F.);
#2630=ORIENTED_EDGE('',*,*,#1804,.T.);
#2631=ORIENTED_EDGE('',*,*,#1811,.T.);
#2632=ORIENTED_EDGE('',*,*,#1812,.F.);
#2633=ORIENTED_EDGE('',*,*,#1813,.F.);
#2634=ORIENTED_EDGE('',*,*,#1808,.T.);
#2635=ORIENTED_EDGE('',*,*,#1814,.T.);
#2636=ORIENTED_EDGE('',*,*,#1815,.T.);
#2637=ORIENTED_EDGE('',*,*,#1816,.F.);
#2638=ORIENTED_EDGE('',*,*,#1817,.F.);
#2639=ORIENTED_EDGE('',*,*,#1818,.F.);
#2640=ORIENTED_EDGE('',*,*,#1812,.T.);
#2641=ORIENTED_EDGE('',*,*,#1819,.T.);
#2642=ORIENTED_EDGE('',*,*,#1820,.F.);
#2643=ORIENTED_EDGE('',*,*,#1821,.F.);
#2644=ORIENTED_EDGE('',*,*,#1816,.T.);
#2645=ORIENTED_EDGE('',*,*,#1822,.T.);
#2646=ORIENTED_EDGE('',*,*,#1823,.T.);
#2647=ORIENTED_EDGE('',*,*,#1824,.F.);
#2648=ORIENTED_EDGE('',*,*,#1825,.F.);
#2649=ORIENTED_EDGE('',*,*,#1826,.F.);
#2650=ORIENTED_EDGE('',*,*,#1820,.T.);
#2651=ORIENTED_EDGE('',*,*,#1827,.T.);
#2652=ORIENTED_EDGE('',*,*,#1828,.F.);
#2653=ORIENTED_EDGE('',*,*,#1829,.F.);
#2654=ORIENTED_EDGE('',*,*,#1824,.T.);
#2655=ORIENTED_EDGE('',*,*,#1830,.T.);
#2656=ORIENTED_EDGE('',*,*,#1831,.T.);
#2657=ORIENTED_EDGE('',*,*,#1832,.F.);
#2658=ORIENTED_EDGE('',*,*,#1833,.F.);
#2659=ORIENTED_EDGE('',*,*,#1834,.F.);
#2660=ORIENTED_EDGE('',*,*,#1828,.T.);
#2661=ORIENTED_EDGE('',*,*,#1835,.T.);
#2662=ORIENTED_EDGE('',*,*,#1836,.F.);
#2663=ORIENTED_EDGE('',*,*,#1837,.F.);
#2664=ORIENTED_EDGE('',*,*,#1832,.T.);
#2665=ORIENTED_EDGE('',*,*,#1838,.T.);
#2666=ORIENTED_EDGE('',*,*,#1839,.T.);
#2667=ORIENTED_EDGE('',*,*,#1840,.F.);
#2668=ORIENTED_EDGE('',*,*,#1841,.F.);
#2669=ORIENTED_EDGE('',*,*,#1842,.F.);
#2670=ORIENTED_EDGE('',*,*,#1836,.T.);
#2671=ORIENTED_EDGE('',*,*,#1843,.T.);
#2672=ORIENTED_EDGE('',*,*,#1844,.T.);
#2673=ORIENTED_EDGE('',*,*,#1845,.F.);
#2674=ORIENTED_EDGE('',*,*,#1846,.T.);
#2675=ORIENTED_EDGE('',*,*,#1847,.F.);
#2676=ORIENTED_EDGE('',*,*,#1848,.T.);
#2677=ORIENTED_EDGE('',*,*,#1849,.F.);
#2678=ORIENTED_EDGE('',*,*,#1850,.T.);
#2679=ORIENTED_EDGE('',*,*,#1845,.T.);
#2680=ORIENTED_EDGE('',*,*,#1851,.T.);
#2681=ORIENTED_EDGE('',*,*,#1852,.F.);
#2682=ORIENTED_EDGE('',*,*,#1853,.T.);
#2683=ORIENTED_EDGE('',*,*,#1849,.T.);
#2684=ORIENTED_EDGE('',*,*,#1854,.T.);
#2685=ORIENTED_EDGE('',*,*,#1855,.F.);
#2686=ORIENTED_EDGE('',*,*,#1856,.T.);
#2687=ORIENTED_EDGE('',*,*,#1852,.T.);
#2688=ORIENTED_EDGE('',*,*,#1857,.T.);
#2689=ORIENTED_EDGE('',*,*,#1858,.F.);
#2690=ORIENTED_EDGE('',*,*,#1859,.T.);
#2691=ORIENTED_EDGE('',*,*,#1855,.T.);
#2692=ORIENTED_EDGE('',*,*,#1860,.T.);
#2693=ORIENTED_EDGE('',*,*,#1861,.F.);
#2694=ORIENTED_EDGE('',*,*,#1862,.T.);
#2695=ORIENTED_EDGE('',*,*,#1858,.T.);
#2696=ORIENTED_EDGE('',*,*,#1863,.T.);
#2697=ORIENTED_EDGE('',*,*,#1864,.F.);
#2698=ORIENTED_EDGE('',*,*,#1865,.T.);
#2699=ORIENTED_EDGE('',*,*,#1861,.T.);
#2700=ORIENTED_EDGE('',*,*,#1866,.T.);
#2701=ORIENTED_EDGE('',*,*,#1867,.F.);
#2702=ORIENTED_EDGE('',*,*,#1868,.T.);
#2703=ORIENTED_EDGE('',*,*,#1864,.T.);
#2704=ORIENTED_EDGE('',*,*,#1869,.T.);
#2705=ORIENTED_EDGE('',*,*,#1870,.F.);
#2706=ORIENTED_EDGE('',*,*,#1871,.T.);
#2707=ORIENTED_EDGE('',*,*,#1867,.T.);
#2708=ORIENTED_EDGE('',*,*,#1872,.T.);
#2709=ORIENTED_EDGE('',*,*,#1873,.F.);
#2710=ORIENTED_EDGE('',*,*,#1874,.T.);
#2711=ORIENTED_EDGE('',*,*,#1870,.T.);
#2712=ORIENTED_EDGE('',*,*,#1875,.T.);
#2713=ORIENTED_EDGE('',*,*,#1876,.F.);
#2714=ORIENTED_EDGE('',*,*,#1877,.T.);
#2715=ORIENTED_EDGE('',*,*,#1873,.T.);
#2716=ORIENTED_EDGE('',*,*,#1878,.T.);
#2717=ORIENTED_EDGE('',*,*,#1879,.F.);
#2718=ORIENTED_EDGE('',*,*,#1880,.T.);
#2719=ORIENTED_EDGE('',*,*,#1876,.T.);
#2720=ORIENTED_EDGE('',*,*,#1881,.T.);
#2721=ORIENTED_EDGE('',*,*,#1882,.F.);
#2722=ORIENTED_EDGE('',*,*,#1883,.T.);
#2723=ORIENTED_EDGE('',*,*,#1879,.T.);
#2724=ORIENTED_EDGE('',*,*,#1884,.T.);
#2725=ORIENTED_EDGE('',*,*,#1885,.F.);
#2726=ORIENTED_EDGE('',*,*,#1886,.T.);
#2727=ORIENTED_EDGE('',*,*,#1882,.T.);
#2728=ORIENTED_EDGE('',*,*,#1887,.T.);
#2729=ORIENTED_EDGE('',*,*,#1888,.F.);
#2730=ORIENTED_EDGE('',*,*,#1889,.T.);
#2731=ORIENTED_EDGE('',*,*,#1885,.T.);
#2732=ORIENTED_EDGE('',*,*,#1890,.T.);
#2733=ORIENTED_EDGE('',*,*,#1891,.F.);
#2734=ORIENTED_EDGE('',*,*,#1892,.T.);
#2735=ORIENTED_EDGE('',*,*,#1888,.T.);
#2736=ORIENTED_EDGE('',*,*,#1893,.T.);
#2737=ORIENTED_EDGE('',*,*,#1894,.F.);
#2738=ORIENTED_EDGE('',*,*,#1895,.T.);
#2739=ORIENTED_EDGE('',*,*,#1891,.T.);
#2740=ORIENTED_EDGE('',*,*,#1896,.T.);
#2741=ORIENTED_EDGE('',*,*,#1897,.F.);
#2742=ORIENTED_EDGE('',*,*,#1898,.T.);
#2743=ORIENTED_EDGE('',*,*,#1894,.T.);
#2744=ORIENTED_EDGE('',*,*,#1899,.T.);
#2745=ORIENTED_EDGE('',*,*,#1900,.F.);
#2746=ORIENTED_EDGE('',*,*,#1901,.T.);
#2747=ORIENTED_EDGE('',*,*,#1897,.T.);
#2748=ORIENTED_EDGE('',*,*,#1902,.T.);
#2749=ORIENTED_EDGE('',*,*,#1903,.F.);
#2750=ORIENTED_EDGE('',*,*,#1904,.T.);
#2751=ORIENTED_EDGE('',*,*,#1900,.T.);
#2752=ORIENTED_EDGE('',*,*,#1905,.T.);
#2753=ORIENTED_EDGE('',*,*,#1906,.F.);
#2754=ORIENTED_EDGE('',*,*,#1907,.T.);
#2755=ORIENTED_EDGE('',*,*,#1903,.T.);
#2756=ORIENTED_EDGE('',*,*,#1908,.T.);
#2757=ORIENTED_EDGE('',*,*,#1906,.T.);
#2758=ORIENTED_EDGE('',*,*,#1909,.T.);
#2759=ORIENTED_EDGE('',*,*,#1910,.F.);
#2760=ORIENTED_EDGE('',*,*,#1911,.T.);
#2761=ORIENTED_EDGE('',*,*,#1840,.T.);
#2762=ORIENTED_EDGE('',*,*,#1912,.T.);
#2763=ORIENTED_EDGE('',*,*,#1913,.F.);
#2764=ORIENTED_EDGE('',*,*,#1914,.F.);
#2765=ORIENTED_EDGE('',*,*,#1915,.F.);
#2766=ORIENTED_EDGE('',*,*,#1916,.F.);
#2767=ORIENTED_EDGE('',*,*,#1909,.F.);
#2768=ORIENTED_EDGE('',*,*,#1908,.F.);
#2769=ORIENTED_EDGE('',*,*,#1905,.F.);
#2770=ORIENTED_EDGE('',*,*,#1902,.F.);
#2771=ORIENTED_EDGE('',*,*,#1899,.F.);
#2772=ORIENTED_EDGE('',*,*,#1896,.F.);
#2773=ORIENTED_EDGE('',*,*,#1893,.F.);
#2774=ORIENTED_EDGE('',*,*,#1890,.F.);
#2775=ORIENTED_EDGE('',*,*,#1887,.F.);
#2776=ORIENTED_EDGE('',*,*,#1884,.F.);
#2777=ORIENTED_EDGE('',*,*,#1881,.F.);
#2778=ORIENTED_EDGE('',*,*,#1878,.F.);
#2779=ORIENTED_EDGE('',*,*,#1875,.F.);
#2780=ORIENTED_EDGE('',*,*,#1872,.F.);
#2781=ORIENTED_EDGE('',*,*,#1869,.F.);
#2782=ORIENTED_EDGE('',*,*,#1866,.F.);
#2783=ORIENTED_EDGE('',*,*,#1863,.F.);
#2784=ORIENTED_EDGE('',*,*,#1860,.F.);
#2785=ORIENTED_EDGE('',*,*,#1857,.F.);
#2786=ORIENTED_EDGE('',*,*,#1854,.F.);
#2787=ORIENTED_EDGE('',*,*,#1851,.F.);
#2788=ORIENTED_EDGE('',*,*,#1848,.F.);
#2789=ORIENTED_EDGE('',*,*,#1917,.F.);
#2790=ORIENTED_EDGE('',*,*,#1918,.T.);
#2791=ORIENTED_EDGE('',*,*,#1761,.T.);
#2792=ORIENTED_EDGE('',*,*,#1765,.T.);
#2793=ORIENTED_EDGE('',*,*,#1770,.T.);
#2794=ORIENTED_EDGE('',*,*,#1769,.T.);
#2795=ORIENTED_EDGE('',*,*,#1773,.T.);
#2796=ORIENTED_EDGE('',*,*,#1778,.T.);
#2797=ORIENTED_EDGE('',*,*,#1777,.T.);
#2798=ORIENTED_EDGE('',*,*,#1781,.T.);
#2799=ORIENTED_EDGE('',*,*,#1786,.T.);
#2800=ORIENTED_EDGE('',*,*,#1785,.T.);
#2801=ORIENTED_EDGE('',*,*,#1789,.T.);
#2802=ORIENTED_EDGE('',*,*,#1794,.T.);
#2803=ORIENTED_EDGE('',*,*,#1793,.T.);
#2804=ORIENTED_EDGE('',*,*,#1797,.T.);
#2805=ORIENTED_EDGE('',*,*,#1802,.T.);
#2806=ORIENTED_EDGE('',*,*,#1801,.T.);
#2807=ORIENTED_EDGE('',*,*,#1805,.T.);
#2808=ORIENTED_EDGE('',*,*,#1810,.T.);
#2809=ORIENTED_EDGE('',*,*,#1809,.T.);
#2810=ORIENTED_EDGE('',*,*,#1813,.T.);
#2811=ORIENTED_EDGE('',*,*,#1818,.T.);
#2812=ORIENTED_EDGE('',*,*,#1817,.T.);
#2813=ORIENTED_EDGE('',*,*,#1821,.T.);
#2814=ORIENTED_EDGE('',*,*,#1826,.T.);
#2815=ORIENTED_EDGE('',*,*,#1825,.T.);
#2816=ORIENTED_EDGE('',*,*,#1829,.T.);
#2817=ORIENTED_EDGE('',*,*,#1834,.T.);
#2818=ORIENTED_EDGE('',*,*,#1833,.T.);
#2819=ORIENTED_EDGE('',*,*,#1837,.T.);
#2820=ORIENTED_EDGE('',*,*,#1842,.T.);
#2821=ORIENTED_EDGE('',*,*,#1841,.T.);
#2822=ORIENTED_EDGE('',*,*,#1915,.T.);
#2823=ORIENTED_EDGE('',*,*,#1914,.T.);
#2824=ORIENTED_EDGE('',*,*,#1919,.F.);
#2825=ORIENTED_EDGE('',*,*,#1920,.F.);
#2826=ORIENTED_EDGE('',*,*,#1912,.F.);
#2827=ORIENTED_EDGE('',*,*,#1844,.F.);
#2828=ORIENTED_EDGE('',*,*,#1843,.F.);
#2829=ORIENTED_EDGE('',*,*,#1839,.F.);
#2830=ORIENTED_EDGE('',*,*,#1838,.F.);
#2831=ORIENTED_EDGE('',*,*,#1835,.F.);
#2832=ORIENTED_EDGE('',*,*,#1831,.F.);
#2833=ORIENTED_EDGE('',*,*,#1830,.F.);
#2834=ORIENTED_EDGE('',*,*,#1827,.F.);
#2835=ORIENTED_EDGE('',*,*,#1823,.F.);
#2836=ORIENTED_EDGE('',*,*,#1822,.F.);
#2837=ORIENTED_EDGE('',*,*,#1819,.F.);
#2838=ORIENTED_EDGE('',*,*,#1815,.F.);
#2839=ORIENTED_EDGE('',*,*,#1814,.F.);
#2840=ORIENTED_EDGE('',*,*,#1811,.F.);
#2841=ORIENTED_EDGE('',*,*,#1807,.F.);
#2842=ORIENTED_EDGE('',*,*,#1806,.F.);
#2843=ORIENTED_EDGE('',*,*,#1803,.F.);
#2844=ORIENTED_EDGE('',*,*,#1799,.F.);
#2845=ORIENTED_EDGE('',*,*,#1798,.F.);
#2846=ORIENTED_EDGE('',*,*,#1795,.F.);
#2847=ORIENTED_EDGE('',*,*,#1791,.F.);
#2848=ORIENTED_EDGE('',*,*,#1790,.F.);
#2849=ORIENTED_EDGE('',*,*,#1787,.F.);
#2850=ORIENTED_EDGE('',*,*,#1783,.F.);
#2851=ORIENTED_EDGE('',*,*,#1782,.F.);
#2852=ORIENTED_EDGE('',*,*,#1779,.F.);
#2853=ORIENTED_EDGE('',*,*,#1775,.F.);
#2854=ORIENTED_EDGE('',*,*,#1774,.F.);
#2855=ORIENTED_EDGE('',*,*,#1771,.F.);
#2856=ORIENTED_EDGE('',*,*,#1767,.F.);
#2857=ORIENTED_EDGE('',*,*,#1766,.F.);
#2858=ORIENTED_EDGE('',*,*,#1763,.F.);
#2859=ORIENTED_EDGE('',*,*,#1921,.F.);
#2860=ORIENTED_EDGE('',*,*,#1846,.F.);
#2861=ORIENTED_EDGE('',*,*,#1850,.F.);
#2862=ORIENTED_EDGE('',*,*,#1853,.F.);
#2863=ORIENTED_EDGE('',*,*,#1856,.F.);
#2864=ORIENTED_EDGE('',*,*,#1859,.F.);
#2865=ORIENTED_EDGE('',*,*,#1862,.F.);
#2866=ORIENTED_EDGE('',*,*,#1865,.F.);
#2867=ORIENTED_EDGE('',*,*,#1868,.F.);
#2868=ORIENTED_EDGE('',*,*,#1871,.F.);
#2869=ORIENTED_EDGE('',*,*,#1874,.F.);
#2870=ORIENTED_EDGE('',*,*,#1877,.F.);
#2871=ORIENTED_EDGE('',*,*,#1880,.F.);
#2872=ORIENTED_EDGE('',*,*,#1883,.F.);
#2873=ORIENTED_EDGE('',*,*,#1886,.F.);
#2874=ORIENTED_EDGE('',*,*,#1889,.F.);
#2875=ORIENTED_EDGE('',*,*,#1892,.F.);
#2876=ORIENTED_EDGE('',*,*,#1895,.F.);
#2877=ORIENTED_EDGE('',*,*,#1898,.F.);
#2878=ORIENTED_EDGE('',*,*,#1901,.F.);
#2879=ORIENTED_EDGE('',*,*,#1904,.F.);
#2880=ORIENTED_EDGE('',*,*,#1907,.F.);
#2881=ORIENTED_EDGE('',*,*,#1911,.F.);
#2882=ORIENTED_EDGE('',*,*,#1916,.T.);
#2883=ORIENTED_EDGE('',*,*,#1913,.T.);
#2884=ORIENTED_EDGE('',*,*,#1920,.T.);
#2885=ORIENTED_EDGE('',*,*,#1919,.T.);
#2886=ORIENTED_EDGE('',*,*,#1910,.T.);
#2887=ORIENTED_EDGE('',*,*,#1917,.T.);
#2888=ORIENTED_EDGE('',*,*,#1847,.T.);
#2889=ORIENTED_EDGE('',*,*,#1921,.T.);
#2890=ORIENTED_EDGE('',*,*,#1762,.T.);
#2891=ORIENTED_EDGE('',*,*,#1918,.F.);
#2892=CYLINDRICAL_SURFACE('',#3266,1.08063175605657);
#2893=CYLINDRICAL_SURFACE('',#3275,2.16126351211314);
#2894=CYLINDRICAL_SURFACE('',#3278,2.5);
#2895=CYLINDRICAL_SURFACE('',#3285,1.08063175605657);
#2896=CYLINDRICAL_SURFACE('',#3293,3.90634189295527);
#2897=CYLINDRICAL_SURFACE('',#3300,1.543);
#2898=CYLINDRICAL_SURFACE('',#3302,1.543);
#2899=CYLINDRICAL_SURFACE('',#3303,1.543);
#2900=CYLINDRICAL_SURFACE('',#3305,1.2645);
#2901=CYLINDRICAL_SURFACE('',#3307,1.2645);
#2902=CYLINDRICAL_SURFACE('',#3308,1.2645);
#2903=CYLINDRICAL_SURFACE('',#3310,1.2645);
#2904=CYLINDRICAL_SURFACE('',#3311,1.543);
#2905=CYLINDRICAL_SURFACE('',#3321,1.08063175605657);
#2906=CYLINDRICAL_SURFACE('',#3331,2.16126351211314);
#2907=CYLINDRICAL_SURFACE('',#3334,2.5);
#2908=CYLINDRICAL_SURFACE('',#3343,1.08063175605657);
#2909=CYLINDRICAL_SURFACE('',#3348,1.08063175605657);
#2910=CYLINDRICAL_SURFACE('',#3352,1.17775);
#2911=CYLINDRICAL_SURFACE('',#3354,1.17775);
#2912=CYLINDRICAL_SURFACE('',#3355,1.17775);
#2913=CYLINDRICAL_SURFACE('',#3356,1.17775);
#2914=CYLINDRICAL_SURFACE('',#3357,1.17775);
#2915=CYLINDRICAL_SURFACE('',#3358,1.17775);
#2916=CYLINDRICAL_SURFACE('',#3359,1.17775);
#2917=CYLINDRICAL_SURFACE('',#3360,1.17775);
#2918=CYLINDRICAL_SURFACE('',#3361,1.17775);
#2919=CYLINDRICAL_SURFACE('',#3362,1.17775);
#2920=CYLINDRICAL_SURFACE('',#3363,1.17775);
#2921=CYLINDRICAL_SURFACE('',#3364,1.17775);
#2922=CYLINDRICAL_SURFACE('',#3365,1.17775);
#2923=CYLINDRICAL_SURFACE('',#3366,1.17775);
#2924=CYLINDRICAL_SURFACE('',#3367,1.17775);
#2925=CYLINDRICAL_SURFACE('',#3368,1.17775);
#2926=CYLINDRICAL_SURFACE('',#3369,1.17775);
#2927=CYLINDRICAL_SURFACE('',#3370,1.17775);
#2928=CYLINDRICAL_SURFACE('',#3371,1.17775);
#2929=CYLINDRICAL_SURFACE('',#3372,1.17775);
#2930=CYLINDRICAL_SURFACE('',#3373,1.17775);
#2931=CYLINDRICAL_SURFACE('',#3374,1.4635);
#2932=CYLINDRICAL_SURFACE('',#3376,1.4635);
#2933=CYLINDRICAL_SURFACE('',#3377,1.4635);
#2934=CYLINDRICAL_SURFACE('',#3378,1.4635);
#2935=CYLINDRICAL_SURFACE('',#3379,1.4635);
#2936=CYLINDRICAL_SURFACE('',#3380,1.4635);
#2937=CYLINDRICAL_SURFACE('',#3381,1.4635);
#2938=CYLINDRICAL_SURFACE('',#3382,1.4635);
#2939=CYLINDRICAL_SURFACE('',#3383,1.4635);
#2940=CYLINDRICAL_SURFACE('',#3384,1.4635);
#2941=CYLINDRICAL_SURFACE('',#3385,1.4635);
#2942=CYLINDRICAL_SURFACE('',#3386,1.4635);
#2943=CYLINDRICAL_SURFACE('',#3387,1.4635);
#2944=CYLINDRICAL_SURFACE('',#3388,1.4635);
#2945=CYLINDRICAL_SURFACE('',#3389,1.4635);
#2946=CYLINDRICAL_SURFACE('',#3390,1.4635);
#2947=CYLINDRICAL_SURFACE('',#3391,1.4635);
#2948=CYLINDRICAL_SURFACE('',#3392,1.4635);
#2949=CYLINDRICAL_SURFACE('',#3393,1.4635);
#2950=CYLINDRICAL_SURFACE('',#3394,1.4635);
#2951=CYLINDRICAL_SURFACE('',#3395,1.4635);
#2952=CYLINDRICAL_SURFACE('',#3396,1.4635);
#2953=CYLINDRICAL_SURFACE('',#3398,1.17775);
#2954=CYLINDRICAL_SURFACE('',#3403,1.543);
#2955=CYLINDRICAL_SURFACE('',#3405,1.543);
#2956=CYLINDRICAL_SURFACE('',#3406,1.543);
#2957=CYLINDRICAL_SURFACE('',#3408,1.2645);
#2958=CYLINDRICAL_SURFACE('',#3410,1.2645);
#2959=CYLINDRICAL_SURFACE('',#3411,1.2645);
#2960=CYLINDRICAL_SURFACE('',#3413,1.2645);
#2961=CYLINDRICAL_SURFACE('',#3414,1.543);
#2962=CYLINDRICAL_SURFACE('',#3424,1.17775);
#2963=CYLINDRICAL_SURFACE('',#3426,1.17775);
#2964=CYLINDRICAL_SURFACE('',#3427,1.17775);
#2965=CYLINDRICAL_SURFACE('',#3428,1.17775);
#2966=CYLINDRICAL_SURFACE('',#3429,1.17775);
#2967=CYLINDRICAL_SURFACE('',#3430,1.17775);
#2968=CYLINDRICAL_SURFACE('',#3431,1.17775);
#2969=CYLINDRICAL_SURFACE('',#3432,1.17775);
#2970=CYLINDRICAL_SURFACE('',#3433,1.17775);
#2971=CYLINDRICAL_SURFACE('',#3434,1.17775);
#2972=CYLINDRICAL_SURFACE('',#3435,1.17775);
#2973=CYLINDRICAL_SURFACE('',#3436,1.17775);
#2974=CYLINDRICAL_SURFACE('',#3437,1.17775);
#2975=CYLINDRICAL_SURFACE('',#3438,1.17775);
#2976=CYLINDRICAL_SURFACE('',#3439,1.17775);
#2977=CYLINDRICAL_SURFACE('',#3440,1.17775);
#2978=CYLINDRICAL_SURFACE('',#3441,1.17775);
#2979=CYLINDRICAL_SURFACE('',#3442,1.17775);
#2980=CYLINDRICAL_SURFACE('',#3443,1.17775);
#2981=CYLINDRICAL_SURFACE('',#3444,1.17775);
#2982=CYLINDRICAL_SURFACE('',#3445,1.17775);
#2983=CYLINDRICAL_SURFACE('',#3446,1.4635);
#2984=CYLINDRICAL_SURFACE('',#3448,1.4635);
#2985=CYLINDRICAL_SURFACE('',#3449,1.4635);
#2986=CYLINDRICAL_SURFACE('',#3450,1.4635);
#2987=CYLINDRICAL_SURFACE('',#3451,1.4635);
#2988=CYLINDRICAL_SURFACE('',#3452,1.4635);
#2989=CYLINDRICAL_SURFACE('',#3453,1.4635);
#2990=CYLINDRICAL_SURFACE('',#3454,1.4635);
#2991=CYLINDRICAL_SURFACE('',#3455,1.4635);
#2992=CYLINDRICAL_SURFACE('',#3456,1.4635);
#2993=CYLINDRICAL_SURFACE('',#3457,1.4635);
#2994=CYLINDRICAL_SURFACE('',#3458,1.4635);
#2995=CYLINDRICAL_SURFACE('',#3459,1.4635);
#2996=CYLINDRICAL_SURFACE('',#3460,1.4635);
#2997=CYLINDRICAL_SURFACE('',#3461,1.4635);
#2998=CYLINDRICAL_SURFACE('',#3462,1.4635);
#2999=CYLINDRICAL_SURFACE('',#3463,1.4635);
#3000=CYLINDRICAL_SURFACE('',#3464,1.4635);
#3001=CYLINDRICAL_SURFACE('',#3465,1.4635);
#3002=CYLINDRICAL_SURFACE('',#3466,1.4635);
#3003=CYLINDRICAL_SURFACE('',#3467,1.4635);
#3004=CYLINDRICAL_SURFACE('',#3468,1.4635);
#3005=CYLINDRICAL_SURFACE('',#3470,1.17775);
#3006=ADVANCED_FACE('',(#427),#2892,.F.);
#3007=ADVANCED_FACE('',(#428),#395,.T.);
#3008=ADVANCED_FACE('',(#429),#391,.T.);
#3009=ADVANCED_FACE('',(#430,#381),#396,.T.);
#3010=ADVANCED_FACE('',(#431),#2893,.T.);
#3011=ADVANCED_FACE('',(#432),#2894,.F.);
#3012=ADVANCED_FACE('',(#433),#397,.F.);
#3013=ADVANCED_FACE('',(#434,#382),#379,.T.);
#3014=ADVANCED_FACE('',(#435),#2895,.F.);
#3015=ADVANCED_FACE('',(#436,#383),#398,.T.);
#3016=ADVANCED_FACE('',(#437),#392,.T.);
#3017=ADVANCED_FACE('',(#438),#2896,.T.);
#3018=ADVANCED_FACE('',(#439),#393,.T.);
#3019=ADVANCED_FACE('',(#440,#384),#399,.T.);
#3020=ADVANCED_FACE('',(#441),#2897,.F.);
#3021=ADVANCED_FACE('',(#442),#2898,.F.);
#3022=ADVANCED_FACE('',(#443),#2899,.F.);
#3023=ADVANCED_FACE('',(#444),#2900,.F.);
#3024=ADVANCED_FACE('',(#445),#2901,.F.);
#3025=ADVANCED_FACE('',(#446),#2902,.F.);
#3026=ADVANCED_FACE('',(#447),#2903,.F.);
#3027=ADVANCED_FACE('',(#448),#2904,.F.);
#3028=ADVANCED_FACE('',(#449),#43,.F.);
#3029=ADVANCED_FACE('',(#450),#44,.F.);
#3030=ADVANCED_FACE('',(#451,#385),#400,.T.);
#3031=ADVANCED_FACE('',(#452),#401,.T.);
#3032=ADVANCED_FACE('',(#453),#402,.T.);
#3033=ADVANCED_FACE('',(#454),#403,.T.);
#3034=ADVANCED_FACE('',(#455),#404,.T.);
#3035=ADVANCED_FACE('',(#456),#405,.T.);
#3036=ADVANCED_FACE('',(#457),#406,.T.);
#3037=ADVANCED_FACE('',(#458,#386),#407,.F.);
#3038=ADVANCED_FACE('',(#459),#2905,.F.);
#3039=ADVANCED_FACE('',(#460),#408,.T.);
#3040=ADVANCED_FACE('',(#461),#394,.T.);
#3041=ADVANCED_FACE('',(#462,#387),#409,.T.);
#3042=ADVANCED_FACE('',(#463),#2906,.T.);
#3043=ADVANCED_FACE('',(#464),#2907,.F.);
#3044=ADVANCED_FACE('',(#465),#410,.F.);
#3045=ADVANCED_FACE('',(#466,#388),#380,.T.);
#3046=ADVANCED_FACE('',(#467),#411,.F.);
#3047=ADVANCED_FACE('',(#468),#2908,.T.);
#3048=ADVANCED_FACE('',(#469),#412,.T.);
#3049=ADVANCED_FACE('',(#470),#413,.T.);
#3050=ADVANCED_FACE('',(#471),#2909,.T.);
#3051=ADVANCED_FACE('',(#472),#414,.T.);
#3052=ADVANCED_FACE('',(#473),#2910,.T.);
#3053=ADVANCED_FACE('',(#474),#2911,.T.);
#3054=ADVANCED_FACE('',(#475),#2912,.T.);
#3055=ADVANCED_FACE('',(#476),#2913,.T.);
#3056=ADVANCED_FACE('',(#477),#2914,.T.);
#3057=ADVANCED_FACE('',(#478),#2915,.T.);
#3058=ADVANCED_FACE('',(#479),#2916,.T.);
#3059=ADVANCED_FACE('',(#480),#2917,.T.);
#3060=ADVANCED_FACE('',(#481),#2918,.T.);
#3061=ADVANCED_FACE('',(#482),#2919,.T.);
#3062=ADVANCED_FACE('',(#483),#2920,.T.);
#3063=ADVANCED_FACE('',(#484),#2921,.T.);
#3064=ADVANCED_FACE('',(#485),#2922,.T.);
#3065=ADVANCED_FACE('',(#486),#2923,.T.);
#3066=ADVANCED_FACE('',(#487),#2924,.T.);
#3067=ADVANCED_FACE('',(#488),#2925,.T.);
#3068=ADVANCED_FACE('',(#489),#2926,.T.);
#3069=ADVANCED_FACE('',(#490),#2927,.T.);
#3070=ADVANCED_FACE('',(#491),#2928,.T.);
#3071=ADVANCED_FACE('',(#492),#2929,.T.);
#3072=ADVANCED_FACE('',(#493),#2930,.T.);
#3073=ADVANCED_FACE('',(#494),#2931,.T.);
#3074=ADVANCED_FACE('',(#495),#2932,.T.);
#3075=ADVANCED_FACE('',(#496),#2933,.T.);
#3076=ADVANCED_FACE('',(#497),#2934,.T.);
#3077=ADVANCED_FACE('',(#498),#2935,.T.);
#3078=ADVANCED_FACE('',(#499),#2936,.T.);
#3079=ADVANCED_FACE('',(#500),#2937,.T.);
#3080=ADVANCED_FACE('',(#501),#2938,.T.);
#3081=ADVANCED_FACE('',(#502),#2939,.T.);
#3082=ADVANCED_FACE('',(#503),#2940,.T.);
#3083=ADVANCED_FACE('',(#504),#2941,.T.);
#3084=ADVANCED_FACE('',(#505),#2942,.T.);
#3085=ADVANCED_FACE('',(#506),#2943,.T.);
#3086=ADVANCED_FACE('',(#507),#2944,.T.);
#3087=ADVANCED_FACE('',(#508),#2945,.T.);
#3088=ADVANCED_FACE('',(#509),#2946,.T.);
#3089=ADVANCED_FACE('',(#510),#2947,.T.);
#3090=ADVANCED_FACE('',(#511),#2948,.T.);
#3091=ADVANCED_FACE('',(#512),#2949,.T.);
#3092=ADVANCED_FACE('',(#513),#2950,.T.);
#3093=ADVANCED_FACE('',(#514),#2951,.T.);
#3094=ADVANCED_FACE('',(#515),#2952,.T.);
#3095=ADVANCED_FACE('',(#516),#2953,.T.);
#3096=ADVANCED_FACE('',(#517),#45,.F.);
#3097=ADVANCED_FACE('',(#518),#46,.F.);
#3098=ADVANCED_FACE('',(#519),#415,.F.);
#3099=ADVANCED_FACE('',(#520),#416,.T.);
#3100=ADVANCED_FACE('',(#521),#2954,.F.);
#3101=ADVANCED_FACE('',(#522),#2955,.F.);
#3102=ADVANCED_FACE('',(#523),#2956,.F.);
#3103=ADVANCED_FACE('',(#524),#2957,.F.);
#3104=ADVANCED_FACE('',(#525),#2958,.F.);
#3105=ADVANCED_FACE('',(#526),#2959,.F.);
#3106=ADVANCED_FACE('',(#527),#2960,.F.);
#3107=ADVANCED_FACE('',(#528),#2961,.F.);
#3108=ADVANCED_FACE('',(#529),#47,.F.);
#3109=ADVANCED_FACE('',(#530),#48,.F.);
#3110=ADVANCED_FACE('',(#531,#389),#417,.T.);
#3111=ADVANCED_FACE('',(#532),#418,.T.);
#3112=ADVANCED_FACE('',(#533),#419,.T.);
#3113=ADVANCED_FACE('',(#534),#420,.T.);
#3114=ADVANCED_FACE('',(#535),#421,.T.);
#3115=ADVANCED_FACE('',(#536),#422,.T.);
#3116=ADVANCED_FACE('',(#537),#423,.T.);
#3117=ADVANCED_FACE('',(#538,#390),#424,.F.);
#3118=ADVANCED_FACE('',(#539),#2962,.T.);
#3119=ADVANCED_FACE('',(#540),#2963,.T.);
#3120=ADVANCED_FACE('',(#541),#2964,.T.);
#3121=ADVANCED_FACE('',(#542),#2965,.T.);
#3122=ADVANCED_FACE('',(#543),#2966,.T.);
#3123=ADVANCED_FACE('',(#544),#2967,.T.);
#3124=ADVANCED_FACE('',(#545),#2968,.T.);
#3125=ADVANCED_FACE('',(#546),#2969,.T.);
#3126=ADVANCED_FACE('',(#547),#2970,.T.);
#3127=ADVANCED_FACE('',(#548),#2971,.T.);
#3128=ADVANCED_FACE('',(#549),#2972,.T.);
#3129=ADVANCED_FACE('',(#550),#2973,.T.);
#3130=ADVANCED_FACE('',(#551),#2974,.T.);
#3131=ADVANCED_FACE('',(#552),#2975,.T.);
#3132=ADVANCED_FACE('',(#553),#2976,.T.);
#3133=ADVANCED_FACE('',(#554),#2977,.T.);
#3134=ADVANCED_FACE('',(#555),#2978,.T.);
#3135=ADVANCED_FACE('',(#556),#2979,.T.);
#3136=ADVANCED_FACE('',(#557),#2980,.T.);
#3137=ADVANCED_FACE('',(#558),#2981,.T.);
#3138=ADVANCED_FACE('',(#559),#2982,.T.);
#3139=ADVANCED_FACE('',(#560),#2983,.T.);
#3140=ADVANCED_FACE('',(#561),#2984,.T.);
#3141=ADVANCED_FACE('',(#562),#2985,.T.);
#3142=ADVANCED_FACE('',(#563),#2986,.T.);
#3143=ADVANCED_FACE('',(#564),#2987,.T.);
#3144=ADVANCED_FACE('',(#565),#2988,.T.);
#3145=ADVANCED_FACE('',(#566),#2989,.T.);
#3146=ADVANCED_FACE('',(#567),#2990,.T.);
#3147=ADVANCED_FACE('',(#568),#2991,.T.);
#3148=ADVANCED_FACE('',(#569),#2992,.T.);
#3149=ADVANCED_FACE('',(#570),#2993,.T.);
#3150=ADVANCED_FACE('',(#571),#2994,.T.);
#3151=ADVANCED_FACE('',(#572),#2995,.T.);
#3152=ADVANCED_FACE('',(#573),#2996,.T.);
#3153=ADVANCED_FACE('',(#574),#2997,.T.);
#3154=ADVANCED_FACE('',(#575),#2998,.T.);
#3155=ADVANCED_FACE('',(#576),#2999,.T.);
#3156=ADVANCED_FACE('',(#577),#3000,.T.);
#3157=ADVANCED_FACE('',(#578),#3001,.T.);
#3158=ADVANCED_FACE('',(#579),#3002,.T.);
#3159=ADVANCED_FACE('',(#580),#3003,.T.);
#3160=ADVANCED_FACE('',(#581),#3004,.T.);
#3161=ADVANCED_FACE('',(#582),#3005,.T.);
#3162=ADVANCED_FACE('',(#583),#49,.F.);
#3163=ADVANCED_FACE('',(#584),#50,.F.);
#3164=ADVANCED_FACE('',(#585),#425,.F.);
#3165=ADVANCED_FACE('',(#586),#426,.T.);
#3166=CLOSED_SHELL('',(#3006,#3007,#3008,#3009,#3010,#3011,#3012,#3013));
#3167=CLOSED_SHELL('',(#3014,#3015,#3016,#3017,#3018,#3019));
#3168=CLOSED_SHELL('',(#3020,#3021,#3022,#3023,#3024,#3025,#3026,#3027,
#3028,#3029,#3030,#3031,#3032,#3033,#3034,#3035,#3036,#3037));
#3169=CLOSED_SHELL('',(#3038,#3039,#3040,#3041,#3042,#3043,#3044,#3045));
#3170=CLOSED_SHELL('',(#3046,#3047,#3048));
#3171=CLOSED_SHELL('',(#3049,#3050,#3051));
#3172=CLOSED_SHELL('',(#3052,#3053,#3054,#3055,#3056,#3057,#3058,#3059,
#3060,#3061,#3062,#3063,#3064,#3065,#3066,#3067,#3068,#3069,#3070,#3071,
#3072,#3073,#3074,#3075,#3076,#3077,#3078,#3079,#3080,#3081,#3082,#3083,
#3084,#3085,#3086,#3087,#3088,#3089,#3090,#3091,#3092,#3093,#3094,#3095,
#3096,#3097,#3098,#3099));
#3173=CLOSED_SHELL('',(#3100,#3101,#3102,#3103,#3104,#3105,#3106,#3107,
#3108,#3109,#3110,#3111,#3112,#3113,#3114,#3115,#3116,#3117));
#3174=CLOSED_SHELL('',(#3118,#3119,#3120,#3121,#3122,#3123,#3124,#3125,
#3126,#3127,#3128,#3129,#3130,#3131,#3132,#3133,#3134,#3135,#3136,#3137,
#3138,#3139,#3140,#3141,#3142,#3143,#3144,#3145,#3146,#3147,#3148,#3149,
#3150,#3151,#3152,#3153,#3154,#3155,#3156,#3157,#3158,#3159,#3160,#3161,
#3162,#3163,#3164,#3165));
#3175=DERIVED_UNIT_ELEMENT(#3191,1.);
#3176=DERIVED_UNIT_ELEMENT(#40736,-3.);
#3177=DERIVED_UNIT_ELEMENT(#3191,1.);
#3178=DERIVED_UNIT_ELEMENT(#40736,-3.);
#3179=DERIVED_UNIT_ELEMENT(#3191,1.);
#3180=DERIVED_UNIT_ELEMENT(#40736,-3.);
#3181=DERIVED_UNIT_ELEMENT(#3191,1.);
#3182=DERIVED_UNIT_ELEMENT(#40736,-3.);
#3183=DERIVED_UNIT_ELEMENT(#3191,1.);
#3184=DERIVED_UNIT_ELEMENT(#40736,-3.);
#3185=DERIVED_UNIT_ELEMENT(#3191,1.);
#3186=DERIVED_UNIT_ELEMENT(#40736,-3.);
#3187=DERIVED_UNIT_ELEMENT(#3191,1.);
#3188=DERIVED_UNIT_ELEMENT(#40736,-3.);
#3189=DERIVED_UNIT_ELEMENT(#3191,1.);
#3190=DERIVED_UNIT_ELEMENT(#40736,-3.);
#3191=(
MASS_UNIT()
NAMED_UNIT(*)
SI_UNIT(.KILO.,.GRAM.)
);
#3192=DERIVED_UNIT((#3175,#3176));
#3193=DERIVED_UNIT((#3177,#3178));
#3194=DERIVED_UNIT((#3179,#3180));
#3195=DERIVED_UNIT((#3181,#3182));
#3196=DERIVED_UNIT((#3183,#3184));
#3197=DERIVED_UNIT((#3185,#3186));
#3198=DERIVED_UNIT((#3187,#3188));
#3199=DERIVED_UNIT((#3189,#3190));
#3200=MEASURE_REPRESENTATION_ITEM('density measure',
POSITIVE_RATIO_MEASURE(7850.),#3192);
#3201=MEASURE_REPRESENTATION_ITEM('density measure',
POSITIVE_RATIO_MEASURE(7850.),#3193);
#3202=MEASURE_REPRESENTATION_ITEM('density measure',
POSITIVE_RATIO_MEASURE(7850.),#3194);
#3203=MEASURE_REPRESENTATION_ITEM('density measure',
POSITIVE_RATIO_MEASURE(7850.),#3195);
#3204=MEASURE_REPRESENTATION_ITEM('density measure',
POSITIVE_RATIO_MEASURE(7850.),#3196);
#3205=MEASURE_REPRESENTATION_ITEM('density measure',
POSITIVE_RATIO_MEASURE(7850.),#3197);
#3206=MEASURE_REPRESENTATION_ITEM('density measure',
POSITIVE_RATIO_MEASURE(7850.),#3198);
#3207=MEASURE_REPRESENTATION_ITEM('density measure',
POSITIVE_RATIO_MEASURE(7850.),#3199);
#3208=PROPERTY_DEFINITION_REPRESENTATION(#3248,#3224);
#3209=PROPERTY_DEFINITION_REPRESENTATION(#3249,#3225);
#3210=PROPERTY_DEFINITION_REPRESENTATION(#3250,#3226);
#3211=PROPERTY_DEFINITION_REPRESENTATION(#3251,#3227);
#3212=PROPERTY_DEFINITION_REPRESENTATION(#3252,#3228);
#3213=PROPERTY_DEFINITION_REPRESENTATION(#3253,#3229);
#3214=PROPERTY_DEFINITION_REPRESENTATION(#3254,#3230);
#3215=PROPERTY_DEFINITION_REPRESENTATION(#3255,#3231);
#3216=PROPERTY_DEFINITION_REPRESENTATION(#3256,#3232);
#3217=PROPERTY_DEFINITION_REPRESENTATION(#3257,#3233);
#3218=PROPERTY_DEFINITION_REPRESENTATION(#3258,#3234);
#3219=PROPERTY_DEFINITION_REPRESENTATION(#3259,#3235);
#3220=PROPERTY_DEFINITION_REPRESENTATION(#3260,#3236);
#3221=PROPERTY_DEFINITION_REPRESENTATION(#3261,#3237);
#3222=PROPERTY_DEFINITION_REPRESENTATION(#3262,#3238);
#3223=PROPERTY_DEFINITION_REPRESENTATION(#3263,#3239);
#3224=REPRESENTATION('material name',(#3240),#40726);
#3225=REPRESENTATION('density',(#3200),#40726);
#3226=REPRESENTATION('material name',(#3241),#40727);
#3227=REPRESENTATION('density',(#3201),#40727);
#3228=REPRESENTATION('material name',(#3242),#40728);
#3229=REPRESENTATION('density',(#3202),#40728);
#3230=REPRESENTATION('material name',(#3243),#40729);
#3231=REPRESENTATION('density',(#3203),#40729);
#3232=REPRESENTATION('material name',(#3244),#40730);
#3233=REPRESENTATION('density',(#3204),#40730);
#3234=REPRESENTATION('material name',(#3245),#40731);
#3235=REPRESENTATION('density',(#3205),#40731);
#3236=REPRESENTATION('material name',(#3246),#40732);
#3237=REPRESENTATION('density',(#3206),#40732);
#3238=REPRESENTATION('material name',(#3247),#40733);
#3239=REPRESENTATION('density',(#3207),#40733);
#3240=DESCRIPTIVE_REPRESENTATION_ITEM('Steel','Steel');
#3241=DESCRIPTIVE_REPRESENTATION_ITEM('Steel','Steel');
#3242=DESCRIPTIVE_REPRESENTATION_ITEM('Steel','Steel');
#3243=DESCRIPTIVE_REPRESENTATION_ITEM('Steel','Steel');
#3244=DESCRIPTIVE_REPRESENTATION_ITEM('Steel','Steel');
#3245=DESCRIPTIVE_REPRESENTATION_ITEM('Steel','Steel');
#3246=DESCRIPTIVE_REPRESENTATION_ITEM('Steel','Steel');
#3247=DESCRIPTIVE_REPRESENTATION_ITEM('Steel','Steel');
#3248=PROPERTY_DEFINITION('material property','material name',#40776);
#3249=PROPERTY_DEFINITION('material property','density of part',#40776);
#3250=PROPERTY_DEFINITION('material property','material name',#40777);
#3251=PROPERTY_DEFINITION('material property','density of part',#40777);
#3252=PROPERTY_DEFINITION('material property','material name',#40778);
#3253=PROPERTY_DEFINITION('material property','density of part',#40778);
#3254=PROPERTY_DEFINITION('material property','material name',#40779);
#3255=PROPERTY_DEFINITION('material property','density of part',#40779);
#3256=PROPERTY_DEFINITION('material property','material name',#40780);
#3257=PROPERTY_DEFINITION('material property','density of part',#40780);
#3258=PROPERTY_DEFINITION('material property','material name',#40781);
#3259=PROPERTY_DEFINITION('material property','density of part',#40781);
#3260=PROPERTY_DEFINITION('material property','material name',#40782);
#3261=PROPERTY_DEFINITION('material property','density of part',#40782);
#3262=PROPERTY_DEFINITION('material property','material name',#40783);
#3263=PROPERTY_DEFINITION('material property','density of part',#40783);
#3264=AXIS2_PLACEMENT_3D('',#4060,#3482,#3483);
#3265=AXIS2_PLACEMENT_3D('',#4061,#3484,#3485);
#3266=AXIS2_PLACEMENT_3D('',#4062,#3486,#3487);
#3267=AXIS2_PLACEMENT_3D('',#4064,#3488,#3489);
#3268=AXIS2_PLACEMENT_3D('',#4067,#3491,#3492);
#3269=AXIS2_PLACEMENT_3D('',#4068,#3493,#3494);
#3270=AXIS2_PLACEMENT_3D('',#4069,#3495,#3496);
#3271=AXIS2_PLACEMENT_3D('',#4071,#3497,#3498);
#3272=AXIS2_PLACEMENT_3D('',#4073,#3499,#3500);
#3273=AXIS2_PLACEMENT_3D('',#4074,#3501,#3502);
#3274=AXIS2_PLACEMENT_3D('',#4075,#3503,#3504);
#3275=AXIS2_PLACEMENT_3D('',#4076,#3505,#3506);
#3276=AXIS2_PLACEMENT_3D('',#4080,#3508,#3509);
#3277=AXIS2_PLACEMENT_3D('',#4081,#3510,#3511);
#3278=AXIS2_PLACEMENT_3D('',#4082,#3512,#3513);
#3279=AXIS2_PLACEMENT_3D('',#4084,#3514,#3515);
#3280=AXIS2_PLACEMENT_3D('',#4087,#3517,#3518);
#3281=AXIS2_PLACEMENT_3D('',#4088,#3519,#3520);
#3282=AXIS2_PLACEMENT_3D('',#4089,#3521,#3522);
#3283=AXIS2_PLACEMENT_3D('',#4091,#3523,#3524);
#3284=AXIS2_PLACEMENT_3D('',#4092,#3525,#3526);
#3285=AXIS2_PLACEMENT_3D('',#4093,#3527,#3528);
#3286=AXIS2_PLACEMENT_3D('',#4095,#3529,#3530);
#3287=AXIS2_PLACEMENT_3D('',#4098,#3532,#3533);
#3288=AXIS2_PLACEMENT_3D('',#4099,#3534,#3535);
#3289=AXIS2_PLACEMENT_3D('',#4101,#3536,#3537);
#3290=AXIS2_PLACEMENT_3D('',#4102,#3538,#3539);
#3291=AXIS2_PLACEMENT_3D('',#4104,#3540,#3541);
#3292=AXIS2_PLACEMENT_3D('',#4105,#3542,#3543);
#3293=AXIS2_PLACEMENT_3D('',#4106,#3544,#3545);
#3294=AXIS2_PLACEMENT_3D('',#4108,#3546,#3547);
#3295=AXIS2_PLACEMENT_3D('',#4110,#3549,#3550);
#3296=AXIS2_PLACEMENT_3D('',#4112,#3551,#3552);
#3297=AXIS2_PLACEMENT_3D('',#4113,#3553,#3554);
#3298=AXIS2_PLACEMENT_3D('',#4114,#3555,#3556);
#3299=AXIS2_PLACEMENT_3D('',#4115,#3557,#3558);
#3300=AXIS2_PLACEMENT_3D('',#4116,#3559,#3560);
#3301=AXIS2_PLACEMENT_3D('',#4128,#3562,#3563);
#3302=AXIS2_PLACEMENT_3D('',#4205,#3564,#3565);
#3303=AXIS2_PLACEMENT_3D('',#4508,#3567,#3568);
#3304=AXIS2_PLACEMENT_3D('',#4581,#3570,#3571);
#3305=AXIS2_PLACEMENT_3D('',#4642,#3572,#3573);
#3306=AXIS2_PLACEMENT_3D('',#4715,#3575,#3576);
#3307=AXIS2_PLACEMENT_3D('',#4798,#3577,#3578);
#3308=AXIS2_PLACEMENT_3D('',#5115,#3580,#3581);
#3309=AXIS2_PLACEMENT_3D('',#5173,#3583,#3584);
#3310=AXIS2_PLACEMENT_3D('',#5274,#3585,#3586);
#3311=AXIS2_PLACEMENT_3D('',#5629,#3587,#3588);
#3312=AXIS2_PLACEMENT_3D('',#6396,#3589,#3590);
#3313=AXIS2_PLACEMENT_3D('',#6409,#3597,#3598);
#3314=AXIS2_PLACEMENT_3D('',#6415,#3602,#3603);
#3315=AXIS2_PLACEMENT_3D('',#6419,#3606,#3607);
#3316=AXIS2_PLACEMENT_3D('',#6423,#3610,#3611);
#3317=AXIS2_PLACEMENT_3D('',#6427,#3614,#3615);
#3318=AXIS2_PLACEMENT_3D('',#6431,#3618,#3619);
#3319=AXIS2_PLACEMENT_3D('',#6433,#3621,#3622);
#3320=AXIS2_PLACEMENT_3D('',#6434,#3623,#3624);
#3321=AXIS2_PLACEMENT_3D('',#6435,#3625,#3626);
#3322=AXIS2_PLACEMENT_3D('',#6437,#3627,#3628);
#3323=AXIS2_PLACEMENT_3D('',#6440,#3630,#3631);
#3324=AXIS2_PLACEMENT_3D('',#6441,#3632,#3633);
#3325=AXIS2_PLACEMENT_3D('',#6442,#3634,#3635);
#3326=AXIS2_PLACEMENT_3D('',#6444,#3636,#3637);
#3327=AXIS2_PLACEMENT_3D('',#6446,#3638,#3639);
#3328=AXIS2_PLACEMENT_3D('',#6448,#3640,#3641);
#3329=AXIS2_PLACEMENT_3D('',#6449,#3642,#3643);
#3330=AXIS2_PLACEMENT_3D('',#6450,#3644,#3645);
#3331=AXIS2_PLACEMENT_3D('',#6451,#3646,#3647);
#3332=AXIS2_PLACEMENT_3D('',#6455,#3649,#3650);
#3333=AXIS2_PLACEMENT_3D('',#6456,#3651,#3652);
#3334=AXIS2_PLACEMENT_3D('',#6457,#3653,#3654);
#3335=AXIS2_PLACEMENT_3D('',#6459,#3655,#3656);
#3336=AXIS2_PLACEMENT_3D('',#6462,#3658,#3659);
#3337=AXIS2_PLACEMENT_3D('',#6463,#3660,#3661);
#3338=AXIS2_PLACEMENT_3D('',#6464,#3662,#3663);
#3339=AXIS2_PLACEMENT_3D('',#6466,#3664,#3665);
#3340=AXIS2_PLACEMENT_3D('',#6467,#3666,#3667);
#3341=AXIS2_PLACEMENT_3D('',#6468,#3668,#3669);
#3342=AXIS2_PLACEMENT_3D('',#6470,#3670,#3671);
#3343=AXIS2_PLACEMENT_3D('',#6471,#3672,#3673);
#3344=AXIS2_PLACEMENT_3D('',#6474,#3675,#3676);
#3345=AXIS2_PLACEMENT_3D('',#6475,#3677,#3678);
#3346=AXIS2_PLACEMENT_3D('',#6476,#3679,#3680);
#3347=AXIS2_PLACEMENT_3D('',#6478,#3681,#3682);
#3348=AXIS2_PLACEMENT_3D('',#6479,#3683,#3684);
#3349=AXIS2_PLACEMENT_3D('',#6482,#3686,#3687);
#3350=AXIS2_PLACEMENT_3D('',#6483,#3688,#3689);
#3351=AXIS2_PLACEMENT_3D('',#6484,#3690,#3691);
#3352=AXIS2_PLACEMENT_3D('',#6485,#3692,#3693);
#3353=AXIS2_PLACEMENT_3D('',#6595,#3695,#3696);
#3354=AXIS2_PLACEMENT_3D('',#6651,#3697,#3698);
#3355=AXIS2_PLACEMENT_3D('',#7079,#3700,#3701);
#3356=AXIS2_PLACEMENT_3D('',#7526,#3703,#3704);
#3357=AXIS2_PLACEMENT_3D('',#7973,#3706,#3707);
#3358=AXIS2_PLACEMENT_3D('',#8418,#3709,#3710);
#3359=AXIS2_PLACEMENT_3D('',#8867,#3712,#3713);
#3360=AXIS2_PLACEMENT_3D('',#9308,#3715,#3716);
#3361=AXIS2_PLACEMENT_3D('',#9755,#3718,#3719);
#3362=AXIS2_PLACEMENT_3D('',#10206,#3721,#3722);
#3363=AXIS2_PLACEMENT_3D('',#10643,#3724,#3725);
#3364=AXIS2_PLACEMENT_3D('',#11118,#3727,#3728);
#3365=AXIS2_PLACEMENT_3D('',#11571,#3730,#3731);
#3366=AXIS2_PLACEMENT_3D('',#12020,#3733,#3734);
#3367=AXIS2_PLACEMENT_3D('',#12467,#3736,#3737);
#3368=AXIS2_PLACEMENT_3D('',#12920,#3739,#3740);
#3369=AXIS2_PLACEMENT_3D('',#13397,#3742,#3743);
#3370=AXIS2_PLACEMENT_3D('',#13852,#3745,#3746);
#3371=AXIS2_PLACEMENT_3D('',#14323,#3748,#3749);
#3372=AXIS2_PLACEMENT_3D('',#14760,#3751,#3752);
#3373=AXIS2_PLACEMENT_3D('',#15178,#3754,#3755);
#3374=AXIS2_PLACEMENT_3D('',#15631,#3757,#3758);
#3375=AXIS2_PLACEMENT_3D('',#15643,#3760,#3761);
#3376=AXIS2_PLACEMENT_3D('',#15649,#3762,#3763);
#3377=AXIS2_PLACEMENT_3D('',#15835,#3765,#3766);
#3378=AXIS2_PLACEMENT_3D('',#16021,#3768,#3769);
#3379=AXIS2_PLACEMENT_3D('',#16369,#3771,#3772);
#3380=AXIS2_PLACEMENT_3D('',#16393,#3774,#3775);
#3381=AXIS2_PLACEMENT_3D('',#16417,#3777,#3778);
#3382=AXIS2_PLACEMENT_3D('',#16604,#3780,#3781);
#3383=AXIS2_PLACEMENT_3D('',#16952,#3783,#3784);
#3384=AXIS2_PLACEMENT_3D('',#16976,#3786,#3787);
#3385=AXIS2_PLACEMENT_3D('',#17002,#3789,#3790);
#3386=AXIS2_PLACEMENT_3D('',#17188,#3792,#3793);
#3387=AXIS2_PLACEMENT_3D('',#17536,#3795,#3796);
#3388=AXIS2_PLACEMENT_3D('',#17562,#3798,#3799);
#3389=AXIS2_PLACEMENT_3D('',#17586,#3801,#3802);
#3390=AXIS2_PLACEMENT_3D('',#17772,#3804,#3805);
#3391=AXIS2_PLACEMENT_3D('',#18120,#3807,#3808);
#3392=AXIS2_PLACEMENT_3D('',#18144,#3810,#3811);
#3393=AXIS2_PLACEMENT_3D('',#18168,#3813,#3814);
#3394=AXIS2_PLACEMENT_3D('',#18355,#3816,#3817);
#3395=AXIS2_PLACEMENT_3D('',#18703,#3819,#3820);
#3396=AXIS2_PLACEMENT_3D('',#18727,#3822,#3823);
#3397=AXIS2_PLACEMENT_3D('',#18739,#3824,#3825);
#3398=AXIS2_PLACEMENT_3D('',#18748,#3826,#3827);
#3399=AXIS2_PLACEMENT_3D('',#18971,#3828,#3829);
#3400=AXIS2_PLACEMENT_3D('',#20483,#3830,#3831);
#3401=AXIS2_PLACEMENT_3D('',#20484,#3832,#3833);
#3402=AXIS2_PLACEMENT_3D('',#20485,#3834,#3835);
#3403=AXIS2_PLACEMENT_3D('',#20486,#3836,#3837);
#3404=AXIS2_PLACEMENT_3D('',#20498,#3839,#3840);
#3405=AXIS2_PLACEMENT_3D('',#20575,#3841,#3842);
#3406=AXIS2_PLACEMENT_3D('',#20878,#3844,#3845);
#3407=AXIS2_PLACEMENT_3D('',#20983,#3847,#3848);
#3408=AXIS2_PLACEMENT_3D('',#21098,#3849,#3850);
#3409=AXIS2_PLACEMENT_3D('',#21171,#3852,#3853);
#3410=AXIS2_PLACEMENT_3D('',#21252,#3854,#3855);
#3411=AXIS2_PLACEMENT_3D('',#21547,#3857,#3858);
#3412=AXIS2_PLACEMENT_3D('',#21587,#3860,#3861);
#3413=AXIS2_PLACEMENT_3D('',#21688,#3862,#3863);
#3414=AXIS2_PLACEMENT_3D('',#21982,#3864,#3865);
#3415=AXIS2_PLACEMENT_3D('',#22853,#3866,#3867);
#3416=AXIS2_PLACEMENT_3D('',#22866,#3874,#3875);
#3417=AXIS2_PLACEMENT_3D('',#22872,#3879,#3880);
#3418=AXIS2_PLACEMENT_3D('',#22876,#3883,#3884);
#3419=AXIS2_PLACEMENT_3D('',#22880,#3887,#3888);
#3420=AXIS2_PLACEMENT_3D('',#22884,#3891,#3892);
#3421=AXIS2_PLACEMENT_3D('',#22888,#3895,#3896);
#3422=AXIS2_PLACEMENT_3D('',#22890,#3898,#3899);
#3423=AXIS2_PLACEMENT_3D('',#22891,#3900,#3901);
#3424=AXIS2_PLACEMENT_3D('',#22892,#3902,#3903);
#3425=AXIS2_PLACEMENT_3D('',#23008,#3905,#3906);
#3426=AXIS2_PLACEMENT_3D('',#23064,#3907,#3908);
#3427=AXIS2_PLACEMENT_3D('',#23484,#3910,#3911);
#3428=AXIS2_PLACEMENT_3D('',#23931,#3913,#3914);
#3429=AXIS2_PLACEMENT_3D('',#24384,#3916,#3917);
#3430=AXIS2_PLACEMENT_3D('',#24835,#3919,#3920);
#3431=AXIS2_PLACEMENT_3D('',#25318,#3922,#3923);
#3432=AXIS2_PLACEMENT_3D('',#25873,#3925,#3926);
#3433=AXIS2_PLACEMENT_3D('',#26322,#3928,#3929);
#3434=AXIS2_PLACEMENT_3D('',#26773,#3931,#3932);
#3435=AXIS2_PLACEMENT_3D('',#27212,#3934,#3935);
#3436=AXIS2_PLACEMENT_3D('',#27653,#3937,#3938);
#3437=AXIS2_PLACEMENT_3D('',#28132,#3940,#3941);
#3438=AXIS2_PLACEMENT_3D('',#28607,#3943,#3944);
#3439=AXIS2_PLACEMENT_3D('',#29130,#3946,#3947);
#3440=AXIS2_PLACEMENT_3D('',#29583,#3949,#3950);
#3441=AXIS2_PLACEMENT_3D('',#30020,#3952,#3953);
#3442=AXIS2_PLACEMENT_3D('',#30479,#3955,#3956);
#3443=AXIS2_PLACEMENT_3D('',#30940,#3958,#3959);
#3444=AXIS2_PLACEMENT_3D('',#31367,#3961,#3962);
#3445=AXIS2_PLACEMENT_3D('',#31795,#3964,#3965);
#3446=AXIS2_PLACEMENT_3D('',#32196,#3967,#3968);
#3447=AXIS2_PLACEMENT_3D('',#32208,#3970,#3971);
#3448=AXIS2_PLACEMENT_3D('',#32214,#3972,#3973);
#3449=AXIS2_PLACEMENT_3D('',#32400,#3975,#3976);
#3450=AXIS2_PLACEMENT_3D('',#32748,#3978,#3979);
#3451=AXIS2_PLACEMENT_3D('',#33096,#3981,#3982);
#3452=AXIS2_PLACEMENT_3D('',#33444,#3984,#3985);
#3453=AXIS2_PLACEMENT_3D('',#33792,#3987,#3988);
#3454=AXIS2_PLACEMENT_3D('',#34140,#3990,#3991);
#3455=AXIS2_PLACEMENT_3D('',#34488,#3993,#3994);
#3456=AXIS2_PLACEMENT_3D('',#34836,#3996,#3997);
#3457=AXIS2_PLACEMENT_3D('',#35184,#3999,#4000);
#3458=AXIS2_PLACEMENT_3D('',#35532,#4002,#4003);
#3459=AXIS2_PLACEMENT_3D('',#35880,#4005,#4006);
#3460=AXIS2_PLACEMENT_3D('',#36228,#4008,#4009);
#3461=AXIS2_PLACEMENT_3D('',#36579,#4011,#4012);
#3462=AXIS2_PLACEMENT_3D('',#36930,#4014,#4015);
#3463=AXIS2_PLACEMENT_3D('',#37278,#4017,#4018);
#3464=AXIS2_PLACEMENT_3D('',#37629,#4020,#4021);
#3465=AXIS2_PLACEMENT_3D('',#37983,#4023,#4024);
#3466=AXIS2_PLACEMENT_3D('',#38331,#4026,#4027);
#3467=AXIS2_PLACEMENT_3D('',#38679,#4029,#4030);
#3468=AXIS2_PLACEMENT_3D('',#39033,#4032,#4033);
#3469=AXIS2_PLACEMENT_3D('',#39045,#4034,#4035);
#3470=AXIS2_PLACEMENT_3D('',#39054,#4036,#4037);
#3471=AXIS2_PLACEMENT_3D('',#39193,#4038,#4039);
#3472=AXIS2_PLACEMENT_3D('',#40705,#4040,#4041);
#3473=AXIS2_PLACEMENT_3D('',#40706,#4042,#4043);
#3474=AXIS2_PLACEMENT_3D('',#40707,#4044,#4045);
#3475=AXIS2_PLACEMENT_3D('',#40708,#4046,#4047);
#3476=AXIS2_PLACEMENT_3D('',#40709,#4048,#4049);
#3477=AXIS2_PLACEMENT_3D('',#40710,#4050,#4051);
#3478=AXIS2_PLACEMENT_3D('',#40711,#4052,#4053);
#3479=AXIS2_PLACEMENT_3D('',#40712,#4054,#4055);
#3480=AXIS2_PLACEMENT_3D('',#40713,#4056,#4057);
#3481=AXIS2_PLACEMENT_3D('',#40714,#4058,#4059);
#3482=DIRECTION('axis',(0.,0.,1.));
#3483=DIRECTION('refdir',(1.,0.,0.));
#3484=DIRECTION('axis',(0.,0.,1.));
#3485=DIRECTION('refdir',(1.,0.,0.));
#3486=DIRECTION('center_axis',(-1.,0.,0.));
#3487=DIRECTION('ref_axis',(0.,1.,0.));
#3488=DIRECTION('center_axis',(-1.,0.,0.));
#3489=DIRECTION('ref_axis',(0.,1.,0.));
#3490=DIRECTION('',(-1.,0.,0.));
#3491=DIRECTION('center_axis',(-1.,0.,0.));
#3492=DIRECTION('ref_axis',(0.,1.,0.));
#3493=DIRECTION('center_axis',(1.,0.,0.));
#3494=DIRECTION('ref_axis',(0.,1.,0.));
#3495=DIRECTION('center_axis',(1.,0.,0.));
#3496=DIRECTION('ref_axis',(0.,0.,-1.));
#3497=DIRECTION('center_axis',(-1.,0.,0.));
#3498=DIRECTION('ref_axis',(0.,1.22464679914735E-16,1.));
#3499=DIRECTION('center_axis',(0.,-1.,-1.22464679914735E-16));
#3500=DIRECTION('ref_axis',(0.,-1.22464679914735E-16,1.));
#3501=DIRECTION('center_axis',(1.,0.,0.));
#3502=DIRECTION('ref_axis',(0.,1.22464679914735E-16,1.));
#3503=DIRECTION('center_axis',(1.,0.,0.));
#3504=DIRECTION('ref_axis',(0.,0.,-1.));
#3505=DIRECTION('center_axis',(1.,0.,0.));
#3506=DIRECTION('ref_axis',(0.,0.,-1.));
#3507=DIRECTION('',(-1.,0.,0.));
#3508=DIRECTION('center_axis',(1.,0.,0.));
#3509=DIRECTION('ref_axis',(0.,0.,-1.));
#3510=DIRECTION('center_axis',(1.,0.,0.));
#3511=DIRECTION('ref_axis',(0.,0.,-1.));
#3512=DIRECTION('center_axis',(0.,0.,-1.));
#3513=DIRECTION('ref_axis',(1.,0.,0.));
#3514=DIRECTION('center_axis',(0.,0.,1.));
#3515=DIRECTION('ref_axis',(1.,0.,0.));
#3516=DIRECTION('',(0.,0.,-1.));
#3517=DIRECTION('center_axis',(0.,0.,1.));
#3518=DIRECTION('ref_axis',(1.,0.,0.));
#3519=DIRECTION('center_axis',(0.,0.,1.));
#3520=DIRECTION('ref_axis',(1.,0.,0.));
#3521=DIRECTION('center_axis',(1.,-1.22464679914735E-16,0.));
#3522=DIRECTION('ref_axis',(0.,-1.,0.));
#3523=DIRECTION('center_axis',(-7.49879891330929E-33,-1.22464679914735E-16,
1.));
#3524=DIRECTION('ref_axis',(0.,1.,1.22464679914735E-16));
#3525=DIRECTION('axis',(0.,0.,1.));
#3526=DIRECTION('refdir',(1.,0.,0.));
#3527=DIRECTION('center_axis',(-1.,0.,0.));
#3528=DIRECTION('ref_axis',(0.,1.,0.));
#3529=DIRECTION('center_axis',(-1.,0.,0.));
#3530=DIRECTION('ref_axis',(0.,1.,0.));
#3531=DIRECTION('',(-1.,0.,0.));
#3532=DIRECTION('center_axis',(1.,0.,0.));
#3533=DIRECTION('ref_axis',(0.,1.,0.));
#3534=DIRECTION('center_axis',(-1.,0.,0.));
#3535=DIRECTION('ref_axis',(0.,0.,1.));
#3536=DIRECTION('center_axis',(1.,0.,0.));
#3537=DIRECTION('ref_axis',(0.,0.,-1.));
#3538=DIRECTION('center_axis',(1.,0.,0.));
#3539=DIRECTION('ref_axis',(0.,0.,-1.));
#3540=DIRECTION('center_axis',(1.,0.,0.));
#3541=DIRECTION('ref_axis',(0.,0.,-1.));
#3542=DIRECTION('center_axis',(0.,-1.,-1.22464679914735E-16));
#3543=DIRECTION('ref_axis',(0.,-1.22464679914735E-16,1.));
#3544=DIRECTION('center_axis',(1.,0.,0.));
#3545=DIRECTION('ref_axis',(0.,0.,-1.));
#3546=DIRECTION('center_axis',(1.,0.,0.));
#3547=DIRECTION('ref_axis',(0.,0.,-1.));
#3548=DIRECTION('',(-1.,0.,0.));
#3549=DIRECTION('center_axis',(1.,0.,0.));
#3550=DIRECTION('ref_axis',(0.,0.,-1.));
#3551=DIRECTION('center_axis',(1.,0.,0.));
#3552=DIRECTION('ref_axis',(0.,0.,-1.));
#3553=DIRECTION('center_axis',(0.,-1.,-1.22464679914735E-16));
#3554=DIRECTION('ref_axis',(0.,-1.22464679914735E-16,1.));
#3555=DIRECTION('center_axis',(1.,0.,0.));
#3556=DIRECTION('ref_axis',(0.,0.,-1.));
#3557=DIRECTION('axis',(0.,0.,1.));
#3558=DIRECTION('refdir',(1.,0.,0.));
#3559=DIRECTION('center_axis',(0.,0.,1.));
#3560=DIRECTION('ref_axis',(-0.609175761423683,0.793035239881479,0.));
#3561=DIRECTION('',(0.,0.,1.));
#3562=DIRECTION('center_axis',(0.,0.,-1.));
#3563=DIRECTION('ref_axis',(1.,4.24024356072764E-16,0.));
#3564=DIRECTION('center_axis',(0.,0.,1.));
#3565=DIRECTION('ref_axis',(-0.609175761423683,0.793035239881479,0.));
#3566=DIRECTION('',(0.,0.,1.));
#3567=DIRECTION('center_axis',(0.,0.,1.));
#3568=DIRECTION('ref_axis',(-0.609175761423683,0.793035239881479,0.));
#3569=DIRECTION('',(0.,0.,1.));
#3570=DIRECTION('center_axis',(0.,0.,1.));
#3571=DIRECTION('ref_axis',(1.,4.24024356072764E-16,0.));
#3572=DIRECTION('center_axis',(0.,0.,1.));
#3573=DIRECTION('ref_axis',(-0.348605484123622,-0.937269553777853,0.));
#3574=DIRECTION('',(0.,0.,1.));
#3575=DIRECTION('center_axis',(0.,0.,-1.));
#3576=DIRECTION('ref_axis',(1.,0.,0.));
#3577=DIRECTION('center_axis',(0.,0.,1.));
#3578=DIRECTION('ref_axis',(-0.348605484123622,-0.937269553777853,0.));
#3579=DIRECTION('',(0.,0.,1.));
#3580=DIRECTION('center_axis',(0.,0.,1.));
#3581=DIRECTION('ref_axis',(-0.348605484123622,-0.937269553777853,0.));
#3582=DIRECTION('',(0.,0.,1.));
#3583=DIRECTION('center_axis',(0.,0.,-1.));
#3584=DIRECTION('ref_axis',(1.,0.,0.));
#3585=DIRECTION('center_axis',(0.,0.,1.));
#3586=DIRECTION('ref_axis',(-0.348605484123622,-0.937269553777853,0.));
#3587=DIRECTION('center_axis',(0.,0.,1.));
#3588=DIRECTION('ref_axis',(-0.609175761423683,0.793035239881479,0.));
#3589=DIRECTION('center_axis',(0.,0.,-1.));
#3590=DIRECTION('ref_axis',(1.,0.,0.));
#3591=DIRECTION('',(1.,6.00925839494863E-16,0.));
#3592=DIRECTION('',(0.5,-0.866025403784439,0.));
#3593=DIRECTION('',(-0.499999999999999,-0.866025403784439,0.));
#3594=DIRECTION('',(-1.,-7.21111007393836E-16,0.));
#3595=DIRECTION('',(-0.500000000000001,0.866025403784438,0.));
#3596=DIRECTION('',(0.499999999999999,0.866025403784439,0.));
#3597=DIRECTION('center_axis',(0.866025403784438,0.5,0.));
#3598=DIRECTION('ref_axis',(-0.5,0.866025403784438,0.));
#3599=DIRECTION('',(0.,0.,1.));
#3600=DIRECTION('',(-0.5,0.866025403784439,0.));
#3601=DIRECTION('',(0.,0.,1.));
#3602=DIRECTION('center_axis',(0.866025403784439,-0.5,0.));
#3603=DIRECTION('ref_axis',(0.5,0.866025403784439,0.));
#3604=DIRECTION('',(0.499999999999999,0.866025403784439,0.));
#3605=DIRECTION('',(0.,0.,1.));
#3606=DIRECTION('center_axis',(7.21111007393836E-16,-1.,0.));
#3607=DIRECTION('ref_axis',(1.,7.21111007393836E-16,0.));
#3608=DIRECTION('',(1.,7.21111007393836E-16,0.));
#3609=DIRECTION('',(0.,0.,1.));
#3610=DIRECTION('center_axis',(-0.866025403784438,-0.500000000000001,0.));
#3611=DIRECTION('ref_axis',(0.500000000000001,-0.866025403784438,0.));
#3612=DIRECTION('',(0.500000000000001,-0.866025403784438,0.));
#3613=DIRECTION('',(0.,0.,1.));
#3614=DIRECTION('center_axis',(-0.866025403784439,0.499999999999999,0.));
#3615=DIRECTION('ref_axis',(-0.499999999999999,-0.866025403784439,0.));
#3616=DIRECTION('',(-0.499999999999999,-0.866025403784439,0.));
#3617=DIRECTION('',(0.,0.,1.));
#3618=DIRECTION('center_axis',(-6.00925839494863E-16,1.,0.));
#3619=DIRECTION('ref_axis',(-1.,-6.00925839494863E-16,0.));
#3620=DIRECTION('',(-1.,-6.00925839494863E-16,0.));
#3621=DIRECTION('center_axis',(0.,0.,-1.));
#3622=DIRECTION('ref_axis',(1.,0.,0.));
#3623=DIRECTION('axis',(0.,0.,1.));
#3624=DIRECTION('refdir',(1.,0.,0.));
#3625=DIRECTION('center_axis',(1.,0.,0.));
#3626=DIRECTION('ref_axis',(0.,-1.,0.));
#3627=DIRECTION('center_axis',(1.,0.,1.22464679914735E-16));
#3628=DIRECTION('ref_axis',(0.,-1.,0.));
#3629=DIRECTION('',(1.,0.,0.));
#3630=DIRECTION('center_axis',(1.,0.,0.));
#3631=DIRECTION('ref_axis',(0.,-1.,0.));
#3632=DIRECTION('center_axis',(-1.,0.,0.));
#3633=DIRECTION('ref_axis',(0.,-1.,0.));
#3634=DIRECTION('center_axis',(-1.,0.,-1.22464679914735E-16));
#3635=DIRECTION('ref_axis',(0.,0.,1.));
#3636=DIRECTION('center_axis',(1.,0.,1.22464679914735E-16));
#3637=DIRECTION('ref_axis',(-1.22464679914735E-16,2.13056796687593E-46,
1.));
#3638=DIRECTION('center_axis',(-1.49975978266185E-32,-1.,1.22464679914735E-16));
#3639=DIRECTION('ref_axis',(0.,-1.22464679914735E-16,-1.));
#3640=DIRECTION('center_axis',(-1.,0.,-1.22464679914735E-16));
#3641=DIRECTION('ref_axis',(-1.22464679914735E-16,2.13056796687593E-46,
1.));
#3642=DIRECTION('center_axis',(-1.,0.,-1.22464679914735E-16));
#3643=DIRECTION('ref_axis',(-1.22464679914735E-16,2.13056796687593E-46,
1.));
#3644=DIRECTION('center_axis',(-1.,0.,-1.22464679914735E-16));
#3645=DIRECTION('ref_axis',(1.22464679914735E-16,-1.22464679914735E-16,
-1.));
#3646=DIRECTION('center_axis',(-1.,0.,-1.22464679914735E-16));
#3647=DIRECTION('ref_axis',(1.22464679914735E-16,-1.22464679914735E-16,
-1.));
#3648=DIRECTION('',(1.,0.,1.22464679914735E-16));
#3649=DIRECTION('center_axis',(-1.,0.,-1.22464679914735E-16));
#3650=DIRECTION('ref_axis',(1.22464679914735E-16,-1.22464679914735E-16,
-1.));
#3651=DIRECTION('center_axis',(-1.,0.,-1.22464679914735E-16));
#3652=DIRECTION('ref_axis',(1.22464679914735E-16,-1.22464679914735E-16,
-1.));
#3653=DIRECTION('center_axis',(1.22464679914735E-16,-1.22464679914735E-16,
-1.));
#3654=DIRECTION('ref_axis',(-1.,1.258548236767E-48,-1.22464679914735E-16));
#3655=DIRECTION('center_axis',(-1.22464679914735E-16,1.22464679914735E-16,
1.));
#3656=DIRECTION('ref_axis',(-1.,1.258548236767E-48,-1.22464679914735E-16));
#3657=DIRECTION('',(1.22464679914735E-16,-1.22464679914735E-16,-1.));
#3658=DIRECTION('center_axis',(-1.22464679914735E-16,1.22464679914735E-16,
1.));
#3659=DIRECTION('ref_axis',(-1.,1.258548236767E-48,-1.22464679914735E-16));
#3660=DIRECTION('center_axis',(-1.22464679914735E-16,1.22464679914735E-16,
1.));
#3661=DIRECTION('ref_axis',(-1.,1.258548236767E-48,-1.22464679914735E-16));
#3662=DIRECTION('center_axis',(-1.,1.22464679914735E-16,-1.22464679914735E-16));
#3663=DIRECTION('ref_axis',(0.,1.,-1.22464679914735E-16));
#3664=DIRECTION('center_axis',(-1.22464679914735E-16,2.4492935982947E-16,
1.));
#3665=DIRECTION('ref_axis',(0.,-1.,2.4492935982947E-16));
#3666=DIRECTION('axis',(0.,0.,1.));
#3667=DIRECTION('refdir',(1.,0.,0.));
#3668=DIRECTION('center_axis',(-1.,0.,0.));
#3669=DIRECTION('ref_axis',(0.,-1.,0.));
#3670=DIRECTION('center_axis',(-1.,0.,0.));
#3671=DIRECTION('ref_axis',(0.,0.,-1.));
#3672=DIRECTION('center_axis',(1.,0.,0.));
#3673=DIRECTION('ref_axis',(0.,0.,-1.));
#3674=DIRECTION('',(-1.,0.,0.));
#3675=DIRECTION('center_axis',(1.,0.,0.));
#3676=DIRECTION('ref_axis',(0.,0.,-1.));
#3677=DIRECTION('center_axis',(-1.,0.,0.));
#3678=DIRECTION('ref_axis',(0.,0.,1.));
#3679=DIRECTION('center_axis',(1.,0.,0.));
#3680=DIRECTION('ref_axis',(0.,0.,-1.));
#3681=DIRECTION('center_axis',(1.,0.,0.));
#3682=DIRECTION('ref_axis',(0.,0.,-1.));
#3683=DIRECTION('center_axis',(1.,0.,0.));
#3684=DIRECTION('ref_axis',(0.,0.,-1.));
#3685=DIRECTION('',(-1.,0.,0.));
#3686=DIRECTION('center_axis',(1.,0.,0.));
#3687=DIRECTION('ref_axis',(0.,0.,-1.));
#3688=DIRECTION('center_axis',(-1.,0.,0.));
#3689=DIRECTION('ref_axis',(0.,-1.,0.));
#3690=DIRECTION('axis',(0.,0.,1.));
#3691=DIRECTION('refdir',(1.,0.,0.));
#3692=DIRECTION('center_axis',(0.,0.,-1.));
#3693=DIRECTION('ref_axis',(-0.457355310655569,0.889284049005237,0.));
#3694=DIRECTION('',(0.,0.,1.));
#3695=DIRECTION('center_axis',(0.,0.,1.));
#3696=DIRECTION('ref_axis',(1.,-4.0036529262094E-14,0.));
#3697=DIRECTION('center_axis',(0.,0.,-1.));
#3698=DIRECTION('ref_axis',(-0.457355310655569,0.889284049005237,0.));
#3699=DIRECTION('',(0.,0.,1.));
#3700=DIRECTION('center_axis',(0.,0.,-1.));
#3701=DIRECTION('ref_axis',(-0.457355310655569,0.889284049005237,0.));
#3702=DIRECTION('',(0.,0.,1.));
#3703=DIRECTION('center_axis',(0.,0.,-1.));
#3704=DIRECTION('ref_axis',(-0.457355310655569,0.889284049005237,0.));
#3705=DIRECTION('',(0.,0.,1.));
#3706=DIRECTION('center_axis',(0.,0.,-1.));
#3707=DIRECTION('ref_axis',(-0.457355310655569,0.889284049005237,0.));
#3708=DIRECTION('',(0.,0.,1.));
#3709=DIRECTION('center_axis',(0.,0.,-1.));
#3710=DIRECTION('ref_axis',(-0.457355310655569,0.889284049005237,0.));
#3711=DIRECTION('',(0.,0.,1.));
#3712=DIRECTION('center_axis',(0.,0.,-1.));
#3713=DIRECTION('ref_axis',(-0.457355310655569,0.889284049005237,0.));
#3714=DIRECTION('',(0.,0.,1.));
#3715=DIRECTION('center_axis',(0.,0.,-1.));
#3716=DIRECTION('ref_axis',(-0.457355310655569,0.889284049005237,0.));
#3717=DIRECTION('',(0.,0.,1.));
#3718=DIRECTION('center_axis',(0.,0.,-1.));
#3719=DIRECTION('ref_axis',(-0.457355310655569,0.889284049005237,0.));
#3720=DIRECTION('',(0.,0.,1.));
#3721=DIRECTION('center_axis',(0.,0.,-1.));
#3722=DIRECTION('ref_axis',(-0.457355310655569,0.889284049005237,0.));
#3723=DIRECTION('',(0.,0.,1.));
#3724=DIRECTION('center_axis',(0.,0.,-1.));
#3725=DIRECTION('ref_axis',(-0.457355310655569,0.889284049005237,0.));
#3726=DIRECTION('',(0.,0.,1.));
#3727=DIRECTION('center_axis',(0.,0.,-1.));
#3728=DIRECTION('ref_axis',(-0.457355310655569,0.889284049005237,0.));
#3729=DIRECTION('',(0.,0.,1.));
#3730=DIRECTION('center_axis',(0.,0.,-1.));
#3731=DIRECTION('ref_axis',(-0.457355310655569,0.889284049005237,0.));
#3732=DIRECTION('',(0.,0.,1.));
#3733=DIRECTION('center_axis',(0.,0.,-1.));
#3734=DIRECTION('ref_axis',(-0.457355310655569,0.889284049005237,0.));
#3735=DIRECTION('',(0.,0.,1.));
#3736=DIRECTION('center_axis',(0.,0.,-1.));
#3737=DIRECTION('ref_axis',(-0.457355310655569,0.889284049005237,0.));
#3738=DIRECTION('',(0.,0.,1.));
#3739=DIRECTION('center_axis',(0.,0.,-1.));
#3740=DIRECTION('ref_axis',(-0.457355310655569,0.889284049005237,0.));
#3741=DIRECTION('',(0.,0.,1.));
#3742=DIRECTION('center_axis',(0.,0.,-1.));
#3743=DIRECTION('ref_axis',(-0.457355310655569,0.889284049005237,0.));
#3744=DIRECTION('',(0.,0.,1.));
#3745=DIRECTION('center_axis',(0.,0.,-1.));
#3746=DIRECTION('ref_axis',(-0.457355310655569,0.889284049005237,0.));
#3747=DIRECTION('',(0.,0.,1.));
#3748=DIRECTION('center_axis',(0.,0.,-1.));
#3749=DIRECTION('ref_axis',(-0.457355310655569,0.889284049005237,0.));
#3750=DIRECTION('',(0.,0.,1.));
#3751=DIRECTION('center_axis',(0.,0.,-1.));
#3752=DIRECTION('ref_axis',(-0.457355310655569,0.889284049005237,0.));
#3753=DIRECTION('',(0.,0.,1.));
#3754=DIRECTION('center_axis',(0.,0.,-1.));
#3755=DIRECTION('ref_axis',(-0.457355310655569,0.889284049005237,0.));
#3756=DIRECTION('',(0.,0.,1.));
#3757=DIRECTION('center_axis',(0.,0.,-1.));
#3758=DIRECTION('ref_axis',(1.,0.,0.));
#3759=DIRECTION('',(0.,0.,1.));
#3760=DIRECTION('center_axis',(0.,0.,-1.));
#3761=DIRECTION('ref_axis',(1.,0.,0.));
#3762=DIRECTION('center_axis',(0.,0.,-1.));
#3763=DIRECTION('ref_axis',(1.,0.,0.));
#3764=DIRECTION('',(0.,0.,1.));
#3765=DIRECTION('center_axis',(0.,0.,-1.));
#3766=DIRECTION('ref_axis',(1.,0.,0.));
#3767=DIRECTION('',(0.,0.,1.));
#3768=DIRECTION('center_axis',(0.,0.,-1.));
#3769=DIRECTION('ref_axis',(1.,0.,0.));
#3770=DIRECTION('',(0.,0.,1.));
#3771=DIRECTION('center_axis',(0.,0.,-1.));
#3772=DIRECTION('ref_axis',(1.,0.,0.));
#3773=DIRECTION('',(0.,0.,1.));
#3774=DIRECTION('center_axis',(0.,0.,-1.));
#3775=DIRECTION('ref_axis',(1.,0.,0.));
#3776=DIRECTION('',(0.,0.,1.));
#3777=DIRECTION('center_axis',(0.,0.,-1.));
#3778=DIRECTION('ref_axis',(1.,0.,0.));
#3779=DIRECTION('',(0.,0.,1.));
#3780=DIRECTION('center_axis',(0.,0.,-1.));
#3781=DIRECTION('ref_axis',(1.,0.,0.));
#3782=DIRECTION('',(0.,0.,1.));
#3783=DIRECTION('center_axis',(0.,0.,-1.));
#3784=DIRECTION('ref_axis',(1.,0.,0.));
#3785=DIRECTION('',(0.,0.,1.));
#3786=DIRECTION('center_axis',(0.,0.,-1.));
#3787=DIRECTION('ref_axis',(1.,0.,0.));
#3788=DIRECTION('',(0.,0.,1.));
#3789=DIRECTION('center_axis',(0.,0.,-1.));
#3790=DIRECTION('ref_axis',(1.,0.,0.));
#3791=DIRECTION('',(0.,0.,1.));
#3792=DIRECTION('center_axis',(0.,0.,-1.));
#3793=DIRECTION('ref_axis',(1.,0.,0.));
#3794=DIRECTION('',(0.,0.,1.));
#3795=DIRECTION('center_axis',(0.,0.,-1.));
#3796=DIRECTION('ref_axis',(1.,0.,0.));
#3797=DIRECTION('',(0.,0.,1.));
#3798=DIRECTION('center_axis',(0.,0.,-1.));
#3799=DIRECTION('ref_axis',(1.,0.,0.));
#3800=DIRECTION('',(0.,0.,1.));
#3801=DIRECTION('center_axis',(0.,0.,-1.));
#3802=DIRECTION('ref_axis',(1.,0.,0.));
#3803=DIRECTION('',(0.,0.,1.));
#3804=DIRECTION('center_axis',(0.,0.,-1.));
#3805=DIRECTION('ref_axis',(1.,0.,0.));
#3806=DIRECTION('',(0.,0.,1.));
#3807=DIRECTION('center_axis',(0.,0.,-1.));
#3808=DIRECTION('ref_axis',(1.,0.,0.));
#3809=DIRECTION('',(0.,0.,1.));
#3810=DIRECTION('center_axis',(0.,0.,-1.));
#3811=DIRECTION('ref_axis',(1.,0.,0.));
#3812=DIRECTION('',(0.,0.,1.));
#3813=DIRECTION('center_axis',(0.,0.,-1.));
#3814=DIRECTION('ref_axis',(1.,0.,0.));
#3815=DIRECTION('',(0.,0.,1.));
#3816=DIRECTION('center_axis',(0.,0.,-1.));
#3817=DIRECTION('ref_axis',(1.,0.,0.));
#3818=DIRECTION('',(0.,0.,1.));
#3819=DIRECTION('center_axis',(0.,0.,-1.));
#3820=DIRECTION('ref_axis',(1.,0.,0.));
#3821=DIRECTION('',(0.,0.,1.));
#3822=DIRECTION('center_axis',(0.,0.,-1.));
#3823=DIRECTION('ref_axis',(1.,0.,0.));
#3824=DIRECTION('center_axis',(0.,0.,-1.));
#3825=DIRECTION('ref_axis',(1.,0.,0.));
#3826=DIRECTION('center_axis',(0.,0.,-1.));
#3827=DIRECTION('ref_axis',(-0.457355310655569,0.889284049005237,0.));
#3828=DIRECTION('center_axis',(0.,0.,-1.));
#3829=DIRECTION('ref_axis',(1.,-4.0036529262094E-14,0.));
#3830=DIRECTION('center_axis',(0.,0.,1.));
#3831=DIRECTION('ref_axis',(1.,0.,0.));
#3832=DIRECTION('center_axis',(0.,0.,1.));
#3833=DIRECTION('ref_axis',(1.,0.,0.));
#3834=DIRECTION('axis',(0.,0.,1.));
#3835=DIRECTION('refdir',(1.,0.,0.));
#3836=DIRECTION('center_axis',(-1.22464679914735E-16,1.22464679914735E-16,
1.));
#3837=DIRECTION('ref_axis',(0.609173230228443,-0.793037184231007,1.71721249579884E-16));
#3838=DIRECTION('',(-1.22464679914735E-16,1.22464679914735E-16,1.));
#3839=DIRECTION('center_axis',(1.22464679914735E-16,-1.22464679914735E-16,
-1.));
#3840=DIRECTION('ref_axis',(-1.,-4.24024356072764E-16,-1.22464679914735E-16));
#3841=DIRECTION('center_axis',(-1.22464679914735E-16,1.22464679914735E-16,
1.));
#3842=DIRECTION('ref_axis',(0.609173230228443,-0.793037184231007,1.71721249579884E-16));
#3843=DIRECTION('',(-1.22464679914735E-16,1.22464679914735E-16,1.));
#3844=DIRECTION('center_axis',(-1.22464679914735E-16,1.22464679914735E-16,
1.));
#3845=DIRECTION('ref_axis',(0.609173230228443,-0.793037184231007,1.71721249579884E-16));
#3846=DIRECTION('',(-1.22464679914735E-16,1.22464679914735E-16,1.));
#3847=DIRECTION('center_axis',(-1.22464679914735E-16,1.22464679914735E-16,
1.));
#3848=DIRECTION('ref_axis',(-1.,-4.24024356072764E-16,-1.22464679914735E-16));
#3849=DIRECTION('center_axis',(-1.22464679914735E-16,1.22464679914735E-16,
1.));
#3850=DIRECTION('ref_axis',(0.348694007966754,0.93723662370187,-7.20756830521819E-17));
#3851=DIRECTION('',(-1.22464679914735E-16,1.22464679914735E-16,1.));
#3852=DIRECTION('center_axis',(1.22464679914735E-16,-1.22464679914735E-16,
-1.));
#3853=DIRECTION('ref_axis',(-1.,1.258548236767E-48,-1.22464679914735E-16));
#3854=DIRECTION('center_axis',(-1.22464679914735E-16,1.22464679914735E-16,
1.));
#3855=DIRECTION('ref_axis',(0.348694007966754,0.93723662370187,-7.20756830521819E-17));
#3856=DIRECTION('',(-1.22464679914735E-16,1.22464679914735E-16,1.));
#3857=DIRECTION('center_axis',(-1.22464679914735E-16,1.22464679914735E-16,
1.));
#3858=DIRECTION('ref_axis',(0.348694007966754,0.93723662370187,-7.20756830521819E-17));
#3859=DIRECTION('',(-1.22464679914735E-16,1.22464679914735E-16,1.));
#3860=DIRECTION('center_axis',(1.22464679914735E-16,-1.22464679914735E-16,
-1.));
#3861=DIRECTION('ref_axis',(-1.,1.258548236767E-48,-1.22464679914735E-16));
#3862=DIRECTION('center_axis',(-1.22464679914735E-16,1.22464679914735E-16,
1.));
#3863=DIRECTION('ref_axis',(0.348694007966754,0.93723662370187,-7.20756830521819E-17));
#3864=DIRECTION('center_axis',(-1.22464679914735E-16,1.22464679914735E-16,
1.));
#3865=DIRECTION('ref_axis',(0.609173230228443,-0.793037184231007,1.71721249579884E-16));
#3866=DIRECTION('center_axis',(1.22464679914735E-16,-1.22464679914735E-16,
-1.));
#3867=DIRECTION('ref_axis',(-1.,1.258548236767E-48,-1.22464679914735E-16));
#3868=DIRECTION('',(-1.,-6.00925839494863E-16,-1.22464679914735E-16));
#3869=DIRECTION('',(-0.5,0.866025403784439,-1.67289863829858E-16));
#3870=DIRECTION('',(0.499999999999999,0.866025403784439,-4.48251839151231E-17));
#3871=DIRECTION('',(1.,7.21111007393836E-16,1.22464679914735E-16));
#3872=DIRECTION('',(0.500000000000001,-0.866025403784438,1.67289863829858E-16));
#3873=DIRECTION('',(-0.499999999999999,-0.866025403784439,4.48251839151232E-17));
#3874=DIRECTION('center_axis',(-0.866025403784438,-0.5,-4.48251839151229E-17));
#3875=DIRECTION('ref_axis',(0.5,-0.866025403784438,1.67289863829858E-16));
#3876=DIRECTION('',(-1.22464679914735E-16,1.22464679914735E-16,1.));
#3877=DIRECTION('',(0.5,-0.866025403784439,1.67289863829858E-16));
#3878=DIRECTION('',(-1.22464679914735E-16,1.22464679914735E-16,1.));
#3879=DIRECTION('center_axis',(-0.866025403784439,0.5,-1.67289863829858E-16));
#3880=DIRECTION('ref_axis',(-0.5,-0.866025403784439,4.4825183915123E-17));
#3881=DIRECTION('',(-0.499999999999999,-0.866025403784439,4.48251839151231E-17));
#3882=DIRECTION('',(-1.22464679914735E-16,1.22464679914735E-16,1.));
#3883=DIRECTION('center_axis',(-7.21111007393836E-16,1.,-1.22464679914735E-16));
#3884=DIRECTION('ref_axis',(-1.,-7.21111007393836E-16,-1.22464679914735E-16));
#3885=DIRECTION('',(-1.,-7.21111007393836E-16,-1.22464679914735E-16));
#3886=DIRECTION('',(-1.22464679914735E-16,1.22464679914735E-16,1.));
#3887=DIRECTION('center_axis',(0.866025403784438,0.500000000000001,4.48251839151229E-17));
#3888=DIRECTION('ref_axis',(-0.500000000000001,0.866025403784438,-1.67289863829858E-16));
#3889=DIRECTION('',(-0.500000000000001,0.866025403784438,-1.67289863829858E-16));
#3890=DIRECTION('',(-1.22464679914735E-16,1.22464679914735E-16,1.));
#3891=DIRECTION('center_axis',(0.866025403784439,-0.499999999999999,1.67289863829858E-16));
#3892=DIRECTION('ref_axis',(0.499999999999999,0.866025403784439,-4.48251839151232E-17));
#3893=DIRECTION('',(0.499999999999999,0.866025403784439,-4.48251839151232E-17));
#3894=DIRECTION('',(-1.22464679914735E-16,1.22464679914735E-16,1.));
#3895=DIRECTION('center_axis',(6.00925839494863E-16,-1.,1.22464679914735E-16));
#3896=DIRECTION('ref_axis',(1.,6.00925839494863E-16,1.22464679914735E-16));
#3897=DIRECTION('',(1.,6.00925839494863E-16,1.22464679914735E-16));
#3898=DIRECTION('center_axis',(1.22464679914735E-16,-1.22464679914735E-16,
-1.));
#3899=DIRECTION('ref_axis',(-1.,1.258548236767E-48,-1.22464679914735E-16));
#3900=DIRECTION('axis',(0.,0.,1.));
#3901=DIRECTION('refdir',(1.,0.,0.));
#3902=DIRECTION('center_axis',(1.22464679914735E-16,-1.22464679914735E-16,
-1.));
#3903=DIRECTION('ref_axis',(0.457379984296263,-0.88927135901543,1.64917225715414E-16));
#3904=DIRECTION('',(-1.22464679914735E-16,1.22464679914735E-16,1.));
#3905=DIRECTION('center_axis',(-1.22464679914735E-16,1.22464679914735E-16,
1.));
#3906=DIRECTION('ref_axis',(-1.,4.0036529262094E-14,-1.2246467991474E-16));
#3907=DIRECTION('center_axis',(1.22464679914735E-16,-1.22464679914735E-16,
-1.));
#3908=DIRECTION('ref_axis',(0.457379984296263,-0.88927135901543,1.64917225715414E-16));
#3909=DIRECTION('',(-1.22464679914735E-16,1.22464679914735E-16,1.));
#3910=DIRECTION('center_axis',(1.22464679914735E-16,-1.22464679914735E-16,
-1.));
#3911=DIRECTION('ref_axis',(0.457379984296263,-0.88927135901543,1.64917225715414E-16));
#3912=DIRECTION('',(-1.22464679914735E-16,1.22464679914735E-16,1.));
#3913=DIRECTION('center_axis',(1.22464679914735E-16,-1.22464679914735E-16,
-1.));
#3914=DIRECTION('ref_axis',(0.457379984296263,-0.88927135901543,1.64917225715414E-16));
#3915=DIRECTION('',(-1.22464679914735E-16,1.22464679914735E-16,1.));
#3916=DIRECTION('center_axis',(1.22464679914735E-16,-1.22464679914735E-16,
-1.));
#3917=DIRECTION('ref_axis',(0.457379984296263,-0.88927135901543,1.64917225715414E-16));
#3918=DIRECTION('',(-1.22464679914735E-16,1.22464679914735E-16,1.));
#3919=DIRECTION('center_axis',(1.22464679914735E-16,-1.22464679914735E-16,
-1.));
#3920=DIRECTION('ref_axis',(0.457379984296263,-0.88927135901543,1.64917225715414E-16));
#3921=DIRECTION('',(-1.22464679914735E-16,1.22464679914735E-16,1.));
#3922=DIRECTION('center_axis',(1.22464679914735E-16,-1.22464679914735E-16,
-1.));
#3923=DIRECTION('ref_axis',(0.457379984296263,-0.88927135901543,1.64917225715414E-16));
#3924=DIRECTION('',(-1.22464679914735E-16,1.22464679914735E-16,1.));
#3925=DIRECTION('center_axis',(1.22464679914735E-16,-1.22464679914735E-16,
-1.));
#3926=DIRECTION('ref_axis',(0.457379984296263,-0.88927135901543,1.64917225715414E-16));
#3927=DIRECTION('',(-1.22464679914735E-16,1.22464679914735E-16,1.));
#3928=DIRECTION('center_axis',(1.22464679914735E-16,-1.22464679914735E-16,
-1.));
#3929=DIRECTION('ref_axis',(0.457379984296263,-0.88927135901543,1.64917225715414E-16));
#3930=DIRECTION('',(-1.22464679914735E-16,1.22464679914735E-16,1.));
#3931=DIRECTION('center_axis',(1.22464679914735E-16,-1.22464679914735E-16,
-1.));
#3932=DIRECTION('ref_axis',(0.457379984296263,-0.88927135901543,1.64917225715414E-16));
#3933=DIRECTION('',(-1.22464679914735E-16,1.22464679914735E-16,1.));
#3934=DIRECTION('center_axis',(1.22464679914735E-16,-1.22464679914735E-16,
-1.));
#3935=DIRECTION('ref_axis',(0.457379984296263,-0.88927135901543,1.64917225715414E-16));
#3936=DIRECTION('',(-1.22464679914735E-16,1.22464679914735E-16,1.));
#3937=DIRECTION('center_axis',(1.22464679914735E-16,-1.22464679914735E-16,
-1.));
#3938=DIRECTION('ref_axis',(0.457379984296263,-0.88927135901543,1.64917225715414E-16));
#3939=DIRECTION('',(-1.22464679914735E-16,1.22464679914735E-16,1.));
#3940=DIRECTION('center_axis',(1.22464679914735E-16,-1.22464679914735E-16,
-1.));
#3941=DIRECTION('ref_axis',(0.457379984296263,-0.88927135901543,1.64917225715414E-16));
#3942=DIRECTION('',(-1.22464679914735E-16,1.22464679914735E-16,1.));
#3943=DIRECTION('center_axis',(1.22464679914735E-16,-1.22464679914735E-16,
-1.));
#3944=DIRECTION('ref_axis',(0.457379984296263,-0.88927135901543,1.64917225715414E-16));
#3945=DIRECTION('',(-1.22464679914735E-16,1.22464679914735E-16,1.));
#3946=DIRECTION('center_axis',(1.22464679914735E-16,-1.22464679914735E-16,
-1.));
#3947=DIRECTION('ref_axis',(0.457379984296263,-0.88927135901543,1.64917225715414E-16));
#3948=DIRECTION('',(-1.22464679914735E-16,1.22464679914735E-16,1.));
#3949=DIRECTION('center_axis',(1.22464679914735E-16,-1.22464679914735E-16,
-1.));
#3950=DIRECTION('ref_axis',(0.457379984296263,-0.88927135901543,1.64917225715414E-16));
#3951=DIRECTION('',(-1.22464679914735E-16,1.22464679914735E-16,1.));
#3952=DIRECTION('center_axis',(1.22464679914735E-16,-1.22464679914735E-16,
-1.));
#3953=DIRECTION('ref_axis',(0.457379984296263,-0.88927135901543,1.64917225715414E-16));
#3954=DIRECTION('',(-1.22464679914735E-16,1.22464679914735E-16,1.));
#3955=DIRECTION('center_axis',(1.22464679914735E-16,-1.22464679914735E-16,
-1.));
#3956=DIRECTION('ref_axis',(0.457379984296263,-0.88927135901543,1.64917225715414E-16));
#3957=DIRECTION('',(-1.22464679914735E-16,1.22464679914735E-16,1.));
#3958=DIRECTION('center_axis',(1.22464679914735E-16,-1.22464679914735E-16,
-1.));
#3959=DIRECTION('ref_axis',(0.457379984296263,-0.88927135901543,1.64917225715414E-16));
#3960=DIRECTION('',(-1.22464679914735E-16,1.22464679914735E-16,1.));
#3961=DIRECTION('center_axis',(1.22464679914735E-16,-1.22464679914735E-16,
-1.));
#3962=DIRECTION('ref_axis',(0.457379984296263,-0.88927135901543,1.64917225715414E-16));
#3963=DIRECTION('',(-1.22464679914735E-16,1.22464679914735E-16,1.));
#3964=DIRECTION('center_axis',(1.22464679914735E-16,-1.22464679914735E-16,
-1.));
#3965=DIRECTION('ref_axis',(0.457379984296263,-0.88927135901543,1.64917225715414E-16));
#3966=DIRECTION('',(-1.22464679914735E-16,1.22464679914735E-16,1.));
#3967=DIRECTION('center_axis',(1.22464679914735E-16,-1.22464679914735E-16,
-1.));
#3968=DIRECTION('ref_axis',(-1.,1.258548236767E-48,-1.22464679914735E-16));
#3969=DIRECTION('',(-1.22464679914735E-16,1.22464679914735E-16,1.));
#3970=DIRECTION('center_axis',(1.22464679914735E-16,-1.22464679914735E-16,
-1.));
#3971=DIRECTION('ref_axis',(-1.,1.258548236767E-48,-1.22464679914735E-16));
#3972=DIRECTION('center_axis',(1.22464679914735E-16,-1.22464679914735E-16,
-1.));
#3973=DIRECTION('ref_axis',(-1.,1.258548236767E-48,-1.22464679914735E-16));
#3974=DIRECTION('',(-1.22464679914735E-16,1.22464679914735E-16,1.));
#3975=DIRECTION('center_axis',(1.22464679914735E-16,-1.22464679914735E-16,
-1.));
#3976=DIRECTION('ref_axis',(-1.,1.258548236767E-48,-1.22464679914735E-16));
#3977=DIRECTION('',(-1.22464679914735E-16,1.22464679914735E-16,1.));
#3978=DIRECTION('center_axis',(1.22464679914735E-16,-1.22464679914735E-16,
-1.));
#3979=DIRECTION('ref_axis',(-1.,1.258548236767E-48,-1.22464679914735E-16));
#3980=DIRECTION('',(-1.22464679914735E-16,1.22464679914735E-16,1.));
#3981=DIRECTION('center_axis',(1.22464679914735E-16,-1.22464679914735E-16,
-1.));
#3982=DIRECTION('ref_axis',(-1.,1.258548236767E-48,-1.22464679914735E-16));
#3983=DIRECTION('',(-1.22464679914735E-16,1.22464679914735E-16,1.));
#3984=DIRECTION('center_axis',(1.22464679914735E-16,-1.22464679914735E-16,
-1.));
#3985=DIRECTION('ref_axis',(-1.,1.258548236767E-48,-1.22464679914735E-16));
#3986=DIRECTION('',(-1.22464679914735E-16,1.22464679914735E-16,1.));
#3987=DIRECTION('center_axis',(1.22464679914735E-16,-1.22464679914735E-16,
-1.));
#3988=DIRECTION('ref_axis',(-1.,1.258548236767E-48,-1.22464679914735E-16));
#3989=DIRECTION('',(-1.22464679914735E-16,1.22464679914735E-16,1.));
#3990=DIRECTION('center_axis',(1.22464679914735E-16,-1.22464679914735E-16,
-1.));
#3991=DIRECTION('ref_axis',(-1.,1.258548236767E-48,-1.22464679914735E-16));
#3992=DIRECTION('',(-1.22464679914735E-16,1.22464679914735E-16,1.));
#3993=DIRECTION('center_axis',(1.22464679914735E-16,-1.22464679914735E-16,
-1.));
#3994=DIRECTION('ref_axis',(-1.,1.258548236767E-48,-1.22464679914735E-16));
#3995=DIRECTION('',(-1.22464679914735E-16,1.22464679914735E-16,1.));
#3996=DIRECTION('center_axis',(1.22464679914735E-16,-1.22464679914735E-16,
-1.));
#3997=DIRECTION('ref_axis',(-1.,1.258548236767E-48,-1.22464679914735E-16));
#3998=DIRECTION('',(-1.22464679914735E-16,1.22464679914735E-16,1.));
#3999=DIRECTION('center_axis',(1.22464679914735E-16,-1.22464679914735E-16,
-1.));
#4000=DIRECTION('ref_axis',(-1.,1.258548236767E-48,-1.22464679914735E-16));
#4001=DIRECTION('',(-1.22464679914735E-16,1.22464679914735E-16,1.));
#4002=DIRECTION('center_axis',(1.22464679914735E-16,-1.22464679914735E-16,
-1.));
#4003=DIRECTION('ref_axis',(-1.,1.258548236767E-48,-1.22464679914735E-16));
#4004=DIRECTION('',(-1.22464679914735E-16,1.22464679914735E-16,1.));
#4005=DIRECTION('center_axis',(1.22464679914735E-16,-1.22464679914735E-16,
-1.));
#4006=DIRECTION('ref_axis',(-1.,1.258548236767E-48,-1.22464679914735E-16));
#4007=DIRECTION('',(-1.22464679914735E-16,1.22464679914735E-16,1.));
#4008=DIRECTION('center_axis',(1.22464679914735E-16,-1.22464679914735E-16,
-1.));
#4009=DIRECTION('ref_axis',(-1.,1.258548236767E-48,-1.22464679914735E-16));
#4010=DIRECTION('',(-1.22464679914735E-16,1.22464679914735E-16,1.));
#4011=DIRECTION('center_axis',(1.22464679914735E-16,-1.22464679914735E-16,
-1.));
#4012=DIRECTION('ref_axis',(-1.,1.258548236767E-48,-1.22464679914735E-16));
#4013=DIRECTION('',(-1.22464679914735E-16,1.22464679914735E-16,1.));
#4014=DIRECTION('center_axis',(1.22464679914735E-16,-1.22464679914735E-16,
-1.));
#4015=DIRECTION('ref_axis',(-1.,1.258548236767E-48,-1.22464679914735E-16));
#4016=DIRECTION('',(-1.22464679914735E-16,1.22464679914735E-16,1.));
#4017=DIRECTION('center_axis',(1.22464679914735E-16,-1.22464679914735E-16,
-1.));
#4018=DIRECTION('ref_axis',(-1.,1.258548236767E-48,-1.22464679914735E-16));
#4019=DIRECTION('',(-1.22464679914735E-16,1.22464679914735E-16,1.));
#4020=DIRECTION('center_axis',(1.22464679914735E-16,-1.22464679914735E-16,
-1.));
#4021=DIRECTION('ref_axis',(-1.,1.258548236767E-48,-1.22464679914735E-16));
#4022=DIRECTION('',(-1.22464679914735E-16,1.22464679914735E-16,1.));
#4023=DIRECTION('center_axis',(1.22464679914735E-16,-1.22464679914735E-16,
-1.));
#4024=DIRECTION('ref_axis',(-1.,1.258548236767E-48,-1.22464679914735E-16));
#4025=DIRECTION('',(-1.22464679914735E-16,1.22464679914735E-16,1.));
#4026=DIRECTION('center_axis',(1.22464679914735E-16,-1.22464679914735E-16,
-1.));
#4027=DIRECTION('ref_axis',(-1.,1.258548236767E-48,-1.22464679914735E-16));
#4028=DIRECTION('',(-1.22464679914735E-16,1.22464679914735E-16,1.));
#4029=DIRECTION('center_axis',(1.22464679914735E-16,-1.22464679914735E-16,
-1.));
#4030=DIRECTION('ref_axis',(-1.,1.258548236767E-48,-1.22464679914735E-16));
#4031=DIRECTION('',(-1.22464679914735E-16,1.22464679914735E-16,1.));
#4032=DIRECTION('center_axis',(1.22464679914735E-16,-1.22464679914735E-16,
-1.));
#4033=DIRECTION('ref_axis',(-1.,1.258548236767E-48,-1.22464679914735E-16));
#4034=DIRECTION('center_axis',(1.22464679914735E-16,-1.22464679914735E-16,
-1.));
#4035=DIRECTION('ref_axis',(-1.,1.258548236767E-48,-1.22464679914735E-16));
#4036=DIRECTION('center_axis',(1.22464679914735E-16,-1.22464679914735E-16,
-1.));
#4037=DIRECTION('ref_axis',(0.457379984296263,-0.88927135901543,1.64917225715414E-16));
#4038=DIRECTION('center_axis',(1.22464679914735E-16,-1.22464679914735E-16,
-1.));
#4039=DIRECTION('ref_axis',(-1.,4.0036529262094E-14,-1.2246467991474E-16));
#4040=DIRECTION('center_axis',(-1.22464679914735E-16,1.22464679914735E-16,
1.));
#4041=DIRECTION('ref_axis',(-1.,1.258548236767E-48,-1.22464679914735E-16));
#4042=DIRECTION('center_axis',(-1.22464679914735E-16,1.22464679914735E-16,
1.));
#4043=DIRECTION('ref_axis',(-1.,1.258548236767E-48,-1.22464679914735E-16));
#4044=DIRECTION('',(0.,0.,1.));
#4045=DIRECTION('',(1.,0.,0.));
#4046=DIRECTION('',(0.,0.,1.));
#4047=DIRECTION('',(1.,0.,0.));
#4048=DIRECTION('',(0.,0.,1.));
#4049=DIRECTION('',(1.,0.,0.));
#4050=DIRECTION('',(0.,0.,1.));
#4051=DIRECTION('',(1.,0.,0.));
#4052=DIRECTION('',(0.,0.,1.));
#4053=DIRECTION('',(1.,0.,0.));
#4054=DIRECTION('',(0.,0.,1.));
#4055=DIRECTION('',(1.,0.,0.));
#4056=DIRECTION('',(0.,0.,1.));
#4057=DIRECTION('',(1.,0.,0.));
#4058=DIRECTION('',(0.,0.,1.));
#4059=DIRECTION('',(1.,0.,0.));
#4060=CARTESIAN_POINT('',(0.,0.,0.));
#4061=CARTESIAN_POINT('',(0.,0.,0.));
#4062=CARTESIAN_POINT('Origin',(67.3063659679149,0.,0.));
#4063=CARTESIAN_POINT('',(14.3512997641764,-1.08063175605657,1.32339222111166E-16));
#4064=CARTESIAN_POINT('Origin',(14.3512997641764,0.,0.));
#4065=CARTESIAN_POINT('',(9.05579314380255,-1.08063175605657,-1.32339222111166E-16));
#4066=CARTESIAN_POINT('',(67.3063659679149,-1.08063175605657,1.32339222111166E-16));
#4067=CARTESIAN_POINT('Origin',(9.05579314380255,0.,0.));
#4068=CARTESIAN_POINT('Origin',(9.05579314380255,0.,0.));
#4069=CARTESIAN_POINT('Origin',(13.3512997641764,0.,0.));
#4070=CARTESIAN_POINT('',(14.3512997641764,-1.42213764307597E-16,1.16126351211314));
#4071=CARTESIAN_POINT('Origin',(14.3512997641764,0.,0.));
#4072=CARTESIAN_POINT('',(13.3512997641764,-2.64678444222332E-16,2.16126351211314));
#4073=CARTESIAN_POINT('Origin',(13.3512997641764,-1.42213764307597E-16,
1.16126351211314));
#4074=CARTESIAN_POINT('Origin',(13.3512997641764,0.,0.));
#4075=CARTESIAN_POINT('Origin',(14.3512997641764,0.,0.));
#4076=CARTESIAN_POINT('Origin',(10.3469384954313,0.,0.));
#4077=CARTESIAN_POINT('',(6.34257722668614,-2.64678444222332E-16,2.16126351211314));
#4078=CARTESIAN_POINT('',(10.3469384954313,-2.64678444222332E-16,2.16126351211314));
#4079=CARTESIAN_POINT('',(6.34257722668614,2.16126351211314,2.64678444222332E-16));
#4080=CARTESIAN_POINT('Origin',(6.34257722668614,0.,0.));
#4081=CARTESIAN_POINT('Origin',(6.34257722668614,0.,0.));
#4082=CARTESIAN_POINT('Origin',(3.53951905042299,8.32667268468867E-16,0.));
#4083=CARTESIAN_POINT('',(1.03951905042299,5.26505568682029E-16,0.));
#4084=CARTESIAN_POINT('Origin',(3.53951905042299,8.32667268468867E-16,0.));
#4085=CARTESIAN_POINT('',(1.03951905042299,5.26505568682029E-16,-2.5056326762531));
#4086=CARTESIAN_POINT('',(1.03951905042299,1.13882896825571E-15,0.));
#4087=CARTESIAN_POINT('Origin',(3.53951905042299,8.32667268468867E-16,-2.5056326762531));
#4088=CARTESIAN_POINT('Origin',(3.53951905042299,6.93889390390723E-16,0.));
#4089=CARTESIAN_POINT('Origin',(3.53951905042299,0.,0.));
#4090=CARTESIAN_POINT('',(0.,2.1673303378108E-16,-1.3684555315672E-47));
#4091=CARTESIAN_POINT('Origin',(3.53951905042299,0.,0.));
#4092=CARTESIAN_POINT('',(0.,0.,0.));
#4093=CARTESIAN_POINT('Origin',(67.3063659679149,0.,0.));
#4094=CARTESIAN_POINT('',(67.3063659679149,-1.08063175605657,-1.32339222111166E-16));
#4095=CARTESIAN_POINT('Origin',(67.3063659679149,0.,0.));
#4096=CARTESIAN_POINT('',(14.3512997641764,-1.08063175605657,-1.32339222111166E-16));
#4097=CARTESIAN_POINT('',(67.3063659679149,-1.08063175605657,1.32339222111166E-16));
#4098=CARTESIAN_POINT('Origin',(14.3512997641764,0.,0.));
#4099=CARTESIAN_POINT('Origin',(14.3512997641764,0.,-2.90634189295526));
#4100=CARTESIAN_POINT('',(14.3512997641764,-3.55924229643552E-16,2.90634189295526));
#4101=CARTESIAN_POINT('Origin',(14.3512997641764,0.,0.));
#4102=CARTESIAN_POINT('Origin',(15.3512997641764,0.,0.));
#4103=CARTESIAN_POINT('',(15.3512997641764,-4.78388909558288E-16,3.90634189295526));
#4104=CARTESIAN_POINT('Origin',(15.3512997641764,0.,0.));
#4105=CARTESIAN_POINT('Origin',(15.3512997641764,-3.55924229643552E-16,
2.90634189295526));
#4106=CARTESIAN_POINT('Origin',(40.8288328660457,0.,0.));
#4107=CARTESIAN_POINT('',(66.3063659679149,-4.78388909558288E-16,3.90634189295527));
#4108=CARTESIAN_POINT('Origin',(66.3063659679149,0.,0.));
#4109=CARTESIAN_POINT('',(40.8288328660457,-4.78388909558288E-16,3.90634189295527));
#4110=CARTESIAN_POINT('Origin',(66.3063659679149,0.,0.));
#4111=CARTESIAN_POINT('',(67.3063659679149,-3.55924229643552E-16,2.90634189295526));
#4112=CARTESIAN_POINT('Origin',(67.3063659679149,0.,0.));
#4113=CARTESIAN_POINT('Origin',(66.3063659679149,-3.55924229643553E-16,
2.90634189295527));
#4114=CARTESIAN_POINT('Origin',(67.3063659679149,0.,0.));
#4115=CARTESIAN_POINT('',(0.,0.,0.));
#4116=CARTESIAN_POINT('Origin',(3.53951905042299,8.32667268468867E-16,-7.60421172358873));
#4117=CARTESIAN_POINT('',(4.47947725029973,-1.22365337513712,-5.21861712256713));
#4118=CARTESIAN_POINT('',(4.47963717506662,-1.22386353108345,-5.17715717872024));
#4119=CARTESIAN_POINT('',(4.47947725029973,-1.22365337513712,-7.60421172358873));
#4120=CARTESIAN_POINT('',(3.93803289228021,1.49064942821852,-5.));
#4121=CARTESIAN_POINT('Ctrl Pts',(4.4796371750665,-1.22386353108354,-5.17715717872025));
#4122=CARTESIAN_POINT('Ctrl Pts',(4.57769164024551,-1.15008922561236,-5.17082834295539));
#4123=CARTESIAN_POINT('Ctrl Pts',(5.037452302555,-0.710090958920894,-5.13813772861957));
#4124=CARTESIAN_POINT('Ctrl Pts',(5.26960331241849,0.567664116001651,-5.07908533571283));
#4125=CARTESIAN_POINT('Ctrl Pts',(4.43184313015523,1.35863299878938,-5.02636177857094));
#4126=CARTESIAN_POINT('Ctrl Pts',(3.93803289228021,1.49064942821852,-5.));
#4127=CARTESIAN_POINT('',(3.14100461111498,1.49064926849444,-5.00001191998211));
#4128=CARTESIAN_POINT('Origin',(3.53951905042299,8.32667268468867E-16,-5.));
#4129=CARTESIAN_POINT('Ctrl Pts',(4.47947725029973,-1.22365337513712,-5.21861712256713));
#4130=CARTESIAN_POINT('Ctrl Pts',(4.52496896162635,-1.18870858770246,-5.21565841989965));
#4131=CARTESIAN_POINT('Ctrl Pts',(4.56856576972649,-1.15118013128263,-5.21269971723217));
#4132=CARTESIAN_POINT('Ctrl Pts',(4.60996354210099,-1.11130445434014,-5.20974101456469));
#4133=CARTESIAN_POINT('Ctrl Pts',(4.65133326839928,-1.07145579228783,-5.2067843163529));
#4134=CARTESIAN_POINT('Ctrl Pts',(4.69050653598573,-1.02926342304973,-5.20382761814111));
#4135=CARTESIAN_POINT('Ctrl Pts',(4.72721349442131,-0.985002998825653,-5.20087091992933));
#4136=CARTESIAN_POINT('Ctrl Pts',(4.763909812257,-0.940755404797399,-5.19791507880415));
#4137=CARTESIAN_POINT('Ctrl Pts',(4.79814090596258,-0.894441347385724,-5.19495923767897));
#4138=CARTESIAN_POINT('Ctrl Pts',(4.82967642307994,-0.846370458947444,-5.1920033965538));
#4139=CARTESIAN_POINT('Ctrl Pts',(4.86208679747809,-0.79696598949994,-5.18896555458115));
#4140=CARTESIAN_POINT('Ctrl Pts',(4.89164943609571,-0.745706210110481,-5.18592771260849));
#4141=CARTESIAN_POINT('Ctrl Pts',(4.91816268873484,-0.692957948610356,-5.18288987063584));
#4142=CARTESIAN_POINT('Ctrl Pts',(4.9439922730574,-0.641569848974656,-5.17993036217948));
#4143=CARTESIAN_POINT('Ctrl Pts',(4.96692770978701,-0.5887696387494,-5.17697085372312));
#4144=CARTESIAN_POINT('Ctrl Pts',(4.986831041283,-0.534917751727157,-5.17401134526675));
#4145=CARTESIAN_POINT('Ctrl Pts',(5.00752458742015,-0.478927803064939,-5.17093433653596));
#4146=CARTESIAN_POINT('Ctrl Pts',(5.0249399808018,-0.421801497406585,-5.16785732780516));
#4147=CARTESIAN_POINT('Ctrl Pts',(5.03897984230443,-0.363959247183371,-5.16478031907437));
#4148=CARTESIAN_POINT('Ctrl Pts',(5.05301970380706,-0.306116996960155,-5.16170331034357));
#4149=CARTESIAN_POINT('Ctrl Pts',(5.06368399482257,-0.247559432113643,-5.15862630161278));
#4150=CARTESIAN_POINT('Ctrl Pts',(5.07093548192274,-0.188713309897771,-5.15554929288199));
#4151=CARTESIAN_POINT('Ctrl Pts',(5.07794803979793,-0.131806108372223,-5.1525736685019));
#4152=CARTESIAN_POINT('Ctrl Pts',(5.08179867841453,-0.0743909914451671,
-5.14959804412181));
#4153=CARTESIAN_POINT('Ctrl Pts',(5.08242705471315,-0.0168490444052572,
-5.14662241974172));
#4154=CARTESIAN_POINT('Ctrl Pts',(5.08305431454027,0.0405906646226169,-5.14365208232074));
#4155=CARTESIAN_POINT('Ctrl Pts',(5.08047067165934,0.0981562413468887,-5.14068174489977));
#4156=CARTESIAN_POINT('Ctrl Pts',(5.07466750694301,0.155461302079316,-5.13771140747879));
#4157=CARTESIAN_POINT('Ctrl Pts',(5.06887011499728,0.21270935788678,-5.13474402483807));
#4158=CARTESIAN_POINT('Ctrl Pts',(5.05985959973971,0.26969689719103,-5.13177664219734));
#4159=CARTESIAN_POINT('Ctrl Pts',(5.04767935517533,0.326039100675548,-5.12880925955662));
#4160=CARTESIAN_POINT('Ctrl Pts',(5.03550658389236,0.382346734973937,-5.12584369757601));
#4161=CARTESIAN_POINT('Ctrl Pts',(5.02016804863226,0.438009311985927,-5.1228781355954));
#4162=CARTESIAN_POINT('Ctrl Pts',(5.00175846772087,0.492650876889871,-5.1199125736148));
#4163=CARTESIAN_POINT('Ctrl Pts',(4.9833531648314,0.547279744176552,-5.11694770077205));
#4164=CARTESIAN_POINT('Ctrl Pts',(4.96187839901806,0.600887578659077,-5.1139828279293));
#4165=CARTESIAN_POINT('Ctrl Pts',(4.93747847740791,0.653114416089551,-5.11101795508655));
#4166=CARTESIAN_POINT('Ctrl Pts',(4.91305752876829,0.705386260846979,-5.10805052721639));
#4167=CARTESIAN_POINT('Ctrl Pts',(4.88570660610911,0.756274258325724,-5.10508309934622));
#4168=CARTESIAN_POINT('Ctrl Pts',(4.85561728494828,0.805440523613895,-5.10211567147606));
#4169=CARTESIAN_POINT('Ctrl Pts',(4.82551583682365,0.854626604487657,-5.09914704763706));
#4170=CARTESIAN_POINT('Ctrl Pts',(4.79267408416198,0.902089140669927,-5.09617842379807));
#4171=CARTESIAN_POINT('Ctrl Pts',(4.75732677699548,0.947519572937856,-5.09320979995907));
#4172=CARTESIAN_POINT('Ctrl Pts',(4.72191366575164,0.99303458046536,-5.09023564960141));
#4173=CARTESIAN_POINT('Ctrl Pts',(4.68398602059646,1.03650953100728,-5.08726149924375));
#4174=CARTESIAN_POINT('Ctrl Pts',(4.64381804905404,1.07767004301988,-5.08428734888609));
#4175=CARTESIAN_POINT('Ctrl Pts',(4.60859793147866,1.11376044083883,-5.08167955164711));
#4176=CARTESIAN_POINT('Ctrl Pts',(4.57165616602179,1.14807187402944,-5.07907175440814));
#4177=CARTESIAN_POINT('Ctrl Pts',(4.53319812916631,1.1804452077364,-5.07646395716916));
#4178=CARTESIAN_POINT('Ctrl Pts',(4.48959378809824,1.21715061445732,-5.07350719469395));
#4179=CARTESIAN_POINT('Ctrl Pts',(4.443859421242,1.25151535266286,-5.07055043221873));
#4180=CARTESIAN_POINT('Ctrl Pts',(4.39627754539696,1.28328246356363,-5.06759366974352));
#4181=CARTESIAN_POINT('Ctrl Pts',(4.34877801436647,1.31499459855583,-5.06464202421784));
#4182=CARTESIAN_POINT('Ctrl Pts',(4.2994377530913,1.34411773663457,-5.06169037869217));
#4183=CARTESIAN_POINT('Ctrl Pts',(4.24857211196857,1.37043524323948,-5.05873873316649));
#4184=CARTESIAN_POINT('Ctrl Pts',(4.19775517201174,1.39672755222125,-5.05578991368557));
#4185=CARTESIAN_POINT('Ctrl Pts',(4.14541621046131,1.42021930978951,-5.05284109420466));
#4186=CARTESIAN_POINT('Ctrl Pts',(4.09189772583826,1.44073828259905,-5.04989227472374));
#4187=CARTESIAN_POINT('Ctrl Pts',(4.03840939328758,1.46124569511204,-5.04694511659439));
#4188=CARTESIAN_POINT('Ctrl Pts',(3.9837433454879,1.47878345424846,-5.04399795846504));
#4189=CARTESIAN_POINT('Ctrl Pts',(3.92826264938041,1.49322718106443,-5.04105080033569));
#4190=CARTESIAN_POINT('Ctrl Pts',(3.87279134964832,1.50766846164796,-5.03810414134579));
#4191=CARTESIAN_POINT('Ctrl Pts',(3.81650618504884,1.51901661846979,-5.03515748235589));
#4192=CARTESIAN_POINT('Ctrl Pts',(3.75978377510704,1.52719758088463,-5.03221082336599));
#4193=CARTESIAN_POINT('Ctrl Pts',(3.70300925473477,1.53538605908509,-5.02926145730373));
#4194=CARTESIAN_POINT('Ctrl Pts',(3.64579720902174,1.54040145688831,-5.02631209124146));
#4195=CARTESIAN_POINT('Ctrl Pts',(3.58853130954693,1.54222138438538,-5.0233627251792));
#4196=CARTESIAN_POINT('Ctrl Pts',(3.53123779596041,1.54404218946723,-5.02041193690713));
#4197=CARTESIAN_POINT('Ctrl Pts',(3.4738909038836,1.54266446818855,-5.01746114863506));
#4198=CARTESIAN_POINT('Ctrl Pts',(3.41687297221943,1.53811798620954,-5.01451036036299));
#4199=CARTESIAN_POINT('Ctrl Pts',(3.3597517542207,1.53356326840989,-5.01155422682328));
#4200=CARTESIAN_POINT('Ctrl Pts',(3.30296120866352,1.5258284006299,-5.00859809328357));
#4201=CARTESIAN_POINT('Ctrl Pts',(3.24687598530104,1.51499473148788,-5.00564195974387));
#4202=CARTESIAN_POINT('Ctrl Pts',(3.21127068834397,1.50811705526926,-5.00376527982328));
#4203=CARTESIAN_POINT('Ctrl Pts',(3.17594943093811,1.49999151658249,-5.00188859990269));
#4204=CARTESIAN_POINT('Ctrl Pts',(3.14100461111498,1.49064926849444,-5.00001191998211));
#4205=CARTESIAN_POINT('Origin',(3.53951905042299,8.32667268468867E-16,-7.60421172358873));
#4206=CARTESIAN_POINT('',(4.47947725029973,-1.22365337513712,-5.718702116292));
#4207=CARTESIAN_POINT('',(4.47947725029973,-1.22365337513712,-5.6770722010002));
#4208=CARTESIAN_POINT('',(4.47947725029973,-1.22365337513712,-7.60421172358873));
#4209=CARTESIAN_POINT('',(1.99678610450128,-0.000229152999684354,-5.35421171051895));
#4210=CARTESIAN_POINT('Ctrl Pts',(4.47947725029973,-1.22365337513712,-5.6770722010002));
#4211=CARTESIAN_POINT('Ctrl Pts',(4.52512102745272,-1.18859177723691,-5.6741124623146));
#4212=CARTESIAN_POINT('Ctrl Pts',(4.5688116981735,-1.15096420156402,-5.671152723629));
#4213=CARTESIAN_POINT('Ctrl Pts',(4.61025595191897,-1.11102272153849,-5.6681929849434));
#4214=CARTESIAN_POINT('Ctrl Pts',(4.65173647123993,-1.07104629093168,-5.66523065635408));
#4215=CARTESIAN_POINT('Ctrl Pts',(4.69096626732107,-1.02875227044639,-5.66226832776476));
#4216=CARTESIAN_POINT('Ctrl Pts',(4.7276881578121,-0.984430379583121,-5.65930599917544));
#4217=CARTESIAN_POINT('Ctrl Pts',(4.76442431086838,-0.940091274359376,-5.65634252003521));
#4218=CARTESIAN_POINT('Ctrl Pts',(4.79865030417651,-0.893723147399871,-5.65337904089497));
#4219=CARTESIAN_POINT('Ctrl Pts',(4.83015066651991,-0.845647108155074,-5.65041556175474));
#4220=CARTESIAN_POINT('Ctrl Pts',(4.86171249899614,-0.797477252830152,-5.64744629965067));
#4221=CARTESIAN_POINT('Ctrl Pts',(4.89053780680758,-0.747593276385191,-5.64447703754659));
#4222=CARTESIAN_POINT('Ctrl Pts',(4.91645618892747,-0.696342671826952,-5.64150777544252));
#4223=CARTESIAN_POINT('Ctrl Pts',(4.94213395443559,-0.645567858803961,-5.63856607886255));
#4224=CARTESIAN_POINT('Ctrl Pts',(4.96495844566623,-0.593452185264546,-5.63562438228257));
#4225=CARTESIAN_POINT('Ctrl Pts',(4.98481162376582,-0.540350235902651,-5.6326826857026));
#4226=CARTESIAN_POINT('Ctrl Pts',(5.00485343793378,-0.486743735435651,-5.62971303843008));
#4227=CARTESIAN_POINT('Ctrl Pts',(5.02195056381987,-0.431908927050247,-5.62674339115755));
#4228=CARTESIAN_POINT('Ctrl Pts',(5.03595542839796,-0.376200965805698,-5.62377374388503));
#4229=CARTESIAN_POINT('Ctrl Pts',(5.04993555413197,-0.320591409694572,-5.62080934233556));
#4230=CARTESIAN_POINT('Ctrl Pts',(5.0608341342622,-0.264112263761363,-5.61784494078608));
#4231=CARTESIAN_POINT('Ctrl Pts',(5.06855262957362,-0.20713597908089,-5.6148805392366));
#4232=CARTESIAN_POINT('Ctrl Pts',(5.07626350804143,-0.150215920313976,-5.61191906304784));
#4233=CARTESIAN_POINT('Ctrl Pts',(5.08080044975292,-0.0928002090382206,
-5.60895758685909));
#4234=CARTESIAN_POINT('Ctrl Pts',(5.08211585109736,-0.0352719513098852,
-5.60599611067033));
#4235=CARTESIAN_POINT('Ctrl Pts',(5.08343046125446,0.02222170433362,-5.60303641574968));
#4236=CARTESIAN_POINT('Ctrl Pts',(5.08152736026662,0.0798272519015085,-5.60007672082902));
#4237=CARTESIAN_POINT('Ctrl Pts',(5.07641092133383,0.13715821932413,-5.59711702590837));
#4238=CARTESIAN_POINT('Ctrl Pts',(5.07129558832057,0.194476794644151,-5.59415797072649));
#4239=CARTESIAN_POINT('Ctrl Pts',(5.06296834276969,0.251520388464657,-5.59119891554461));
#4240=CARTESIAN_POINT('Ctrl Pts',(5.05148550847944,0.307906527557052,-5.58823986036274));
#4241=CARTESIAN_POINT('Ctrl Pts',(5.03999228093245,0.364343702448172,-5.58527812690306));
#4242=CARTESIAN_POINT('Ctrl Pts',(5.02533786080861,0.42012172111455,-5.58231639344338));
#4243=CARTESIAN_POINT('Ctrl Pts',(5.00762968441671,0.474868577981904,-5.5793546599837));
#4244=CARTESIAN_POINT('Ctrl Pts',(4.9899140057136,0.529638629104231,-5.57639167174512));
#4245=CARTESIAN_POINT('Ctrl Pts',(4.96914217909774,0.583376159735024,-5.57342868350654));
#4246=CARTESIAN_POINT('Ctrl Pts',(4.94547043890925,0.635727687940012,-5.57046569526795));
#4247=CARTESIAN_POINT('Ctrl Pts',(4.92175318439951,0.68817987390206,-5.56749701000847));
#4248=CARTESIAN_POINT('Ctrl Pts',(4.89512511611778,0.739240268107272,-5.56452832474899));
#4249=CARTESIAN_POINT('Ctrl Pts',(4.86578877829008,0.788579488031072,-5.56155963948951));
#4250=CARTESIAN_POINT('Ctrl Pts',(4.83956118434086,0.83269027764405,-5.5589055429896));
#4251=CARTESIAN_POINT('Ctrl Pts',(4.81116967362603,0.875425510514394,-5.55625144648969));
#4252=CARTESIAN_POINT('Ctrl Pts',(4.780786696453,0.916571672548917,-5.55359734998977));
#4253=CARTESIAN_POINT('Ctrl Pts',(4.7467782835908,0.962627582678985,-5.55062655456604));
#4254=CARTESIAN_POINT('Ctrl Pts',(4.71013248018302,1.00688382228577,-5.5476557591423));
#4255=CARTESIAN_POINT('Ctrl Pts',(4.67106669050714,1.04902284923637,-5.54468496371856));
#4256=CARTESIAN_POINT('Ctrl Pts',(4.63206995983055,1.09108738443712,-5.54171941995263));
#4257=CARTESIAN_POINT('Ctrl Pts',(4.59066208558193,1.13104175687353,-5.53875387618669));
#4258=CARTESIAN_POINT('Ctrl Pts',(4.54710170338979,1.16860010159181,-5.53578833242076));
#4259=CARTESIAN_POINT('Ctrl Pts',(4.50358435587312,1.20612134123674,-5.53282571840904));
#4260=CARTESIAN_POINT('Ctrl Pts',(4.45791910652903,1.24125090469248,-5.52986310439732));
#4261=CARTESIAN_POINT('Ctrl Pts',(4.41040129674942,1.27373981371136,-5.5269004903856));
#4262=CARTESIAN_POINT('Ctrl Pts',(4.36291215771501,1.30620911994893,-5.52393966392159));
#4263=CARTESIAN_POINT('Ctrl Pts',(4.31357310338658,1.33604063673605,-5.52097883745757));
#4264=CARTESIAN_POINT('Ctrl Pts',(4.262710643379,1.36302711633986,-5.51801801099355));
#4265=CARTESIAN_POINT('Ctrl Pts',(4.21185931345673,1.39000769057023,-5.51505783243864));
#4266=CARTESIAN_POINT('Ctrl Pts',(4.15948569983316,1.41414421965574,-5.51209765388373));
#4267=CARTESIAN_POINT('Ctrl Pts',(4.10594129811614,1.43527517825616,-5.50913747532882));
#4268=CARTESIAN_POINT('Ctrl Pts',(4.05234884212578,1.45642510117083,-5.50617464011467));
#4269=CARTESIAN_POINT('Ctrl Pts',(3.99758398388154,1.47456387091719,-5.50321180490052));
#4270=CARTESIAN_POINT('Ctrl Pts',(3.94201732753734,1.48957850982081,-5.50024896968638));
#4271=CARTESIAN_POINT('Ctrl Pts',(3.88642732768093,1.50459945636339,-5.49728488978729));
#4272=CARTESIAN_POINT('Ctrl Pts',(3.83003536888944,1.51649354672025,-5.49432080988821));
#4273=CARTESIAN_POINT('Ctrl Pts',(3.77322316025061,1.52519880312361,-5.49135672998913));
#4274=CARTESIAN_POINT('Ctrl Pts',(3.71630234984157,1.53392070042648,-5.48838698397828));
#4275=CARTESIAN_POINT('Ctrl Pts',(3.65896020465046,1.53944153217191,-5.48541723796742));
#4276=CARTESIAN_POINT('Ctrl Pts',(3.60158350752301,1.54175127798387,-5.48244749195657));
#4277=CARTESIAN_POINT('Ctrl Pts',(3.55047795868461,1.54380857359876,-5.47980233273003));
#4278=CARTESIAN_POINT('Ctrl Pts',(3.49934528115122,1.54331910966274,-5.47715717350348));
#4279=CARTESIAN_POINT('Ctrl Pts',(3.44845565257208,1.54031050686926,-5.47451201427694));
#4280=CARTESIAN_POINT('Ctrl Pts',(3.39129979441924,1.53693144360425,-5.47154114673938));
#4281=CARTESIAN_POINT('Ctrl Pts',(3.3342138916778,1.53035977644368,-5.46857027920183));
#4282=CARTESIAN_POINT('Ctrl Pts',(3.27758271527957,1.52060460223282,-5.46559941166427));
#4283=CARTESIAN_POINT('Ctrl Pts',(3.22105127320109,1.51086660805822,-5.46263377618213));
#4284=CARTESIAN_POINT('Ctrl Pts',(3.16497347722393,1.49795632296522,-5.45966814069998));
#4285=CARTESIAN_POINT('Ctrl Pts',(3.10973002638419,1.48193467967241,-5.45670250521784));
#4286=CARTESIAN_POINT('Ctrl Pts',(3.05454093042656,1.4659288003212,-5.45373978767012));
#4287=CARTESIAN_POINT('Ctrl Pts',(3.00018505098282,1.44681777278669,-5.4507770701224));
#4288=CARTESIAN_POINT('Ctrl Pts',(2.94703217859048,1.42471341213106,-5.44781435257468));
#4289=CARTESIAN_POINT('Ctrl Pts',(2.8939111695424,1.40262230228996,-5.44485341107565));
#4290=CARTESIAN_POINT('Ctrl Pts',(2.84199221804376,1.37754161619727,-5.44189246957662));
#4291=CARTESIAN_POINT('Ctrl Pts',(2.79162712720225,1.34963205029415,-5.43893152807759));
#4292=CARTESIAN_POINT('Ctrl Pts',(2.74127286679701,1.32172848602371,-5.43597122329513));
#4293=CARTESIAN_POINT('Ctrl Pts',(2.69247225908117,1.29099750223447,-5.43301091851268));
#4294=CARTESIAN_POINT('Ctrl Pts',(2.6455524033983,1.25764567108841,-5.43005061373022));
#4295=CARTESIAN_POINT('Ctrl Pts',(2.59859018328914,1.22426372622673,-5.42708763605775));
#4296=CARTESIAN_POINT('Ctrl Pts',(2.55351253468013,1.18825650726338,-5.42412465838528));
#4297=CARTESIAN_POINT('Ctrl Pts',(2.51061628248063,1.14987307739617,-5.42116168071281));
#4298=CARTESIAN_POINT('Ctrl Pts',(2.46770187824625,1.11147340514596,-5.41819744922279));
#4299=CARTESIAN_POINT('Ctrl Pts',(2.42697108034768,1.07069588606239,-5.41523321773276));
#4300=CARTESIAN_POINT('Ctrl Pts',(2.38868401791696,1.0278267013251,-5.41226898624274));
#4301=CARTESIAN_POINT('Ctrl Pts',(2.35032360023518,0.984875382320805,-5.40929907549891));
#4302=CARTESIAN_POINT('Ctrl Pts',(2.31441660015544,0.939824798144525,-5.40632916475507));
#4303=CARTESIAN_POINT('Ctrl Pts',(2.28118236144417,0.892993716198393,-5.40335925401124));
#4304=CARTESIAN_POINT('Ctrl Pts',(2.25159302035572,0.851298738037958,-5.40071506219553));
#4305=CARTESIAN_POINT('Ctrl Pts',(2.22412184802125,0.808193041144038,-5.39807087037983));
#4306=CARTESIAN_POINT('Ctrl Pts',(2.19889289039257,0.763917861449834,-5.39542667856413));
#4307=CARTESIAN_POINT('Ctrl Pts',(2.1694007361956,0.712161049065484,-5.39233567044945));
#4308=CARTESIAN_POINT('Ctrl Pts',(2.14285864125366,0.658604878470103,-5.38924466233477));
#4309=CARTESIAN_POINT('Ctrl Pts',(2.11947982028678,0.603603831063202,-5.38615365422009));
#4310=CARTESIAN_POINT('Ctrl Pts',(2.09616542177511,0.548754344015884,-5.38307116365777));
#4311=CARTESIAN_POINT('Ctrl Pts',(2.07599713401881,0.492468323152804,-5.37998867309545));
#4312=CARTESIAN_POINT('Ctrl Pts',(2.05914207527831,0.435124133393559,-5.37690618253314));
#4313=CARTESIAN_POINT('Ctrl Pts',(2.04231496635934,0.377875034366083,-5.37382880349624));
#4314=CARTESIAN_POINT('Ctrl Pts',(2.02879030435349,0.319571690885604,-5.37075142445933));
#4315=CARTESIAN_POINT('Ctrl Pts',(2.01868679289945,0.260611290000743,-5.36767404542243));
#4316=CARTESIAN_POINT('Ctrl Pts',(2.00860191294967,0.201759615766563,-5.3646023412641));
#4317=CARTESIAN_POINT('Ctrl Pts',(2.00192571204157,0.142253746948874,-5.36153063710577));
#4318=CARTESIAN_POINT('Ctrl Pts',(1.9987263078915,0.0825028760850183,-5.35845893294744));
#4319=CARTESIAN_POINT('Ctrl Pts',(1.99725171501102,0.054963933005107,-5.35704319649454));
#4320=CARTESIAN_POINT('Ctrl Pts',(1.99651497203302,0.027373102629171,-5.35562746004163));
#4321=CARTESIAN_POINT('Ctrl Pts',(1.99651906740702,-0.000228938216534968,
-5.35421172358873));
#4322=CARTESIAN_POINT('Ctrl Pts',(1.99901526745067,-0.000230945958973693,
-5.35421160141548));
#4323=CARTESIAN_POINT('Ctrl Pts',(1.99878308421294,-0.245946535663003,-5.34158818189409));
#4324=CARTESIAN_POINT('Ctrl Pts',(2.16986900897196,-1.00442940714747,-5.30260298380174));
#4325=CARTESIAN_POINT('Ctrl Pts',(3.24055550621135,-1.73347751710041,-5.24358484290335));
#4326=CARTESIAN_POINT('Ctrl Pts',(4.16926105443531,-1.45738459198171,-5.19719012152633));
#4327=CARTESIAN_POINT('Ctrl Pts',(4.4796371750665,-1.22386353108354,-5.17715717872025));
#4328=CARTESIAN_POINT('',(1.99651909233433,-0.00035963648524883,-5.39578827645238));
#4329=CARTESIAN_POINT('Ctrl Pts',(1.99651909233452,-0.0003596372777212,
-5.39578827641127));
#4330=CARTESIAN_POINT('Ctrl Pts',(1.99652355962509,-0.0195262520735117,
-5.39479395094767));
#4331=CARTESIAN_POINT('Ctrl Pts',(1.99688513508193,-0.0386883289920865,
-5.39379962548406));
#4332=CARTESIAN_POINT('Ctrl Pts',(1.99760339341755,-0.0578368972324017,
-5.39280530002046));
#4333=CARTESIAN_POINT('Ctrl Pts',(1.99974937102273,-0.115048065662224,-5.3898345023682));
#4334=CARTESIAN_POINT('Ctrl Pts',(2.00508825750452,-0.172258466379416,-5.38686370471594));
#4335=CARTESIAN_POINT('Ctrl Pts',(2.01361936247661,-0.229083265048165,-5.38389290706369));
#4336=CARTESIAN_POINT('Ctrl Pts',(2.02213538638427,-0.285807610322849,-5.38092736110988));
#4337=CARTESIAN_POINT('Ctrl Pts',(2.03383235103549,-0.342147195438881,-5.37796181515608));
#4338=CARTESIAN_POINT('Ctrl Pts',(2.04865765425814,-0.397720124491333,-5.37499626920227));
#4339=CARTESIAN_POINT('Ctrl Pts',(2.06346831097628,-0.453238150845048,-5.37203365302883));
#4340=CARTESIAN_POINT('Ctrl Pts',(2.08140104899805,-0.507990520864456,-5.36907103685538));
#4341=CARTESIAN_POINT('Ctrl Pts',(2.10235215788664,-0.561605130850327,-5.36610842068194));
#4342=CARTESIAN_POINT('Ctrl Pts',(2.12329062533932,-0.615187390965849,-5.36314759208559));
#4343=CARTESIAN_POINT('Ctrl Pts',(2.14724366403913,-0.667632767584206,-5.36018676348925));
#4344=CARTESIAN_POINT('Ctrl Pts',(2.17405830089212,-0.718586071038539,-5.35722593489291));
#4345=CARTESIAN_POINT('Ctrl Pts',(2.20086706968364,-0.769528223973896,-5.35426575423837));
#4346=CARTESIAN_POINT('Ctrl Pts',(2.23053595067948,-0.818978491176606,-5.35130557358383));
#4347=CARTESIAN_POINT('Ctrl Pts',(2.26286556636343,-0.866605378265437,-5.34834539292929));
#4348=CARTESIAN_POINT('Ctrl Pts',(2.29522419602285,-0.914275007753285,-5.34538255568243));
#4349=CARTESIAN_POINT('Ctrl Pts',(2.33024803934686,-0.960117554562589,-5.34241971843557));
#4350=CARTESIAN_POINT('Ctrl Pts',(2.36769457816158,-1.00383086534,-5.33945688118871));
#4351=CARTESIAN_POINT('Ctrl Pts',(2.40515684780633,-1.04756253954122,-5.33649279929039));
#4352=CARTESIAN_POINT('Ctrl Pts',(2.44504348135292,-1.08916281683413,-5.33352871739207));
#4353=CARTESIAN_POINT('Ctrl Pts',(2.48707405043502,-1.12836542042032,-5.33056463549375));
#4354=CARTESIAN_POINT('Ctrl Pts',(2.52918496361848,-1.16764296227228,-5.32759488756468));
#4355=CARTESIAN_POINT('Ctrl Pts',(2.57344760042178,-1.20451333669098,-5.32462513963562));
#4356=CARTESIAN_POINT('Ctrl Pts',(2.61954806545789,-1.2387503327234,-5.32165539170656));
#4357=CARTESIAN_POINT('Ctrl Pts',(2.66060956316622,-1.26924508658379,-5.31901024924025));
#4358=CARTESIAN_POINT('Ctrl Pts',(2.70312842199546,-1.29765114353574,-5.31636510677394));
#4359=CARTESIAN_POINT('Ctrl Pts',(2.74686587636044,-1.32383909356408,-5.31371996430764));
#4360=CARTESIAN_POINT('Ctrl Pts',(2.79598933941203,-1.35325193466999,-5.31074908819936));
#4361=CARTESIAN_POINT('Ctrl Pts',(2.8468538816937,-1.37998776674441,-5.30777821209108));
#4362=CARTESIAN_POINT('Ctrl Pts',(2.89913649611857,-1.40383730686378,-5.3048073359828));
#4363=CARTESIAN_POINT('Ctrl Pts',(2.95132703607727,-1.42764484576153,-5.30184169185909));
#4364=CARTESIAN_POINT('Ctrl Pts',(3.00493022098378,-1.44857596748968,-5.29887604773538));
#4365=CARTESIAN_POINT('Ctrl Pts',(3.05959720111394,-1.46646650781932,-5.29591040361166));
#4366=CARTESIAN_POINT('Ctrl Pts',(3.11421039439706,-1.48433944564459,-5.29294767738549));
#4367=CARTESIAN_POINT('Ctrl Pts',(3.16988481632705,-1.49917756835214,-5.28998495115932));
#4368=CARTESIAN_POINT('Ctrl Pts',(3.22625195985338,-1.51086489467657,-5.28702222493315));
#4369=CARTESIAN_POINT('Ctrl Pts',(3.28258531370008,-1.52254521495125,-5.284061274734));
#4370=CARTESIAN_POINT('Ctrl Pts',(3.33961005679031,-1.53107837754764,-5.28110032453484));
#4371=CARTESIAN_POINT('Ctrl Pts',(3.39694500041986,-1.53639891963829,-5.27813937433569));
#4372=CARTESIAN_POINT('Ctrl Pts',(3.45426761498812,-1.5417183176223,-5.27517906084662));
#4373=CARTESIAN_POINT('Ctrl Pts',(3.511899779116,-1.54382641869227,-5.27221874735755));
#4374=CARTESIAN_POINT('Ctrl Pts',(3.5694548646447,-1.54270957961208,-5.26925843386848));
#4375=CARTESIAN_POINT('Ctrl Pts',(3.62706191594448,-1.54159173215177,-5.26629544754916));
#4376=CARTESIAN_POINT('Ctrl Pts',(3.68459122742742,-1.53724313542495,-5.26333246122985));
#4377=CARTESIAN_POINT('Ctrl Pts',(3.74165724076404,-1.52970230829585,-5.26036947491054));
#4378=CARTESIAN_POINT('Ctrl Pts',(3.79874740179333,-1.52215829023811,-5.2574052347927));
#4379=CARTESIAN_POINT('Ctrl Pts',(3.85537336070937,-1.51141944510768,-5.25444099467487));
#4380=CARTESIAN_POINT('Ctrl Pts',(3.91115896138416,-1.49757563300849,-5.25147675455704));
#4381=CARTESIAN_POINT('Ctrl Pts',(3.96705144023782,-1.48370529791039,-5.24850683532879));
#4382=CARTESIAN_POINT('Ctrl Pts',(4.02209984393975,-1.46671826238209,-5.24553691610055));
#4383=CARTESIAN_POINT('Ctrl Pts',(4.07594335058692,-1.44675428812001,-5.24256699687231));
#4384=CARTESIAN_POINT('Ctrl Pts',(4.12388029109525,-1.4289803371628,-5.23992287411314));
#4385=CARTESIAN_POINT('Ctrl Pts',(4.17086221813424,-1.40884756517063,-5.23727875135398));
#4386=CARTESIAN_POINT('Ctrl Pts',(4.21665074612344,-1.38648536475429,-5.23463462859482));
#4387=CARTESIAN_POINT('Ctrl Pts',(4.26800422218038,-1.36140535510795,-5.23166915010562));
#4388=CARTESIAN_POINT('Ctrl Pts',(4.31807087215149,-1.33341541556237,-5.22870367161642));
#4389=CARTESIAN_POINT('Ctrl Pts',(4.36650003494377,-1.30267089137703,-5.22573819312721));
#4390=CARTESIAN_POINT('Ctrl Pts',(4.40526471622146,-1.27806171764032,-5.22336450294052));
#4391=CARTESIAN_POINT('Ctrl Pts',(4.4429804336582,-1.25168866909262,-5.22099081275382));
#4392=CARTESIAN_POINT('Ctrl Pts',(4.47947725029973,-1.22365337513712,-5.21861712256713));
#4393=CARTESIAN_POINT('Ctrl Pts',(4.47947725029973,-1.22365337513712,-5.718702116292));
#4394=CARTESIAN_POINT('Ctrl Pts',(4.5250506460368,-1.18864584123114,-5.71573178326587));
#4395=CARTESIAN_POINT('Ctrl Pts',(4.56859375641112,-1.15114421804424,-5.71276145023973));
#4396=CARTESIAN_POINT('Ctrl Pts',(4.60983854390703,-1.1114248431037,-5.7097911172136));
#4397=CARTESIAN_POINT('Ctrl Pts',(4.6128215099069,-1.10855220022742,-5.70957629243299));
#4398=CARTESIAN_POINT('Ctrl Pts',(4.61579247143402,-1.10566797149909,-5.70936146765238));
#4399=CARTESIAN_POINT('Ctrl Pts',(4.61875133531101,-1.10277226808412,-5.70914664287176));
#4400=CARTESIAN_POINT('Ctrl Pts',(4.65965884843631,-1.062737974389,-5.70617660170126));
#4401=CARTESIAN_POINT('Ctrl Pts',(4.69842089249096,-1.02034104388721,-5.70320656053075));
#4402=CARTESIAN_POINT('Ctrl Pts',(4.73475305844049,-0.975840492128923,-5.70023651936025));
#4403=CARTESIAN_POINT('Ctrl Pts',(4.77102103844435,-0.931418556933201,-5.69727172519047));
#4404=CARTESIAN_POINT('Ctrl Pts',(4.80486733375244,-0.884900777484445,-5.6943069310207));
#4405=CARTESIAN_POINT('Ctrl Pts',(4.83604459506597,-0.836582639126709,-5.69134213685092));
#4406=CARTESIAN_POINT('Ctrl Pts',(4.8671910827755,-0.788312193324169,-5.68838026908962));
#4407=CARTESIAN_POINT('Ctrl Pts',(4.89567347497013,-0.738245345429881,-5.68541840132832));
#4408=CARTESIAN_POINT('Ctrl Pts',(4.92128602087865,-0.686708846133332,-5.68245653356702));
#4409=CARTESIAN_POINT('Ctrl Pts',(4.94688314864507,-0.635203370580891,-5.67949644877951));
#4410=CARTESIAN_POINT('Ctrl Pts',(4.96961362320494,-0.582230463341924,-5.676536363992));
#4411=CARTESIAN_POINT('Ctrl Pts',(4.98931732760889,-0.528141984194405,-5.67357627920449));
#4412=CARTESIAN_POINT('Ctrl Pts',(5.00901675787319,-0.474065237952958,-5.67061683652038));
#4413=CARTESIAN_POINT('Ctrl Pts',(5.02569054325441,-0.418873889913193,-5.66765739383628));
#4414=CARTESIAN_POINT('Ctrl Pts',(5.03922730215849,-0.362938231213574,-5.66469795115218));
#4415=CARTESIAN_POINT('Ctrl Pts',(5.05277628077117,-0.306952079079415,-5.66173583696247));
#4416=CARTESIAN_POINT('Ctrl Pts',(5.06318245047086,-0.250220781394763,-5.65877372277277));
#4417=CARTESIAN_POINT('Ctrl Pts',(5.07038515182195,-0.193126848437895,-5.65581160858307));
#4418=CARTESIAN_POINT('Ctrl Pts',(5.07759089676128,-0.136008789751712,-5.65284824271632));
#4419=CARTESIAN_POINT('Ctrl Pts',(5.08159043747568,-0.0785283114140747,
-5.64988487684958));
#4420=CARTESIAN_POINT('Ctrl Pts',(5.08237516046643,-0.0210718699127709,
-5.64692151098283));
#4421=CARTESIAN_POINT('Ctrl Pts',(5.08316138940842,0.0364948354656624,-5.64395245816087));
#4422=CARTESIAN_POINT('Ctrl Pts',(5.08072049402758,0.09403688916843,-5.6409834053389));
#4423=CARTESIAN_POINT('Ctrl Pts',(5.07509602117283,0.151169993393991,-5.63801435251694));
#4424=CARTESIAN_POINT('Ctrl Pts',(5.0700740281433,0.202183138729789,-5.63536333739761));
#4425=CARTESIAN_POINT('Ctrl Pts',(5.06251474258129,0.252870072794343,-5.63271232227827));
#4426=CARTESIAN_POINT('Ctrl Pts',(5.05248338402327,0.302965221194532,-5.63006130715894));
#4427=CARTESIAN_POINT('Ctrl Pts',(5.04124398616276,0.359093142501999,-5.62709104012201));
#4428=CARTESIAN_POINT('Ctrl Pts',(5.02685363357415,0.414711515953188,-5.62412077308509));
#4429=CARTESIAN_POINT('Ctrl Pts',(5.00937431062045,0.469440639559313,-5.62115050604816));
#4430=CARTESIAN_POINT('Ctrl Pts',(4.99192585970976,0.524073100390679,-5.61818548510755));
#4431=CARTESIAN_POINT('Ctrl Pts',(4.97139942469621,0.57781893626908,-5.61522046416694));
#4432=CARTESIAN_POINT('Ctrl Pts',(4.94790777060758,0.63030961666217,-5.61225544322633));
#4433=CARTESIAN_POINT('Ctrl Pts',(4.92443929913074,0.682748496911197,-5.6092933483006));
#4434=CARTESIAN_POINT('Ctrl Pts',(4.89801161826705,0.733934202401455,-5.60633125337487));
#4435=CARTESIAN_POINT('Ctrl Pts',(4.86878638733919,0.783516015795281,-5.60336915844913));
#4436=CARTESIAN_POINT('Ctrl Pts',(4.83957874786955,0.833067984552437,-5.60040884648858));
#4437=CARTESIAN_POINT('Ctrl Pts',(4.80757716062695,0.881017526855358,-5.59744853452803));
#4438=CARTESIAN_POINT('Ctrl Pts',(4.7729892208029,0.9270384775094,-5.59448822256748));
#4439=CARTESIAN_POINT('Ctrl Pts',(4.73840878763058,0.973049440195079,-5.5915285530861));
#4440=CARTESIAN_POINT('Ctrl Pts',(4.70124342942734,1.0171322258076,-5.58856888360472));
#4441=CARTESIAN_POINT('Ctrl Pts',(4.66174277275769,1.05899146220791,-5.58560921412333));
#4442=CARTESIAN_POINT('Ctrl Pts',(4.62220649312785,1.10088844861133,-5.58264687551701));
#4443=CARTESIAN_POINT('Ctrl Pts',(4.5803310645842,1.14055749815937,-5.57968453691068));
#4444=CARTESIAN_POINT('Ctrl Pts',(4.53640402249908,1.17773908504764,-5.57672219830435));
#4445=CARTESIAN_POINT('Ctrl Pts',(4.49245843394368,1.21493637040236,-5.57375860896676));
#4446=CARTESIAN_POINT('Ctrl Pts',(4.44645992134105,1.24964378394846,-5.57079501962917));
#4447=CARTESIAN_POINT('Ctrl Pts',(4.39872771866148,1.28164326722526,-5.56783143029157));
#4448=CARTESIAN_POINT('Ctrl Pts',(4.35090399238202,1.31370410756794,-5.5648621584514));
#4449=CARTESIAN_POINT('Ctrl Pts',(4.30134038312763,1.34304637521189,-5.56189288661123));
#4450=CARTESIAN_POINT('Ctrl Pts',(4.25038276935214,1.36949690511159,-5.55892361477106));
#4451=CARTESIAN_POINT('Ctrl Pts',(4.20491786967552,1.3930963360736,-5.55627440032941));
#4452=CARTESIAN_POINT('Ctrl Pts',(4.15834386516771,1.41439438923619,-5.55362518588776));
#4453=CARTESIAN_POINT('Ctrl Pts',(4.11091835799445,1.43330102606077,-5.55097597144611));
#4454=CARTESIAN_POINT('Ctrl Pts',(4.05774453158703,1.45449928590827,-5.54800565278781));
#4455=CARTESIAN_POINT('Ctrl Pts',(4.00327892648833,1.47277857230596,-5.5450353341295));
#4456=CARTESIAN_POINT('Ctrl Pts',(3.94787360955783,1.48798372102446,-5.5420650154712));
#4457=CARTESIAN_POINT('Ctrl Pts',(3.89256610051544,1.50316202785184,-5.53909994036371));
#4458=CARTESIAN_POINT('Ctrl Pts',(3.83632267091484,1.51527683172048,-5.53613486525623));
#4459=CARTESIAN_POINT('Ctrl Pts',(3.77951372278401,1.52422162339941,-5.53316979014875));
#4460=CARTESIAN_POINT('Ctrl Pts',(3.72276080637997,1.53315759266321,-5.53020763955023));
#4461=CARTESIAN_POINT('Ctrl Pts',(3.66544398895872,1.53892966400306,-5.52724548895171));
#4462=CARTESIAN_POINT('Ctrl Pts',(3.60794541203941,1.54148202488253,-5.5242833383532));
#4463=CARTESIAN_POINT('Ctrl Pts',(3.55048141736608,1.54403285065667,-5.52132296932609));
#4464=CARTESIAN_POINT('Ctrl Pts',(3.49283639960112,1.54336778169137,-5.51836260029899));
#4465=CARTESIAN_POINT('Ctrl Pts',(3.43539697819457,1.53948289827294,-5.51540223127188));
#4466=CARTESIAN_POINT('Ctrl Pts',(3.37796999777386,1.5355988562937,-5.51244250344046));
#4467=CARTESIAN_POINT('Ctrl Pts',(3.32074904510053,1.5284964197212,-5.50948277560903));
#4468=CARTESIAN_POINT('Ctrl Pts',(3.26411785739403,1.51822369329365,-5.50652304777761));
#4469=CARTESIAN_POINT('Ctrl Pts',(3.20743556993601,1.50794169752551,-5.50356064930899));
#4470=CARTESIAN_POINT('Ctrl Pts',(3.15134462507232,1.49448378804402,-5.50059825084036));
#4471=CARTESIAN_POINT('Ctrl Pts',(3.09621939422068,1.47794939521315,-5.49763585237174));
#4472=CARTESIAN_POINT('Ctrl Pts',(3.0410708721494,1.46140801635847,-5.49467220224625));
#4473=CARTESIAN_POINT('Ctrl Pts',(2.9868893689835,1.44178773967977,-5.49170855212077));
#4474=CARTESIAN_POINT('Ctrl Pts',(2.93403179183757,1.41923718232391,-5.48874490199529));
#4475=CARTESIAN_POINT('Ctrl Pts',(2.8810728522954,1.39664338086469,-5.48577556862258));
#4476=CARTESIAN_POINT('Ctrl Pts',(2.82944338102946,1.37110830140213,-5.48280623524988));
#4477=CARTESIAN_POINT('Ctrl Pts',(2.77947719277766,1.34282738080032,-5.47983690187717));
#4478=CARTESIAN_POINT('Ctrl Pts',(2.73490550162595,1.31759975182454,-5.47718814649588));
#4479=CARTESIAN_POINT('Ctrl Pts',(2.69165718122887,1.29018796291122,-5.47453939111459));
#4480=CARTESIAN_POINT('Ctrl Pts',(2.64994809620117,1.26075870705099,-5.47189063573329));
#4481=CARTESIAN_POINT('Ctrl Pts',(2.60346496462164,1.22796096115151,-5.46893870224377));
#4482=CARTESIAN_POINT('Ctrl Pts',(2.55869546569534,1.19251654365165,-5.46598676875425));
#4483=CARTESIAN_POINT('Ctrl Pts',(2.51595948046345,1.15463189231211,-5.46303483526472));
#4484=CARTESIAN_POINT('Ctrl Pts',(2.47329895141399,1.11681413146655,-5.46008811381444));
#4485=CARTESIAN_POINT('Ctrl Pts',(2.43266520432176,1.07656503309214,-5.45714139236415));
#4486=CARTESIAN_POINT('Ctrl Pts',(2.39434758436882,1.0341331216702,-5.45419467091387));
#4487=CARTESIAN_POINT('Ctrl Pts',(2.35606741861139,0.991742686026445,-5.45125082978552));
#4488=CARTESIAN_POINT('Ctrl Pts',(2.32009924872405,0.947174053247093,-5.44830698865717));
#4489=CARTESIAN_POINT('Ctrl Pts',(2.28669647218713,0.90071337697541,-5.44536314752882));
#4490=CARTESIAN_POINT('Ctrl Pts',(2.25331307243261,0.854279652307993,-5.44242101410788));
#4491=CARTESIAN_POINT('Ctrl Pts',(2.22249242482938,0.805956487503688,-5.43947888068694));
#4492=CARTESIAN_POINT('Ctrl Pts',(2.19444693579754,0.756062171026311,-5.436536747266));
#4493=CARTESIAN_POINT('Ctrl Pts',(2.16640657201678,0.706176972624892,-5.43359515151344));
#4494=CARTESIAN_POINT('Ctrl Pts',(2.14114061823626,0.654721653414925,-5.43065355576087));
#4495=CARTESIAN_POINT('Ctrl Pts',(2.11881630704433,0.602040459567581,-5.4277119600083));
#4496=CARTESIAN_POINT('Ctrl Pts',(2.09647190485982,0.549311854740122,-5.4247677169365));
#4497=CARTESIAN_POINT('Ctrl Pts',(2.07707463860601,0.49535565974548,-5.4218234738647));
#4498=CARTESIAN_POINT('Ctrl Pts',(2.06074356441428,0.440536107464182,-5.41887923079291));
#4499=CARTESIAN_POINT('Ctrl Pts',(2.0444047076198,0.385690430826799,-5.41593358463678));
#4500=CARTESIAN_POINT('Ctrl Pts',(2.03113507514356,0.329981092328246,-5.41298793848066));
#4501=CARTESIAN_POINT('Ctrl Pts',(2.02100294881358,0.273784311371141,-5.41004229232454));
#4502=CARTESIAN_POINT('Ctrl Pts',(2.01085268402028,0.217486927320778,-5.40709137289279));
#4503=CARTESIAN_POINT('Ctrl Pts',(2.00385120279259,0.160700883809956,-5.40414045346105));
#4504=CARTESIAN_POINT('Ctrl Pts',(2.00001494507583,0.103808042170368,-5.40118953402931));
#4505=CARTESIAN_POINT('Ctrl Pts',(1.9976743620204,0.0690965001028133,-5.399389114837));
#4506=CARTESIAN_POINT('Ctrl Pts',(1.99651100345573,0.034345238722842,-5.39758869564469));
#4507=CARTESIAN_POINT('Ctrl Pts',(1.99651909233433,-0.000359636485246585,
-5.39578827645238));
#4508=CARTESIAN_POINT('Origin',(3.53951905042299,8.32667268468867E-16,-7.60421172358873));
#4509=CARTESIAN_POINT('',(4.47947725029973,-1.22365337513712,-6.21868039134515));
#4510=CARTESIAN_POINT('',(4.48050266131609,-1.22496740309806,-6.17703688246106));
#4511=CARTESIAN_POINT('',(4.47947725029973,-1.22365337513712,-7.60421172358873));
#4512=CARTESIAN_POINT('',(1.99673565886186,0.00179124603277963,-6.39578836743343));
#4513=CARTESIAN_POINT('Ctrl Pts',(1.99652008837714,0.0017897277490038,-6.39578827641128));
#4514=CARTESIAN_POINT('Ctrl Pts',(1.99645403628334,-0.055156538086158,-6.39286004236045));
#4515=CARTESIAN_POINT('Ctrl Pts',(1.99954477721908,-0.11215736321612,-6.38993180830962));
#4516=CARTESIAN_POINT('Ctrl Pts',(2.00578359056079,-0.168832873461531,-6.38700357425878));
#4517=CARTESIAN_POINT('Ctrl Pts',(2.01202038127157,-0.22549000943717,-6.38407628954501));
#4518=CARTESIAN_POINT('Ctrl Pts',(2.02140316267154,-0.281821510112156,-6.38114900483125));
#4519=CARTESIAN_POINT('Ctrl Pts',(2.03387131239083,-0.33745205431088,-6.37822172011748));
#4520=CARTESIAN_POINT('Ctrl Pts',(2.04678845321045,-0.395085912538913,-6.37518902082222));
#4521=CARTESIAN_POINT('Ctrl Pts',(2.06301736691178,-0.451966755193889,-6.37215632152696));
#4522=CARTESIAN_POINT('Ctrl Pts',(2.08243330891811,-0.507690990567261,-6.36912362223169));
#4523=CARTESIAN_POINT('Ctrl Pts',(2.10119790125384,-0.561545836222492,-6.3661926613783));
#4524=CARTESIAN_POINT('Ctrl Pts',(2.12293876895841,-0.614319974748326,-6.3632617005249));
#4525=CARTESIAN_POINT('Ctrl Pts',(2.14749415252614,-0.665669350079501,-6.3603307396715));
#4526=CARTESIAN_POINT('Ctrl Pts',(2.17332807234279,-0.719692356532698,-6.35724717115531));
#4527=CARTESIAN_POINT('Ctrl Pts',(2.20227731628823,-0.772137569091362,-6.35416360263912));
#4528=CARTESIAN_POINT('Ctrl Pts',(2.23410044380417,-0.822636773730281,-6.35108003412292));
#4529=CARTESIAN_POINT('Ctrl Pts',(2.2659235713201,-0.873135978369199,-6.34799646560673));
#4530=CARTESIAN_POINT('Ctrl Pts',(2.30062011630072,-0.921688676698492,-6.34491289709054));
#4531=CARTESIAN_POINT('Ctrl Pts',(2.33790045788765,-0.967967849710609,-6.34182932857435));
#4532=CARTESIAN_POINT('Ctrl Pts',(2.3738540446845,-1.01260001221099,-6.33885549991368));
#4533=CARTESIAN_POINT('Ctrl Pts',(2.41237149952583,-1.05531795719075,-6.33588167125301));
#4534=CARTESIAN_POINT('Ctrl Pts',(2.45322151678262,-1.09581324522331,-6.33290784259233));
#4535=CARTESIAN_POINT('Ctrl Pts',(2.49399924564804,-1.13623687259509,-6.32993927643348));
#4536=CARTESIAN_POINT('Ctrl Pts',(2.53710097697729,-1.17444528766237,-6.32697071027463));
#4537=CARTESIAN_POINT('Ctrl Pts',(2.58225558169485,-1.21016348128613,-6.32400214411577));
#4538=CARTESIAN_POINT('Ctrl Pts',(2.62736548428903,-1.24584631463803,-6.32103651677592));
#4539=CARTESIAN_POINT('Ctrl Pts',(2.67452382749928,-1.27904349068993,-6.31807088943608));
#4540=CARTESIAN_POINT('Ctrl Pts',(2.7234243909379,-1.30951842551371,-6.31510526209623));
#4541=CARTESIAN_POINT('Ctrl Pts',(2.77229523555306,-1.3399748395037,-6.31214143708644));
#4542=CARTESIAN_POINT('Ctrl Pts',(2.82290576097275,-1.3677120178566,-6.30917761207666));
#4543=CARTESIAN_POINT('Ctrl Pts',(2.87492038146038,-1.39253639421493,-6.30621378706687));
#4544=CARTESIAN_POINT('Ctrl Pts',(2.92692327130035,-1.41735517203175,-6.30325063047659));
#4545=CARTESIAN_POINT('Ctrl Pts',(2.98032915856549,-1.43926222845626,-6.30028747388631));
#4546=CARTESIAN_POINT('Ctrl Pts',(3.03477942309202,-1.45811073262691,-6.29732431729602));
#4547=CARTESIAN_POINT('Ctrl Pts',(3.08927744992821,-1.47697577019921,-6.29435856150436));
#4548=CARTESIAN_POINT('Ctrl Pts',(3.14482119268528,-1.49277672287494,-6.2913928057127));
#4549=CARTESIAN_POINT('Ctrl Pts',(3.20103498306298,-1.50541606745226,-6.28842704992104));
#4550=CARTESIAN_POINT('Ctrl Pts',(3.25727185362023,-1.51806060147403,-6.28546007645351));
#4551=CARTESIAN_POINT('Ctrl Pts',(3.31417880676457,-1.52754085216985,-6.28249310298597));
#4552=CARTESIAN_POINT('Ctrl Pts',(3.37137119544686,-1.53381071155046,-6.27952612951844));
#4553=CARTESIAN_POINT('Ctrl Pts',(3.42867118730259,-1.54009236719945,-6.2765535739137));
#4554=CARTESIAN_POINT('Ctrl Pts',(3.48625716706642,-1.54315153299832,-6.27358101830897));
#4555=CARTESIAN_POINT('Ctrl Pts',(3.54374157597108,-1.5429942223735,-6.27060846270423));
#4556=CARTESIAN_POINT('Ctrl Pts',(3.59443694390479,-1.54285549049546,-6.26798697275666));
#4557=CARTESIAN_POINT('Ctrl Pts',(3.64505308062308,-1.54021596828826,-6.26536548280909));
#4558=CARTESIAN_POINT('Ctrl Pts',(3.69532853995772,-1.53511315640604,-6.26274399286153));
#4559=CARTESIAN_POINT('Ctrl Pts',(3.75238143557914,-1.5293224545896,-6.25976911019848));
#4560=CARTESIAN_POINT('Ctrl Pts',(3.80922524850646,-1.52033529212181,-6.25679422753544));
#4561=CARTESIAN_POINT('Ctrl Pts',(3.86547505287269,-1.50817826680635,-6.25381934487239));
#4562=CARTESIAN_POINT('Ctrl Pts',(3.92163253419786,-1.49604119486779,-6.2508493448968));
#4563=CARTESIAN_POINT('Ctrl Pts',(3.97719743813669,-1.48074469342844,-6.24787934492122));
#4564=CARTESIAN_POINT('Ctrl Pts',(4.03179118627241,-1.46236696634813,-6.24490934494563));
#4565=CARTESIAN_POINT('Ctrl Pts',(4.08633139370007,-1.44400726251324,-6.24194225768271));
#4566=CARTESIAN_POINT('Ctrl Pts',(4.13990184334824,-1.42257248758474,-6.23897517041978));
#4567=CARTESIAN_POINT('Ctrl Pts',(4.19213719523688,-1.39819117328771,-6.23600808315686));
#4568=CARTESIAN_POINT('Ctrl Pts',(4.24435372260801,-1.37381864550137,-6.23304206516952));
#4569=CARTESIAN_POINT('Ctrl Pts',(4.29523563084465,-1.34650189102749,-6.23007604718218));
#4570=CARTESIAN_POINT('Ctrl Pts',(4.34443752800149,-1.31641757981756,-6.22711002919483));
#4571=CARTESIAN_POINT('Ctrl Pts',(4.39104931259161,-1.28791698299728,-6.22430014991161));
#4572=CARTESIAN_POINT('Ctrl Pts',(4.43615314090438,-1.25693310345394,-6.22149027062838));
#4573=CARTESIAN_POINT('Ctrl Pts',(4.47947725029973,-1.22365337513712,-6.21868039134515));
#4574=CARTESIAN_POINT('',(3.14100520856574,1.49064942821851,-6.5));
#4575=CARTESIAN_POINT('Ctrl Pts',(3.14100520856575,1.49064942821851,-6.5));
#4576=CARTESIAN_POINT('Ctrl Pts',(2.64719497069073,1.35863299878936,-6.47363822142906));
#4577=CARTESIAN_POINT('Ctrl Pts',(2.09523405725447,0.837507597441754,-6.43890120269724));
#4578=CARTESIAN_POINT('Ctrl Pts',(1.99690773965972,0.164511449214008,-6.40416418396542));
#4579=CARTESIAN_POINT('Ctrl Pts',(1.99810069593897,0.00180086012095238,
-6.39578894380455));
#4580=CARTESIAN_POINT('',(3.93825622282343,1.49058970456196,-6.49999997840053));
#4581=CARTESIAN_POINT('Origin',(3.53951905042299,8.32667268468867E-16,-6.5));
#4582=CARTESIAN_POINT('',(1.99642704442048,-0.000970003776170875,-6.35421172358872));
#4583=CARTESIAN_POINT('Ctrl Pts',(3.93825622282343,1.49058970456196,-6.49999997840053));
#4584=CARTESIAN_POINT('Ctrl Pts',(3.88320017949414,1.50531735964604,-6.49704310510064));
#4585=CARTESIAN_POINT('Ctrl Pts',(3.82720821675325,1.51702233478024,-6.49408623180075));
#4586=CARTESIAN_POINT('Ctrl Pts',(3.77064508224469,1.52559160898792,-6.49112935850085));
#4587=CARTESIAN_POINT('Ctrl Pts',(3.71418095414078,1.53414588379649,-6.4881776608228));
#4588=CARTESIAN_POINT('Ctrl Pts',(3.65714815441855,1.53957527077174,-6.48522596314475));
#4589=CARTESIAN_POINT('Ctrl Pts',(3.59992408344123,1.54181718500802,-6.48227426546669));
#4590=CARTESIAN_POINT('Ctrl Pts',(3.54275550164339,1.54405692529934,-6.47932542999819));
#4591=CARTESIAN_POINT('Ctrl Pts',(3.48539653951463,1.54311529457029,-6.47637659452968));
#4592=CARTESIAN_POINT('Ctrl Pts',(3.42823038115855,1.53898142681884,-6.47342775906117));
#4593=CARTESIAN_POINT('Ctrl Pts',(3.37109712766582,1.5348499385233,-6.47048062094353));
#4594=CARTESIAN_POINT('Ctrl Pts',(3.3141569821572,1.52752989286647,-6.46753348282588));
#4595=CARTESIAN_POINT('Ctrl Pts',(3.25779148941335,1.51706248433199,-6.46458634470824));
#4596=CARTESIAN_POINT('Ctrl Pts',(3.20143622917433,1.50659697603476,-6.46163974160951));
#4597=CARTESIAN_POINT('Ctrl Pts',(3.14565593190065,1.49298533599691,-6.45869313851079));
#4598=CARTESIAN_POINT('Ctrl Pts',(3.09082310807727,1.47632007075786,-6.45574653541206));
#4599=CARTESIAN_POINT('Ctrl Pts',(3.03594089558616,1.4596397948885,-6.45279727826798));
#4600=CARTESIAN_POINT('Ctrl Pts',(2.98200836571185,1.43990055421428,-6.4498480211239));
#4601=CARTESIAN_POINT('Ctrl Pts',(2.92938251822518,1.41724465498291,-6.44689876397981));
#4602=CARTESIAN_POINT('Ctrl Pts',(2.87673184203508,1.39457806677208,-6.44394811538582));
#4603=CARTESIAN_POINT('Ctrl Pts',(2.82538954798554,1.36899231429978,-6.44099746679182));
#4604=CARTESIAN_POINT('Ctrl Pts',(2.77568933676639,1.34067638471604,-6.43804681819783));
#4605=CARTESIAN_POINT('Ctrl Pts',(2.7258998292641,1.31230957995083,-6.43509086817863));
#4606=CARTESIAN_POINT('Ctrl Pts',(2.67775873799462,1.28120309021216,-6.43213491815943));
#4607=CARTESIAN_POINT('Ctrl Pts',(2.63157094440542,1.24758937025734,-6.42917896814024));
#4608=CARTESIAN_POINT('Ctrl Pts',(2.60218002465184,1.22619977640494,-6.42729799303711));
#4609=CARTESIAN_POINT('Ctrl Pts',(2.57357939911721,1.20379579159119,-6.42541701793398));
#4610=CARTESIAN_POINT('Ctrl Pts',(2.54584005379241,1.18044527685753,-6.42353604283085));
#4611=CARTESIAN_POINT('Ctrl Pts',(2.5025987241781,1.1440454522604,-6.42060389488437));
#4612=CARTESIAN_POINT('Ctrl Pts',(2.46126130737398,1.10518307986427,-6.41767174693789));
#4613=CARTESIAN_POINT('Ctrl Pts',(2.42212621493193,1.06408752045743,-6.41473959899141));
#4614=CARTESIAN_POINT('Ctrl Pts',(2.38304397962318,1.02304746605458,-6.41181141129966));
#4615=CARTESIAN_POINT('Ctrl Pts',(2.346158547839,0.979780578008112,-6.4088832236079));
#4616=CARTESIAN_POINT('Ctrl Pts',(2.31173475047303,0.934555890675563,-6.40595503591615));
#4617=CARTESIAN_POINT('Ctrl Pts',(2.27734338470286,0.889373810751027,-6.40302960694967));
#4618=CARTESIAN_POINT('Ctrl Pts',(2.24540938426969,0.842238007844451,-6.40010417798319));
#4619=CARTESIAN_POINT('Ctrl Pts',(2.21615855693819,0.79345195461582,-6.39717874901671));
#4620=CARTESIAN_POINT('Ctrl Pts',(2.18692334329738,0.744691942713686,-6.39425488160411));
#4621=CARTESIAN_POINT('Ctrl Pts',(2.16036873932762,0.694283884801881,-6.39133101419151));
#4622=CARTESIAN_POINT('Ctrl Pts',(2.1366769243486,0.642559700970342,-6.38840714677891));
#4623=CARTESIAN_POINT('Ctrl Pts',(2.1129737029059,0.590810614444568,-6.38548187166549));
#4624=CARTESIAN_POINT('Ctrl Pts',(2.09213625856676,0.537744618682926,-6.38255659655207));
#4625=CARTESIAN_POINT('Ctrl Pts',(2.07429971023128,0.483716120393116,-6.37963132143865));
#4626=CARTESIAN_POINT('Ctrl Pts',(2.05645979752164,0.429677431113449,-6.37670549455255));
#4627=CARTESIAN_POINT('Ctrl Pts',(2.04162205759539,0.374676393092577,-6.37377966766645));
#4628=CARTESIAN_POINT('Ctrl Pts',(2.02987153650266,0.319082095571282,-6.37085384078036));
#4629=CARTESIAN_POINT('Ctrl Pts',(2.0181021161795,0.26339838163765,-6.36792330807091));
#4630=CARTESIAN_POINT('Ctrl Pts',(2.00942992235938,0.207120032030301,-6.36499277536147));
#4631=CARTESIAN_POINT('Ctrl Pts',(2.00388848089591,0.15062454625301,-6.36206224265202));
#4632=CARTESIAN_POINT('Ctrl Pts',(1.99894021196776,0.100176506930577,-6.35944540296426));
#4633=CARTESIAN_POINT('Ctrl Pts',(1.99648759434767,0.0495556759557013,-6.35682856327649));
#4634=CARTESIAN_POINT('Ctrl Pts',(1.99651935528198,-0.000969945748597822,
-6.35421172358872));
#4635=CARTESIAN_POINT('Ctrl Pts',(1.99491409331847,-0.000970954833059484,
-6.35421172358872));
#4636=CARTESIAN_POINT('Ctrl Pts',(1.99443510396552,-0.0638581426144525,
-6.35095805143182));
#4637=CARTESIAN_POINT('Ctrl Pts',(2.02640462481052,-0.635796929598567,-6.32134260070397));
#4638=CARTESIAN_POINT('Ctrl Pts',(2.7401727925123,-1.63684014941779,-6.26536537140521));
#4639=CARTESIAN_POINT('Ctrl Pts',(3.96445470277286,-1.58450089972216,-6.20956076318621));
#4640=CARTESIAN_POINT('Ctrl Pts',(4.4335630505712,-1.26162659872001,-6.18011793353816));
#4641=CARTESIAN_POINT('Ctrl Pts',(4.4805026613161,-1.22496740309806,-6.17703688246106));
#4642=CARTESIAN_POINT('Origin',(3.53951905042299,8.32667268468867E-16,-6.5));
#4643=CARTESIAN_POINT('',(3.98033068508385,1.1851773507571,-5.34783926643463));
#4644=CARTESIAN_POINT('',(3.98033068509731,1.1851773507521,-5.20988106086703));
#4645=CARTESIAN_POINT('',(3.98033068509731,1.1851773507521,-6.5));
#4646=CARTESIAN_POINT('',(2.27502014636762,0.00166482514493488,-5.05658113604771));
#4647=CARTESIAN_POINT('Ctrl Pts',(3.98033068509731,1.1851773507521,-5.20988106086703));
#4648=CARTESIAN_POINT('Ctrl Pts',(3.93383793648786,1.20246973699456,-5.20676616267198));
#4649=CARTESIAN_POINT('Ctrl Pts',(3.88629663681185,1.21703326229598,-5.20365126447694));
#4650=CARTESIAN_POINT('Ctrl Pts',(3.83805721807373,1.22875351981418,-5.20053636628189));
#4651=CARTESIAN_POINT('Ctrl Pts',(3.7898260992678,1.24047176077942,-5.19742200402705));
#4652=CARTESIAN_POINT('Ctrl Pts',(3.7408976307118,1.24934757713148,-5.19430764177221));
#4653=CARTESIAN_POINT('Ctrl Pts',(3.69163490741804,1.25531709780862,-5.19119327951737));
#4654=CARTESIAN_POINT('Ctrl Pts',(3.64232470727583,1.26129237159906,-5.18807591580229));
#4655=CARTESIAN_POINT('Ctrl Pts',(3.59268015271285,1.26435569180074,-5.18495855208722));
#4656=CARTESIAN_POINT('Ctrl Pts',(3.54307018622395,1.26449501360603,-5.18184118837215));
#4657=CARTESIAN_POINT('Ctrl Pts',(3.49343414586118,1.26463440863571,-5.17872218624137));
#4658=CARTESIAN_POINT('Ctrl Pts',(3.44383327594736,1.2618467746437,-5.17560318411059));
#4659=CARTESIAN_POINT('Ctrl Pts',(3.394633694541,1.25617215526016,-5.17248418197981));
#4660=CARTESIAN_POINT('Ctrl Pts',(3.34534262492254,1.25048698373843,-5.16935937996374));
#4661=CARTESIAN_POINT('Ctrl Pts',(3.29645487202891,1.24190420480259,-5.16623457794767));
#4662=CARTESIAN_POINT('Ctrl Pts',(3.24832704708739,1.2305151227,-5.1631097759316));
#4663=CARTESIAN_POINT('Ctrl Pts',(3.22296988250465,1.22451454341614,-5.16146340776295));
#4664=CARTESIAN_POINT('Ctrl Pts',(3.1978234261036,1.21773579564166,-5.1598170395943));
#4665=CARTESIAN_POINT('Ctrl Pts',(3.17293779691212,1.21019768408901,-5.15817067142565));
#4666=CARTESIAN_POINT('Ctrl Pts',(3.12623148321434,1.19604986406976,-5.15508070381603));
#4667=CARTESIAN_POINT('Ctrl Pts',(3.08023135044039,1.17915948645447,-5.1519907362064));
#4668=CARTESIAN_POINT('Ctrl Pts',(3.03528596549808,1.1596159907776,-5.14890076859677));
#4669=CARTESIAN_POINT('Ctrl Pts',(2.99042256294068,1.1401081433077,-5.14581643722575));
#4670=CARTESIAN_POINT('Ctrl Pts',(2.94661060463452,1.11795698926683,-5.14273210585473));
#4671=CARTESIAN_POINT('Ctrl Pts',(2.90418287418204,1.09330151063626,-5.1396477744837));
#4672=CARTESIAN_POINT('Ctrl Pts',(2.86179747117057,1.06867062920442,-5.1365665201534));
#4673=CARTESIAN_POINT('Ctrl Pts',(2.82079404657099,1.04154064457733,-5.1334852658231));
#4674=CARTESIAN_POINT('Ctrl Pts',(2.78148262924307,1.01209734421385,-5.13040401149279));
#4675=CARTESIAN_POINT('Ctrl Pts',(2.74219287983153,0.982670272595451,-5.1273244555078));
#4676=CARTESIAN_POINT('Ctrl Pts',(2.70459373924722,0.950932744232993,-5.1242448995228));
#4677=CARTESIAN_POINT('Ctrl Pts',(2.66896563574984,0.917113407491636,-5.12116534353781));
#4678=CARTESIAN_POINT('Ctrl Pts',(2.63334126514557,0.883297614131952,-5.11808611020971));
#4679=CARTESIAN_POINT('Ctrl Pts',(2.5996879267293,0.847400831915252,-5.11500687688161));
#4680=CARTESIAN_POINT('Ctrl Pts',(2.56825029767131,0.809689607150916,-5.11192764355352));
#4681=CARTESIAN_POINT('Ctrl Pts',(2.53677682467762,0.771935385546272,-5.10884489940591));
#4682=CARTESIAN_POINT('Ctrl Pts',(2.50752446118266,0.7323630247258,-5.1057621552583));
#4683=CARTESIAN_POINT('Ctrl Pts',(2.48069730103542,0.691271837285332,-5.10267941111069));
#4684=CARTESIAN_POINT('Ctrl Pts',(2.45385343030684,0.650155054231102,-5.09959474672827));
#4685=CARTESIAN_POINT('Ctrl Pts',(2.42943804360905,0.607518050553414,-5.09651008234585));
#4686=CARTESIAN_POINT('Ctrl Pts',(2.40760963429149,0.563685482936052,-5.09342541796343));
#4687=CARTESIAN_POINT('Ctrl Pts',(2.38573573195641,0.519761563001731,-5.09033432477125));
#4688=CARTESIAN_POINT('Ctrl Pts',(2.36645978141159,0.474637623744029,-5.08724323157908));
#4689=CARTESIAN_POINT('Ctrl Pts',(2.34989178961744,0.428657474387527,-5.0841521383869));
#4690=CARTESIAN_POINT('Ctrl Pts',(2.3408392484497,0.403534502326666,-5.08246320416221));
#4691=CARTESIAN_POINT('Ctrl Pts',(2.33259425763629,0.378156169768814,-5.08077426993752));
#4692=CARTESIAN_POINT('Ctrl Pts',(2.32516831107601,0.352579823369751,-5.07908533571283));
#4693=CARTESIAN_POINT('Ctrl Pts',(2.30700791862498,0.290032041171172,-5.07495499245014));
#4694=CARTESIAN_POINT('Ctrl Pts',(2.2936812592166,0.226070765504886,-5.07082464918745));
#4695=CARTESIAN_POINT('Ctrl Pts',(2.28535400033502,0.161339013068296,-5.06669430592475));
#4696=CARTESIAN_POINT('Ctrl Pts',(2.27855755281454,0.108506986995674,-5.06332324929907));
#4697=CARTESIAN_POINT('Ctrl Pts',(2.27509057994272,0.0551618418107654,-5.05995219267339));
#4698=CARTESIAN_POINT('Ctrl Pts',(2.27502014636762,0.00166482514493488,
-5.05658113604771));
#4699=CARTESIAN_POINT('',(2.58140289770062,-0.825211298936501,-5.));
#4700=CARTESIAN_POINT('Ctrl Pts',(2.27502018610934,0.00169474171970803,
-5.05612766244439));
#4701=CARTESIAN_POINT('Ctrl Pts',(2.27492762199581,-0.067370187214906,-5.05136691138681));
#4702=CARTESIAN_POINT('Ctrl Pts',(2.28049343395356,-0.136334638631543,-5.0466822093755));
#4703=CARTESIAN_POINT('Ctrl Pts',(2.2980708935941,-0.243587770328582,-5.0395587692782));
#4704=CARTESIAN_POINT('Ctrl Pts',(2.30630841992252,-0.282348371496498,-5.03701662818025));
#4705=CARTESIAN_POINT('Ctrl Pts',(2.32685863727146,-0.360737280072117,-5.03192125490839));
#4706=CARTESIAN_POINT('Ctrl Pts',(2.33932850452305,-0.400274698986001,-5.02937610304411));
#4707=CARTESIAN_POINT('Ctrl Pts',(2.37034907125676,-0.484040487389494,-5.02398385765428));
#4708=CARTESIAN_POINT('Ctrl Pts',(2.38951839495634,-0.527970216674481,-5.02115625735706));
#4709=CARTESIAN_POINT('Ctrl Pts',(2.44620717420155,-0.640053277041579,-5.01378604101922));
#4710=CARTESIAN_POINT('Ctrl Pts',(2.48759504636693,-0.706012164800675,-5.00929109021215));
#4711=CARTESIAN_POINT('Ctrl Pts',(2.54975148458737,-0.787355859854348,-5.00307314010455));
#4712=CARTESIAN_POINT('Ctrl Pts',(2.56530247076859,-0.806517809003463,-5.00155260994088));
#4713=CARTESIAN_POINT('Ctrl Pts',(2.58140289770062,-0.825211298936505,-5.));
#4714=CARTESIAN_POINT('',(4.48475997009368,-0.83992848134833,-5.));
#4715=CARTESIAN_POINT('Origin',(3.53951905042299,8.32667268468867E-16,-5.));
#4716=CARTESIAN_POINT('Ctrl Pts',(4.48475997009368,-0.83992848134833,-5.));
#4717=CARTESIAN_POINT('Ctrl Pts',(4.4743645141033,-0.851627346905269,-5.0010238610782));
#4718=CARTESIAN_POINT('Ctrl Pts',(4.46375282341081,-0.863132148146834,-5.00206025069617));
#4719=CARTESIAN_POINT('Ctrl Pts',(4.40421107071591,-0.925327730920914,-5.00781443230508));
#4720=CARTESIAN_POINT('Ctrl Pts',(4.35132615145554,-0.97205564021386,-5.01269719730609));
#4721=CARTESIAN_POINT('Ctrl Pts',(4.25291556543452,-1.04535004341478,-5.02111726956437));
#4722=CARTESIAN_POINT('Ctrl Pts',(4.20910528876381,-1.07393968753869,-5.02467043786506));
#4723=CARTESIAN_POINT('Ctrl Pts',(4.12654471049289,-1.12079487791517,-5.03097376948309));
#4724=CARTESIAN_POINT('Ctrl Pts',(4.0883967039719,-1.13996241146875,-5.03374816690764));
#4725=CARTESIAN_POINT('Ctrl Pts',(4.0174102350422,-1.17123795030084,-5.0386725547192));
#4726=CARTESIAN_POINT('Ctrl Pts',(3.98490083149402,-1.18398216322048,-5.0408424334626));
#4727=CARTESIAN_POINT('Ctrl Pts',(3.89903290236951,-1.21360535989443,-5.04638289410142));
#4728=CARTESIAN_POINT('Ctrl Pts',(3.84500778793352,-1.22831829455146,-5.04968091607328));
#4729=CARTESIAN_POINT('Ctrl Pts',(3.71808637329925,-1.2539873051317,-5.0571950936033));
#4730=CARTESIAN_POINT('Ctrl Pts',(3.64486043657265,-1.26224916290169,-5.06135580064609));
#4731=CARTESIAN_POINT('Ctrl Pts',(3.54245933434724,-1.26482643100954,-5.06734893032052));
#4732=CARTESIAN_POINT('Ctrl Pts',(3.5135696546245,-1.26456354629239,-5.06906017420318));
#4733=CARTESIAN_POINT('Ctrl Pts',(3.46109229551139,-1.26228706604992,-5.0722450323917));
#4734=CARTESIAN_POINT('Ctrl Pts',(3.43750362481475,-1.26059988191603,-5.07370488792634));
#4735=CARTESIAN_POINT('Ctrl Pts',(3.39105407348582,-1.25596542288288,-5.07665963921581));
#4736=CARTESIAN_POINT('Ctrl Pts',(3.36819912874026,-1.25305237762915,-5.07815265257495));
#4737=CARTESIAN_POINT('Ctrl Pts',(3.2965384961007,-1.24192175199295,-5.08293167075412));
#4738=CARTESIAN_POINT('Ctrl Pts',(3.24813003345425,-1.23146287712779,-5.08630237284614));
#4739=CARTESIAN_POINT('Ctrl Pts',(3.13401621803822,-1.19970202365469,-5.09442626540856));
#4740=CARTESIAN_POINT('Ctrl Pts',(3.06918849400282,-1.17580097531217,-5.09918282320499));
#4741=CARTESIAN_POINT('Ctrl Pts',(2.96247804631192,-1.12621242059119,-5.10708133864211));
#4742=CARTESIAN_POINT('Ctrl Pts',(2.9195427603486,-1.10315961359804,-5.11028233747527));
#4743=CARTESIAN_POINT('Ctrl Pts',(2.84880332620626,-1.05973997347714,-5.11559260274478));
#4744=CARTESIAN_POINT('Ctrl Pts',(2.82030757361024,-1.04061147451596,-5.11774329065059));
#4745=CARTESIAN_POINT('Ctrl Pts',(2.75620244933123,-0.993686332871481,-5.12262750419393));
#4746=CARTESIAN_POINT('Ctrl Pts',(2.72123327068826,-0.965094023148555,-5.125326492505));
#4747=CARTESIAN_POINT('Ctrl Pts',(2.60903907537223,-0.862866940372734,-5.13423063660923));
#4748=CARTESIAN_POINT('Ctrl Pts',(2.53962259610747,-0.781368418606664,-5.14013376231597));
#4749=CARTESIAN_POINT('Ctrl Pts',(2.4632036049359,-0.664525024115634,-5.14836345464608));
#4750=CARTESIAN_POINT('Ctrl Pts',(2.44623638784157,-0.636224064089069,-5.15034459662317));
#4751=CARTESIAN_POINT('Ctrl Pts',(2.42079093564898,-0.589752213326867,-5.15363129948203));
#4752=CARTESIAN_POINT('Ctrl Pts',(2.4116048890828,-0.57198758318919,-5.15489678252057));
#4753=CARTESIAN_POINT('Ctrl Pts',(2.38915256413399,-0.525921738428734,-5.15820497132823));
#4754=CARTESIAN_POINT('Ctrl Pts',(2.37650884762872,-0.497336543800919,-5.1602785064423));
#4755=CARTESIAN_POINT('Ctrl Pts',(2.33313051466738,-0.38853938817627,-5.16817180977536));
#4756=CARTESIAN_POINT('Ctrl Pts',(2.30953313212375,-0.305730994533581,-5.17416419262342));
#4757=CARTESIAN_POINT('Ctrl Pts',(2.28721462895428,-0.180094801583148,-5.18282841741911));
#4758=CARTESIAN_POINT('Ctrl Pts',(2.28195466443356,-0.138682650408762,-5.18562148923988));
#4759=CARTESIAN_POINT('Ctrl Pts',(2.27587380190061,-0.0597133732315236,
-5.19081296811046));
#4760=CARTESIAN_POINT('Ctrl Pts',(2.27465888365585,-0.0222316917080967,
-5.1932202476294));
#4761=CARTESIAN_POINT('Ctrl Pts',(2.27553710499034,0.0505733384564403,-5.1977955046571));
#4762=CARTESIAN_POINT('Ctrl Pts',(2.27744304036795,0.0858635505184319,-5.19996731003112));
#4763=CARTESIAN_POINT('Ctrl Pts',(2.28804875130298,0.19616088358106,-5.20664995369242));
#4764=CARTESIAN_POINT('Ctrl Pts',(2.30198506044707,0.270496428041747,-5.21099058531991));
#4765=CARTESIAN_POINT('Ctrl Pts',(2.33773738553142,0.397298403786643,-5.21852052734508));
#4766=CARTESIAN_POINT('Ctrl Pts',(2.35659993548028,0.450363089996163,-5.22171668726163));
#4767=CARTESIAN_POINT('Ctrl Pts',(2.39279803420042,0.534051715336838,-5.22706607770719));
#4768=CARTESIAN_POINT('Ctrl Pts',(2.4079858052802,0.565519558930165,-5.22915375780192));
#4769=CARTESIAN_POINT('Ctrl Pts',(2.43388776422174,0.613954250597111,-5.23255070019152));
#4770=CARTESIAN_POINT('Ctrl Pts',(2.4437359266768,0.631363294207987,-5.23381224779747));
#4771=CARTESIAN_POINT('Ctrl Pts',(2.46919692470231,0.673980350977448,-5.23700803109764));
#4772=CARTESIAN_POINT('Ctrl Pts',(2.48528903118701,0.698883192109106,-5.23896782302949));
#4773=CARTESIAN_POINT('Ctrl Pts',(2.55114631917314,0.793342341460392,-5.24670165190081));
#4774=CARTESIAN_POINT('Ctrl Pts',(2.60704166538098,0.858346627924565,-5.25266507426581));
#4775=CARTESIAN_POINT('Ctrl Pts',(2.70040320575373,0.94694815151863,-5.26141964091538));
#4776=CARTESIAN_POINT('Ctrl Pts',(2.73324154547406,0.975060710863728,-5.26431831772141));
#4777=CARTESIAN_POINT('Ctrl Pts',(2.79780873090725,1.02483891266637,-5.269672645021));
#4778=CARTESIAN_POINT('Ctrl Pts',(2.82921055875536,1.04684829775139,-5.27213882732288));
#4779=CARTESIAN_POINT('Ctrl Pts',(2.8914676395768,1.0863905158672,-5.27678094391539));
#4780=CARTESIAN_POINT('Ctrl Pts',(2.9221552813526,1.10411835666648,-5.27896272802317));
#4781=CARTESIAN_POINT('Ctrl Pts',(3.01270516141864,1.15147024643782,-5.28513697804023));
#4782=CARTESIAN_POINT('Ctrl Pts',(3.07422041368736,1.17767362145201,-5.28900896875804));
#4783=CARTESIAN_POINT('Ctrl Pts',(3.21462029992273,1.22475031791382,-5.29750616966733));
#4784=CARTESIAN_POINT('Ctrl Pts',(3.29402373486489,1.24310177739744,-5.30209051974957));
#4785=CARTESIAN_POINT('Ctrl Pts',(3.40040308794286,1.25709297651745,-5.30852607071481));
#4786=CARTESIAN_POINT('Ctrl Pts',(3.42627259895793,1.25968687097981,-5.310114481789));
#4787=CARTESIAN_POINT('Ctrl Pts',(3.47308082785827,1.26292685993581,-5.31306001010594));
#4788=CARTESIAN_POINT('Ctrl Pts',(3.49398942685692,1.2638532744479,-5.314403271179));
#4789=CARTESIAN_POINT('Ctrl Pts',(3.55495672925024,1.26504005998883,-5.31838627957415));
#4790=CARTESIAN_POINT('Ctrl Pts',(3.5950153476632,1.26391623423788,-5.32108418100623));
#4791=CARTESIAN_POINT('Ctrl Pts',(3.71404739847578,1.25490736348001,-5.32922380939964));
#4792=CARTESIAN_POINT('Ctrl Pts',(3.79241350516521,1.2414903899723,-5.33473260426232));
#4793=CARTESIAN_POINT('Ctrl Pts',(3.90629091016403,1.2107559904635,-5.34268783329034));
#4794=CARTESIAN_POINT('Ctrl Pts',(3.94309777202561,1.19898972085493,-5.34525373164033));
#4795=CARTESIAN_POINT('Ctrl Pts',(3.97965115673757,1.18542992638994,-5.34779208082771));
#4796=CARTESIAN_POINT('Ctrl Pts',(3.97999094872115,1.18530371137418,-5.34781567595674));
#4797=CARTESIAN_POINT('Ctrl Pts',(3.98033068508385,1.1851773507571,-5.34783926643463));
#4798=CARTESIAN_POINT('Origin',(3.53951905042299,8.32667268468867E-16,-6.5));
#4799=CARTESIAN_POINT('',(3.98033068509731,1.1851773507521,-5.8467115517674));
#4800=CARTESIAN_POINT('',(3.98033068509731,1.1851773507521,-5.70990589948393));
#4801=CARTESIAN_POINT('',(3.98033068509731,1.1851773507521,-6.5));
#4802=CARTESIAN_POINT('',(2.27501908476962,-0.00029472464996097,-5.55658032642993));
#4803=CARTESIAN_POINT('Ctrl Pts',(3.98033068509731,1.1851773507521,-5.70990589948393));
#4804=CARTESIAN_POINT('Ctrl Pts',(3.93266078708269,1.20290756273704,-5.70668826557637));
#4805=CARTESIAN_POINT('Ctrl Pts',(3.88381723853165,1.21779517476562,-5.70347063166882));
#4806=CARTESIAN_POINT('Ctrl Pts',(3.83417275920534,1.22969079117508,-5.70025299776126));
#4807=CARTESIAN_POINT('Ctrl Pts',(3.7861066381084,1.24120820754482,-5.6971376628208));
#4808=CARTESIAN_POINT('Ctrl Pts',(3.7372903345029,1.24992090283827,-5.69402232788034));
#4809=CARTESIAN_POINT('Ctrl Pts',(3.68808057068957,1.25574269844427,-5.69090699293988));
#4810=CARTESIAN_POINT('Ctrl Pts',(3.63891548683514,1.2615592081564,-5.68779448656486));
#4811=CARTESIAN_POINT('Ctrl Pts',(3.58935819208574,1.26448995114612,-5.68468198018984));
#4812=CARTESIAN_POINT('Ctrl Pts',(3.53977466164734,1.26449997416485,-5.68156947381481));
#4813=CARTESIAN_POINT('Ctrl Pts',(3.49021507007097,1.26450999234448,-5.6784584701537));
#4814=CARTESIAN_POINT('Ctrl Pts',(3.44062981503274,1.26160208493541,-5.67534746649258));
#4815=CARTESIAN_POINT('Ctrl Pts',(3.3913864360269,1.25579336618418,-5.67223646283146));
#4816=CARTESIAN_POINT('Ctrl Pts',(3.34214589715217,1.24998498245306,-5.66912563859869));
#4817=CARTESIAN_POINT('Ctrl Pts',(3.2932477386714,1.2412761865991,-5.66601481436593));
#4818=CARTESIAN_POINT('Ctrl Pts',(3.2450533364277,1.22973582255753,-5.66290399013316));
#4819=CARTESIAN_POINT('Ctrl Pts',(3.19680873819873,1.21818343886396,-5.65978992587914));
#4820=CARTESIAN_POINT('Ctrl Pts',(3.14926989168937,1.20379373299775,-5.65667586162512));
#4821=CARTESIAN_POINT('Ctrl Pts',(3.10278512137278,1.18668602638455,-5.65356179737111));
#4822=CARTESIAN_POINT('Ctrl Pts',(3.05627090213853,1.16956748173904,-5.65044576030274));
#4823=CARTESIAN_POINT('Ctrl Pts',(3.01081258962835,1.149727730013,-5.64732972323438));
#4824=CARTESIAN_POINT('Ctrl Pts',(2.96673728188377,1.12733371085455,-5.64421368616602));
#4825=CARTESIAN_POINT('Ctrl Pts',(2.9225839425669,1.10490004499561,-5.64109213241985));
#4826=CARTESIAN_POINT('Ctrl Pts',(2.87981896217944,1.07990337102618,-5.63797057867369));
#4827=CARTESIAN_POINT('Ctrl Pts',(2.83874208093206,1.0525549339731,-5.63484902492752));
#4828=CARTESIAN_POINT('Ctrl Pts',(2.82923971273982,1.04622838457428,-5.63412691185255));
#4829=CARTESIAN_POINT('Ctrl Pts',(2.81982754314012,1.0397761536681,-5.63340479877757));
#4830=CARTESIAN_POINT('Ctrl Pts',(2.81050902345375,1.03320115688007,-5.6326826857026));
#4831=CARTESIAN_POINT('Ctrl Pts',(2.76958968560826,1.00432913385951,-5.62951175406624));
#4832=CARTESIAN_POINT('Ctrl Pts',(2.73029110202993,0.972953837852343,-5.62634082242988));
#4833=CARTESIAN_POINT('Ctrl Pts',(2.69293720100625,0.939286656052421,-5.62316989079352));
#4834=CARTESIAN_POINT('Ctrl Pts',(2.65645656039763,0.906406546455044,-5.62007308927479));
#4835=CARTESIAN_POINT('Ctrl Pts',(2.62183110828954,0.871340933996097,-5.61697628775606));
#4836=CARTESIAN_POINT('Ctrl Pts',(2.58933297529691,0.83433007415321,-5.61387948623733));
#4837=CARTESIAN_POINT('Ctrl Pts',(2.5568668743894,0.797355694406365,-5.61078573710963));
#4838=CARTESIAN_POINT('Ctrl Pts',(2.52652430809794,0.758440276970468,-5.60769198798194));
#4839=CARTESIAN_POINT('Ctrl Pts',(2.49854077772478,0.717861049068864,-5.60459823885425));
#4840=CARTESIAN_POINT('Ctrl Pts',(2.47057254586883,0.677304005716816,-5.60150618107048));
#4841=CARTESIAN_POINT('Ctrl Pts',(2.44496111038932,0.635085410031833,-5.59841412328672));
#4842=CARTESIAN_POINT('Ctrl Pts',(2.42190017579619,0.591513567957594,-5.59532206550296));
#4843=CARTESIAN_POINT('Ctrl Pts',(2.39782180110025,0.546019351952645,-5.59209358724687));
#4844=CARTESIAN_POINT('Ctrl Pts',(2.37652462727331,0.499050215905228,-5.58886510899079));
#4845=CARTESIAN_POINT('Ctrl Pts',(2.35817563284779,0.450985564903965,-5.5856366307347));
#4846=CARTESIAN_POINT('Ctrl Pts',(2.34058627219792,0.40491075222674,-5.5825418089107));
#4847=CARTESIAN_POINT('Ctrl Pts',(2.32570585877347,0.357829942193402,-5.5794469870867));
#4848=CARTESIAN_POINT('Ctrl Pts',(2.31363092908186,0.310094443605026,-5.5763521652627));
#4849=CARTESIAN_POINT('Ctrl Pts',(2.30154836761841,0.262328774535878,-5.57325538740461));
#4850=CARTESIAN_POINT('Ctrl Pts',(2.29227491914344,0.213908139602331,-5.57015860954653));
#4851=CARTESIAN_POINT('Ctrl Pts',(2.28585581517434,0.165193046421117,-5.56706183168844));
#4852=CARTESIAN_POINT('Ctrl Pts',(2.27942574158406,0.116394703907808,-5.56395976173973));
#4853=CARTESIAN_POINT('Ctrl Pts',(2.27585977127268,0.0673014528084192,-5.56085769179101));
#4854=CARTESIAN_POINT('Ctrl Pts',(2.27515112835769,0.0182758762383297,-5.55775562184229));
#4855=CARTESIAN_POINT('Ctrl Pts',(2.27506163276488,0.012084361520348,-5.55736385670483));
#4856=CARTESIAN_POINT('Ctrl Pts',(2.2750176423448,0.00589392001067389,-5.55697209156738));
#4857=CARTESIAN_POINT('Ctrl Pts',(2.27501908476962,-0.000294724649960815,
-5.55658032642993));
#4858=CARTESIAN_POINT('Ctrl Pts',(2.2750190847698,-0.000294725429491894,
-5.55658032638058));
#4859=CARTESIAN_POINT('Ctrl Pts',(2.27502274574772,-0.016001909103677,-5.55558600091698));
#4860=CARTESIAN_POINT('Ctrl Pts',(2.27531905952943,-0.0317053739536449,
-5.55459167545337));
#4861=CARTESIAN_POINT('Ctrl Pts',(2.27590767758865,-0.0473977683410977,
-5.55359734998976));
#4862=CARTESIAN_POINT('Ctrl Pts',(2.27775605165365,-0.096674908838074,-5.55047497654182));
#4863=CARTESIAN_POINT('Ctrl Pts',(2.28249527066355,-0.145951370989865,-5.54735260309388));
#4864=CARTESIAN_POINT('Ctrl Pts',(2.29012341262698,-0.194860951081293,-5.54423022964595));
#4865=CARTESIAN_POINT('Ctrl Pts',(2.2977376142519,-0.2436811494981,-5.54111356229827));
#4866=CARTESIAN_POINT('Ctrl Pts',(2.30823018369446,-0.292135258826107,-5.5379968949506));
#4867=CARTESIAN_POINT('Ctrl Pts',(2.32154730484888,-0.339860378660354,-5.53488022760293));
#4868=CARTESIAN_POINT('Ctrl Pts',(2.33485101052464,-0.387537420886852,-5.53176669994168));
#4869=CARTESIAN_POINT('Ctrl Pts',(2.35097348810582,-0.434486402446487,-5.52865317228042));
#4870=CARTESIAN_POINT('Ctrl Pts',(2.36980995915212,-0.480354964373507,-5.52553964461917));
#4871=CARTESIAN_POINT('Ctrl Pts',(2.38863545658795,-0.526196804536665,-5.52242793081359));
#4872=CARTESIAN_POINT('Ctrl Pts',(2.41017160734413,-0.570958966357735,-5.51931621700801));
#4873=CARTESIAN_POINT('Ctrl Pts',(2.43426475233936,-0.614307078396184,-5.51620450320243));
#4874=CARTESIAN_POINT('Ctrl Pts',(2.45835409572011,-0.657648350613166,-5.51309328038863));
#4875=CARTESIAN_POINT('Ctrl Pts',(2.48499936537833,-0.699575538115731,-5.50998205757484));
#4876=CARTESIAN_POINT('Ctrl Pts',(2.51400121246915,-0.73977930089891,-5.50687083476104));
#4877=CARTESIAN_POINT('Ctrl Pts',(2.54303116976748,-0.780022031410974,-5.5037565963766));
#4878=CARTESIAN_POINT('Ctrl Pts',(2.57442194269341,-0.818537557918219,-5.50064235799216));
#4879=CARTESIAN_POINT('Ctrl Pts',(2.60793219618554,-0.855047474127594,-5.49752811960771));
#4880=CARTESIAN_POINT('Ctrl Pts',(2.64146065504772,-0.891577225356572,-5.49441218932732));
#4881=CARTESIAN_POINT('Ctrl Pts',(2.67711049359016,-0.926098815186914,-5.49129625904692));
#4882=CARTESIAN_POINT('Ctrl Pts',(2.71460409784854,-0.958371311663225,-5.48818032876653));
#4883=CARTESIAN_POINT('Ctrl Pts',(2.75216641403445,-0.990702951705028,-5.48505868813686));
#4884=CARTESIAN_POINT('Ctrl Pts',(2.79157880363042,-1.02077694043359,-5.4819370475072));
#4885=CARTESIAN_POINT('Ctrl Pts',(2.83253258454186,-1.04839419449981,-5.47881540687754));
#4886=CARTESIAN_POINT('Ctrl Pts',(2.8513517695631,-1.0610849449625,-5.47738094267736));
#4887=CARTESIAN_POINT('Ctrl Pts',(2.87049606900254,-1.0732575561212,-5.47594647847717));
#4888=CARTESIAN_POINT('Ctrl Pts',(2.88993386662373,-1.08489600376648,-5.47451201427699));
#4889=CARTESIAN_POINT('Ctrl Pts',(2.93224490233421,-1.11022988075866,-5.4713895583701));
#4890=CARTESIAN_POINT('Ctrl Pts',(2.97613231701829,-1.13314001524391,-5.4682671024632));
#4891=CARTESIAN_POINT('Ctrl Pts',(3.02128805141708,-1.15342831665836,-5.46514464655631));
#4892=CARTESIAN_POINT('Ctrl Pts',(3.06636157543434,-1.17367968125798,-5.46202787538236));
#4893=CARTESIAN_POINT('Ctrl Pts',(3.11269834367567,-1.19131845758046,-5.45891110420842));
#4894=CARTESIAN_POINT('Ctrl Pts',(3.15996476984413,-1.20619185791244,-5.45579433303447));
#4895=CARTESIAN_POINT('Ctrl Pts',(3.20718378070552,-1.2210503379955,-5.45268068844898));
#4896=CARTESIAN_POINT('Ctrl Pts',(3.25533008322022,-1.23314877058989,-5.44956704386349));
#4897=CARTESIAN_POINT('Ctrl Pts',(3.30405114133481,-1.24238283704728,-5.44645339927799));
#4898=CARTESIAN_POINT('Ctrl Pts',(3.35274401589305,-1.25161156189587,-5.44334155583518));
#4899=CARTESIAN_POINT('Ctrl Pts',(3.40201045025828,-1.25797910157165,-5.44022971239238));
#4900=CARTESIAN_POINT('Ctrl Pts',(3.45148633478003,-1.26143192086475,-5.43711786894957));
#4901=CARTESIAN_POINT('Ctrl Pts',(3.50095460919738,-1.26488420906445,-5.43400650415315));
#4902=CARTESIAN_POINT('Ctrl Pts',(3.5506317237145,-1.26542263006767,-5.43089513935673));
#4903=CARTESIAN_POINT('Ctrl Pts',(3.60014963877545,-1.26304559765514,-5.42778377456031));
#4904=CARTESIAN_POINT('Ctrl Pts',(3.64971582044746,-1.26066624827715,-5.42466937702242));
#4905=CARTESIAN_POINT('Ctrl Pts',(3.69912194490598,-1.25536579956374,-5.42155497948453));
#4906=CARTESIAN_POINT('Ctrl Pts',(3.7480030070167,-1.24719472811708,-5.41844058194665));
#4907=CARTESIAN_POINT('Ctrl Pts',(3.79691078113621,-1.23901919142922,-5.41532448248554));
#4908=CARTESIAN_POINT('Ctrl Pts',(3.84529238718609,-1.22797003034951,-5.41220838302444));
#4909=CARTESIAN_POINT('Ctrl Pts',(3.89279445080751,-1.21414856647906,-5.40909228356333));
#4910=CARTESIAN_POINT('Ctrl Pts',(3.94038376461397,-1.2003017158109,-5.40597046055605));
#4911=CARTESIAN_POINT('Ctrl Pts',(3.98708979596454,-1.18367258409638,-5.40284863754878));
#4912=CARTESIAN_POINT('Ctrl Pts',(4.03257730729884,-1.16441135571865,-5.3997268145415));
#4913=CARTESIAN_POINT('Ctrl Pts',(4.05346280524401,-1.1555676020398,-5.39829343588236));
#4914=CARTESIAN_POINT('Ctrl Pts',(4.07409174376038,-1.14616960703868,-5.39686005722323));
#4915=CARTESIAN_POINT('Ctrl Pts',(4.0944335217213,-1.13623508991041,-5.3954266785641));
#4916=CARTESIAN_POINT('Ctrl Pts',(4.13867888344531,-1.1146265410049,-5.3923089394273));
#4917=CARTESIAN_POINT('Ctrl Pts',(4.18175845816928,-1.09038172784545,-5.3891912002905));
#4918=CARTESIAN_POINT('Ctrl Pts',(4.22333876640782,-1.06364977602142,-5.3860734611537));
#4919=CARTESIAN_POINT('Ctrl Pts',(4.26484300037015,-1.03696673229772,-5.38296142615327));
#4920=CARTESIAN_POINT('Ctrl Pts',(4.30485294930259,-1.00780586895283,-5.37984939115284));
#4921=CARTESIAN_POINT('Ctrl Pts',(4.34305908348303,-0.976362466131235,-5.37673735615241));
#4922=CARTESIAN_POINT('Ctrl Pts',(4.3812267346318,-0.944950734597319,-5.37362845574133));
#4923=CARTESIAN_POINT('Ctrl Pts',(4.41759374531062,-0.911261362163879,-5.37051955533026));
#4924=CARTESIAN_POINT('Ctrl Pts',(4.4518808051329,-0.875531997440788,-5.36741065491918));
#4925=CARTESIAN_POINT('Ctrl Pts',(4.48614801060192,-0.839823322255751,-5.364303554756));
#4926=CARTESIAN_POINT('Ctrl Pts',(4.51833727133104,-0.802077390582719,-5.36119645459281));
#4927=CARTESIAN_POINT('Ctrl Pts',(4.54820548565155,-0.762569292186549,-5.35808935442962));
#4928=CARTESIAN_POINT('Ctrl Pts',(4.57806919277791,-0.723067155669058,-5.35498272313624));
#4929=CARTESIAN_POINT('Ctrl Pts',(4.60561221858689,-0.681803819158794,-5.35187609184285));
#4930=CARTESIAN_POINT('Ctrl Pts',(4.63063283820331,-0.639086028728283,-5.34876946054947));
#4931=CARTESIAN_POINT('Ctrl Pts',(4.6556783001173,-0.596325824957177,-5.34565974476576));
#4932=CARTESIAN_POINT('Ctrl Pts',(4.67819607889475,-0.552108760000173,-5.34255002898205));
#4933=CARTESIAN_POINT('Ctrl Pts',(4.69802973222386,-0.506767451750091,-5.33944031319835));
#4934=CARTESIAN_POINT('Ctrl Pts',(4.71787438600363,-0.461400995595288,-5.33632887265549));
#4935=CARTESIAN_POINT('Ctrl Pts',(4.73503176028608,-0.414909570772984,-5.33321743211263));
#4936=CARTESIAN_POINT('Ctrl Pts',(4.74939437995943,-0.367643763688562,-5.33010599156978));
#4937=CARTESIAN_POINT('Ctrl Pts',(4.76378382985173,-0.320289661294376,-5.32698873867284));
#4938=CARTESIAN_POINT('Ctrl Pts',(4.7753679784059,-0.272158824256545,-5.32387148577591));
#4939=CARTESIAN_POINT('Ctrl Pts',(4.78409020431963,-0.223613266351477,-5.32075423287897));
#4940=CARTESIAN_POINT('Ctrl Pts',(4.78820603162296,-0.200705681217004,-5.31928326953642));
#4941=CARTESIAN_POINT('Ctrl Pts',(4.79168534827568,-0.177705835991882,-5.31781230619386));
#4942=CARTESIAN_POINT('Ctrl Pts',(4.79452622970454,-0.154651963944089,-5.31634134285131));
#4943=CARTESIAN_POINT('Ctrl Pts',(4.80056628812567,-0.105636636311179,-5.31321389640666));
#4944=CARTESIAN_POINT('Ctrl Pts',(4.80374356326664,-0.0561614284076493,
-5.31008644996201));
#4945=CARTESIAN_POINT('Ctrl Pts',(4.80400188255505,-0.00658917622266315,
-5.30695900351735));
#4946=CARTESIAN_POINT('Ctrl Pts',(4.80425972737876,0.0428920247533582,-5.30383730137051));
#4947=CARTESIAN_POINT('Ctrl Pts',(4.80160924873279,0.092469374936108,-5.30071559922367));
#4948=CARTESIAN_POINT('Ctrl Pts',(4.79604603805036,0.141775101354518,-5.29759389707683));
#4949=CARTESIAN_POINT('Ctrl Pts',(4.79048847306251,0.191030791006713,-5.29447536291659));
#4950=CARTESIAN_POINT('Ctrl Pts',(4.78202408983974,0.240014862905859,-5.29135682875634));
#4951=CARTESIAN_POINT('Ctrl Pts',(4.77070046785673,0.288361868779224,-5.2882382945961));
#4952=CARTESIAN_POINT('Ctrl Pts',(4.75938356895954,0.336680169961623,-5.28512161197884));
#4953=CARTESIAN_POINT('Ctrl Pts',(4.7452109192292,0.384361624174091,-5.28200492936157));
#4954=CARTESIAN_POINT('Ctrl Pts',(4.72828121689885,0.431050764476334,-5.27888824674431));
#4955=CARTESIAN_POINT('Ctrl Pts',(4.71135443753347,0.477731843755436,-5.27577210223185));
#4956=CARTESIAN_POINT('Ctrl Pts',(4.69167173757609,0.523420436840053,-5.27265595771939));
#4957=CARTESIAN_POINT('Ctrl Pts',(4.66938091360084,0.567778495662066,-5.26953981320693));
#4958=CARTESIAN_POINT('Ctrl Pts',(4.64706929923758,0.612177926721152,-5.26642076230332));
#4959=CARTESIAN_POINT('Ctrl Pts',(4.62214495041812,0.655243857716199,-5.26330171139971));
#4960=CARTESIAN_POINT('Ctrl Pts',(4.59480205087727,0.696662069408267,-5.2601826604961));
#4961=CARTESIAN_POINT('Ctrl Pts',(4.56744481033775,0.738102004418964,-5.25706197369046));
#4962=CARTESIAN_POINT('Ctrl Pts',(4.53766681944526,0.77789206113148,-5.25394128688483));
#4963=CARTESIAN_POINT('Ctrl Pts',(4.50570408803224,0.815749179037295,-5.25082060007919));
#4964=CARTESIAN_POINT('Ctrl Pts',(4.47368430213115,0.853673873097775,-5.24769434274875));
#4965=CARTESIAN_POINT('Ctrl Pts',(4.4394723684359,0.889658346260538,-5.2445680854183));
#4966=CARTESIAN_POINT('Ctrl Pts',(4.40334168380365,0.923455850628115,-5.24144182808786));
#4967=CARTESIAN_POINT('Ctrl Pts',(4.38721627028579,0.938539947133523,-5.24004655443806));
#4968=CARTESIAN_POINT('Ctrl Pts',(4.37070910220634,0.95318895592024,-5.23865128078826));
#4969=CARTESIAN_POINT('Ctrl Pts',(4.35384646135687,0.967383645614151,-5.23725600713846));
#4970=CARTESIAN_POINT('Ctrl Pts',(4.31608428534962,0.999171215270337,-5.23413143314009));
#4971=CARTESIAN_POINT('Ctrl Pts',(4.27637765767766,1.02881208577837,-5.23100685914173));
#4972=CARTESIAN_POINT('Ctrl Pts',(4.23499993142354,1.05606183254708,-5.22788228514336));
#4973=CARTESIAN_POINT('Ctrl Pts',(4.19368748929417,1.08326858575311,-5.22476264097312));
#4974=CARTESIAN_POINT('Ctrl Pts',(4.15070962524876,1.10809139224436,-5.22164299680288));
#4975=CARTESIAN_POINT('Ctrl Pts',(4.10637220230447,1.13032639277424,-5.21852335263265));
#4976=CARTESIAN_POINT('Ctrl Pts',(4.06542982508554,1.15085879449505,-5.21564258871077));
#4977=CARTESIAN_POINT('Ctrl Pts',(4.02332876222096,1.16918476310038,-5.2127618247889));
#4978=CARTESIAN_POINT('Ctrl Pts',(3.98033068509731,1.1851773507521,-5.20988106086703));
#4979=CARTESIAN_POINT('',(2.27501952462653,0.00109510754574143,-5.69341967361942));
#4980=CARTESIAN_POINT('Ctrl Pts',(3.98033068508385,1.1851773507571,-5.34783926643463));
#4981=CARTESIAN_POINT('Ctrl Pts',(4.01383899306308,1.17271436198533,-5.35016600294365));
#4982=CARTESIAN_POINT('Ctrl Pts',(4.0468062752844,1.15883497555727,-5.35244677809117));
#4983=CARTESIAN_POINT('Ctrl Pts',(4.11262314463296,1.12777762618674,-5.35699420702988));
#4984=CARTESIAN_POINT('Ctrl Pts',(4.14539459441361,1.11051606334499,-5.35925521350175));
#4985=CARTESIAN_POINT('Ctrl Pts',(4.21235649313321,1.07139739845899,-5.36390131317071));
#4986=CARTESIAN_POINT('Ctrl Pts',(4.24634763115312,1.04928373059564,-5.36627499860472));
#4987=CARTESIAN_POINT('Ctrl Pts',(4.35505663752254,0.97087676199841,-5.37402900391421));
#4988=CARTESIAN_POINT('Ctrl Pts',(4.42458507856987,0.907941949608262,-5.37924200727832));
#4989=CARTESIAN_POINT('Ctrl Pts',(4.50588853312012,0.816053420441164,-5.38652725672441));
#4990=CARTESIAN_POINT('Ctrl Pts',(4.52447588503683,0.793519309361531,-5.38829391937243));
#4991=CARTESIAN_POINT('Ctrl Pts',(4.55452196213696,0.754409780389055,-5.39136623261555));
#4992=CARTESIAN_POINT('Ctrl Pts',(4.56639404836727,0.738168401294929,-5.39264571877438));
#4993=CARTESIAN_POINT('Ctrl Pts',(4.5985072796071,0.691961975534618,-5.39629287469257));
#4994=CARTESIAN_POINT('Ctrl Pts',(4.61785633603671,0.661404295057555,-5.39870838581128));
#4995=CARTESIAN_POINT('Ctrl Pts',(4.6658382957047,0.577912698047838,-5.40523711375543));
#4996=CARTESIAN_POINT('Ctrl Pts',(4.692049014446,0.523691383273651,-5.40940152559124));
#4997=CARTESIAN_POINT('Ctrl Pts',(4.74009679133558,0.403032350044958,-5.41829767247082));
#4998=CARTESIAN_POINT('Ctrl Pts',(4.76049353314704,0.336222944703702,-5.42299589415376));
#4999=CARTESIAN_POINT('Ctrl Pts',(4.78278760168466,0.233448391232862,-5.4298190597256));
#5000=CARTESIAN_POINT('Ctrl Pts',(4.78883921860845,0.198530528253468,-5.43207143502346));
#5001=CARTESIAN_POINT('Ctrl Pts',(4.79832045384951,0.125774158497969,-5.43664203584638));
#5002=CARTESIAN_POINT('Ctrl Pts',(4.80152802478373,0.0879426534074953,-5.43895106809916));
#5003=CARTESIAN_POINT('Ctrl Pts',(4.80471082561513,0.00754626257473869,
-5.44375345981939));
#5004=CARTESIAN_POINT('Ctrl Pts',(4.8042496130601,-0.03498833550617,-5.44623230076327));
#5005=CARTESIAN_POINT('Ctrl Pts',(4.79639705344158,-0.163001369958141,-5.45362764700549));
#5006=CARTESIAN_POINT('Ctrl Pts',(4.78245737643129,-0.247818402955921,-5.45842909637968));
#5007=CARTESIAN_POINT('Ctrl Pts',(4.75210217012925,-0.359897005900358,-5.46530399947366));
#5008=CARTESIAN_POINT('Ctrl Pts',(4.74310411347431,-0.388929738538274,-5.46713695065838));
#5009=CARTESIAN_POINT('Ctrl Pts',(4.72644682058844,-0.436537430765181,-5.47027283083785));
#5010=CARTESIAN_POINT('Ctrl Pts',(4.71937551365201,-0.455303229163825,-5.47154534477018));
#5011=CARTESIAN_POINT('Ctrl Pts',(4.6989965656696,-0.505717745451123,-5.47506323219359));
#5012=CARTESIAN_POINT('Ctrl Pts',(4.68484280513477,-0.537002417496111,-5.47735002698292));
#5013=CARTESIAN_POINT('Ctrl Pts',(4.6450535440025,-0.616200873231293,-5.48334451660414));
#5014=CARTESIAN_POINT('Ctrl Pts',(4.61757073058802,-0.663109578273905,-5.48709603000919));
#5015=CARTESIAN_POINT('Ctrl Pts',(4.54326497476591,-0.773044751477453,-5.49620791905494));
#5016=CARTESIAN_POINT('Ctrl Pts',(4.49342271089991,-0.833771799768242,-5.50151597657881));
#5017=CARTESIAN_POINT('Ctrl Pts',(4.41331640010028,-0.914711308259354,-5.50890506251307));
#5018=CARTESIAN_POINT('Ctrl Pts',(4.38731162387462,-0.938864607305538,-5.51116097468996));
#5019=CARTESIAN_POINT('Ctrl Pts',(4.33142469063804,-0.986554067352629,-5.51573797273894));
#5020=CARTESIAN_POINT('Ctrl Pts',(4.30142770909568,-1.00990054807934,-5.51804987940183));
#5021=CARTESIAN_POINT('Ctrl Pts',(4.23568619295422,-1.05646748778856,-5.5228589219122));
#5022=CARTESIAN_POINT('Ctrl Pts',(4.19972804002095,-1.07930382153396,-5.52534149384131));
#5023=CARTESIAN_POINT('Ctrl Pts',(4.07025073296527,-1.15263558984765,-5.53392298603898));
#5024=CARTESIAN_POINT('Ctrl Pts',(3.97160330547309,-1.19312259814339,-5.53981654639278));
#5025=CARTESIAN_POINT('Ctrl Pts',(3.84840599039205,-1.22637981534584,-5.54761004845566));
#5026=CARTESIAN_POINT('Ctrl Pts',(3.82759943302925,-1.23143340518724,-5.54894173074041));
#5027=CARTESIAN_POINT('Ctrl Pts',(3.78257944721993,-1.24116462084355,-5.55187437396506));
#5028=CARTESIAN_POINT('Ctrl Pts',(3.75833873242266,-1.24566677385104,-5.55348273678575));
#5029=CARTESIAN_POINT('Ctrl Pts',(3.70336636963696,-1.25422265243101,-5.55717295482336));
#5030=CARTESIAN_POINT('Ctrl Pts',(3.67258562310545,-1.25786066508259,-5.55926892668274));
#5031=CARTESIAN_POINT('Ctrl Pts',(3.55207131652317,-1.26763149215377,-5.56752107953678));
#5032=CARTESIAN_POINT('Ctrl Pts',(3.46190730505992,-1.26531673700144,-5.5737704961506));
#5033=CARTESIAN_POINT('Ctrl Pts',(3.32776485139802,-1.24746938802161,-5.5828114653218));
#5034=CARTESIAN_POINT('Ctrl Pts',(3.28313081164288,-1.23906642879302,-5.58578072864624));
#5035=CARTESIAN_POINT('Ctrl Pts',(3.20590422952255,-1.22017421867164,-5.59085023275138));
#5036=CARTESIAN_POINT('Ctrl Pts',(3.1731073338312,-1.21072985681481,-5.59298144935432));
#5037=CARTESIAN_POINT('Ctrl Pts',(3.09551783294056,-1.18494432674075,-5.59799123775252));
#5038=CARTESIAN_POINT('Ctrl Pts',(3.05118816882779,-1.16737476305348,-5.60082602558441));
#5039=CARTESIAN_POINT('Ctrl Pts',(2.94812926422528,-1.11962730013014,-5.60745846739225));
#5040=CARTESIAN_POINT('Ctrl Pts',(2.89056595536774,-1.08727518220347,-5.61119511748772));
#5041=CARTESIAN_POINT('Ctrl Pts',(2.78830352015497,-1.01877465912023,-5.61825812801595));
#5042=CARTESIAN_POINT('Ctrl Pts',(2.74303612497406,-0.983788655790435,-5.62156687198817));
#5043=CARTESIAN_POINT('Ctrl Pts',(2.6838519083931,-0.931277190323247,-5.62638363008584));
#5044=CARTESIAN_POINT('Ctrl Pts',(2.66779300593776,-0.916262556773373,-5.6277464693398));
#5045=CARTESIAN_POINT('Ctrl Pts',(2.63526749049333,-0.884222773535953,-5.63064569291508));
#5046=CARTESIAN_POINT('Ctrl Pts',(2.61887199637917,-0.867138748811013,-5.63218557213672));
#5047=CARTESIAN_POINT('Ctrl Pts',(2.58341112486266,-0.828048932372558,-5.63567575042531));
#5048=CARTESIAN_POINT('Ctrl Pts',(2.56460649859647,-0.805824236301561,-5.63763806522961));
#5049=CARTESIAN_POINT('Ctrl Pts',(2.4998858357199,-0.723748207857147,-5.64475426343522));
#5050=CARTESIAN_POINT('Ctrl Pts',(2.45857653552093,-0.660464077423448,-5.64999271959722));
#5051=CARTESIAN_POINT('Ctrl Pts',(2.39697872910789,-0.544672047145205,-5.65888001056765));
#5052=CARTESIAN_POINT('Ctrl Pts',(2.37408386428528,-0.493789726746075,-5.66257995845826));
#5053=CARTESIAN_POINT('Ctrl Pts',(2.3425910548086,-0.409279923580441,-5.66838528776535));
#5054=CARTESIAN_POINT('Ctrl Pts',(2.33188615171131,-0.376523359957652,-5.67055834010406));
#5055=CARTESIAN_POINT('Ctrl Pts',(2.31136088024728,-0.303776268951802,-5.67523297503839));
#5056=CARTESIAN_POINT('Ctrl Pts',(2.30212821130146,-0.263660698190303,-5.67771323638318));
#5057=CARTESIAN_POINT('Ctrl Pts',(2.28159558261087,-0.149143516307408,-5.68459356816637));
#5058=CARTESIAN_POINT('Ctrl Pts',(2.27495355791553,-0.0740900462670108,
-5.68886124052725));
#5059=CARTESIAN_POINT('Ctrl Pts',(2.27501953713604,0.00110945800815503,
-5.69316916139296));
#5060=CARTESIAN_POINT('Ctrl Pts',(2.27501952462653,0.00109510754574143,
-5.69341967361942));
#5061=CARTESIAN_POINT('Ctrl Pts',(2.27508084679143,0.0719026266169531,-5.69788243689888));
#5062=CARTESIAN_POINT('Ctrl Pts',(2.28109314086155,0.142459189162486,-5.70234520017833));
#5063=CARTESIAN_POINT('Ctrl Pts',(2.29291052307184,0.211960915112676,-5.70680796345778));
#5064=CARTESIAN_POINT('Ctrl Pts',(2.29497479482244,0.224101543802159,-5.70758752326244));
#5065=CARTESIAN_POINT('Ctrl Pts',(2.29721609154514,0.236210054463847,-5.7083670830671));
#5066=CARTESIAN_POINT('Ctrl Pts',(2.29963349906839,0.248282237669356,-5.70914664287175));
#5067=CARTESIAN_POINT('Ctrl Pts',(2.30931421785275,0.296626345810645,-5.71226845794507));
#5068=CARTESIAN_POINT('Ctrl Pts',(2.321847798193,0.344509128671207,-5.71539027301839));
#5069=CARTESIAN_POINT('Ctrl Pts',(2.33717400774133,0.391569468088145,-5.71851208809171));
#5070=CARTESIAN_POINT('Ctrl Pts',(2.35247223362812,0.438543881457545,-5.7216282031375));
#5071=CARTESIAN_POINT('Ctrl Pts',(2.37055280714682,0.484698312959515,-5.72474431818329));
#5072=CARTESIAN_POINT('Ctrl Pts',(2.3913047909112,0.529683173466743,-5.72786043322908));
#5073=CARTESIAN_POINT('Ctrl Pts',(2.41203589391428,0.574622769957512,-5.73097341282261));
#5074=CARTESIAN_POINT('Ctrl Pts',(2.43543285718586,0.61839463009274,-5.73408639241614));
#5075=CARTESIAN_POINT('Ctrl Pts',(2.46133611263667,0.660667694583638,-5.73719937200966));
#5076=CARTESIAN_POINT('Ctrl Pts',(2.48722431832861,0.702916198477182,-5.74031054296596));
#5077=CARTESIAN_POINT('Ctrl Pts',(2.51561564556851,0.743667165597622,-5.74342171392225));
#5078=CARTESIAN_POINT('Ctrl Pts',(2.54630513890367,0.78261508799952,-5.74653288487854));
#5079=CARTESIAN_POINT('Ctrl Pts',(2.57698985019277,0.821556941524459,-5.74964357105125));
#5080=CARTESIAN_POINT('Ctrl Pts',(2.60997167677727,0.858695878713766,-5.75275425722395));
#5081=CARTESIAN_POINT('Ctrl Pts',(2.64500455080803,0.893758390158439,-5.75586494339665));
#5082=CARTESIAN_POINT('Ctrl Pts',(2.6800715380493,0.928855043673001,-5.75897865859552));
#5083=CARTESIAN_POINT('Ctrl Pts',(2.71719317121231,0.961870847335929,-5.76209237379439));
#5084=CARTESIAN_POINT('Ctrl Pts',(2.75608686802635,0.992569526826832,-5.76520608899327));
#5085=CARTESIAN_POINT('Ctrl Pts',(2.79500178536475,1.02328495561465,-5.76832150304503));
#5086=CARTESIAN_POINT('Ctrl Pts',(2.83569024184058,1.05168042901441,-5.77143691709679));
#5087=CARTESIAN_POINT('Ctrl Pts',(2.87783982272104,1.07756245741384,-5.77455233114855));
#5088=CARTESIAN_POINT('Ctrl Pts',(2.92006688462982,1.10349206318257,-5.77767347207776));
#5089=CARTESIAN_POINT('Ctrl Pts',(2.96375994793821,1.12689874468181,-5.78079461300698));
#5090=CARTESIAN_POINT('Ctrl Pts',(3.00858260762519,1.14763528340201,-5.78391575393619));
#5091=CARTESIAN_POINT('Ctrl Pts',(3.02924435418254,1.1571941340036,-5.78535449548566));
#5092=CARTESIAN_POINT('Ctrl Pts',(3.05014586513611,1.1661862863862,-5.78679323703512));
#5093=CARTESIAN_POINT('Ctrl Pts',(3.07125306164386,1.17460087423461,-5.78823197858459));
#5094=CARTESIAN_POINT('Ctrl Pts',(3.11704109100752,1.19285471459395,-5.79135305344118));
#5095=CARTESIAN_POINT('Ctrl Pts',(3.16399811037257,1.20846708514513,-5.79447412829778));
#5096=CARTESIAN_POINT('Ctrl Pts',(3.21178884403069,1.2212915957371,-5.79759520315438));
#5097=CARTESIAN_POINT('Ctrl Pts',(3.25950731526502,1.23409671490842,-5.80071155876068));
#5098=CARTESIAN_POINT('Ctrl Pts',(3.30805648012053,1.2441221799778,-5.80382791436698));
#5099=CARTESIAN_POINT('Ctrl Pts',(3.3570827507601,1.25127025320884,-5.80694426997328));
#5100=CARTESIAN_POINT('Ctrl Pts',(3.4060557416028,1.25841055819879,-5.81005723884852));
#5101=CARTESIAN_POINT('Ctrl Pts',(3.4555042712478,1.26267958835051,-5.81317020772375));
#5102=CARTESIAN_POINT('Ctrl Pts',(3.50506384158547,1.26403049353406,-5.81628317659899));
#5103=CARTESIAN_POINT('Ctrl Pts',(3.55460065781235,1.26538077848128,-5.8193947162278));
#5104=CARTESIAN_POINT('Ctrl Pts',(3.60424786719166,1.26381557054246,-5.82250625585661));
#5105=CARTESIAN_POINT('Ctrl Pts',(3.65363749481286,1.2593399980347,-5.82561779548543));
#5106=CARTESIAN_POINT('Ctrl Pts',(3.70301483436451,1.25486553904306,-5.82872856096758));
#5107=CARTESIAN_POINT('Ctrl Pts',(3.75213417445898,1.24748220834006,-5.83183932644973));
#5108=CARTESIAN_POINT('Ctrl Pts',(3.80063203620425,1.23724704835227,-5.83495009193188));
#5109=CARTESIAN_POINT('Ctrl Pts',(3.84915605933676,1.22700636717293,-5.83806253546616));
#5110=CARTESIAN_POINT('Ctrl Pts',(3.89705740105416,1.21391090970786,-5.84117497900045));
#5111=CARTESIAN_POINT('Ctrl Pts',(3.9439843271744,1.19806848297683,-5.84428742253473));
#5112=CARTESIAN_POINT('Ctrl Pts',(3.95616735230715,1.19395552056942,-5.84509546561229));
#5113=CARTESIAN_POINT('Ctrl Pts',(3.96828478884944,1.18965766858197,-5.84590350868984));
#5114=CARTESIAN_POINT('Ctrl Pts',(3.98033068509731,1.1851773507521,-5.8467115517674));
#5115=CARTESIAN_POINT('Origin',(3.53951905042299,8.32667268468867E-16,-6.5));
#5116=CARTESIAN_POINT('',(3.98033068509731,1.1851773507521,-6.346783713414));
#5117=CARTESIAN_POINT('',(3.98033068509731,1.1851773507521,-6.20995736687868));
#5118=CARTESIAN_POINT('',(3.98033068509731,1.1851773507521,-6.5));
#5119=CARTESIAN_POINT('',(4.4976352031454,-0.825211298936473,-6.5));
#5120=CARTESIAN_POINT('Ctrl Pts',(3.98033068509731,1.1851773507521,-6.346783713414));
#5121=CARTESIAN_POINT('Ctrl Pts',(4.02616495548084,1.16812987710687,-6.34987250303372));
#5122=CARTESIAN_POINT('Ctrl Pts',(4.07110586500492,1.1483834254578,-6.35296129265343));
#5123=CARTESIAN_POINT('Ctrl Pts',(4.1148117000608,1.12605444685091,-6.35605008227315));
#5124=CARTESIAN_POINT('Ctrl Pts',(4.15843020115214,1.10377008650205,-6.35913269980525));
#5125=CARTESIAN_POINT('Ctrl Pts',(4.20081803353623,1.0789137028647,-6.36221531733735));
#5126=CARTESIAN_POINT('Ctrl Pts',(4.24165368460605,1.05164975418655,-6.36529793486946));
#5127=CARTESIAN_POINT('Ctrl Pts',(4.28245834983294,1.02440649322634,-6.36837821333018));
#5128=CARTESIAN_POINT('Ctrl Pts',(4.32171269959968,0.994759591665204,-6.3714584917909));
#5129=CARTESIAN_POINT('Ctrl Pts',(4.35912171531297,0.962918335948197,-6.37453877025163));
#5130=CARTESIAN_POINT('Ctrl Pts',(4.39651904341382,0.931087028321222,-6.37761808634806));
#5131=CARTESIAN_POINT('Ctrl Pts',(4.43207175366471,0.897063087696465,-6.3806974024445));
#5132=CARTESIAN_POINT('Ctrl Pts',(4.46551781507142,0.86109612580105,-6.38377671854093));
#5133=CARTESIAN_POINT('Ctrl Pts',(4.49913236819104,0.824947972615459,-6.38687154735312));
#5134=CARTESIAN_POINT('Ctrl Pts',(4.5306185831317,0.786837569042,-6.3899663761653));
#5135=CARTESIAN_POINT('Ctrl Pts',(4.55974993405299,0.747053675506357,-6.39306120497749));
#5136=CARTESIAN_POINT('Ctrl Pts',(4.58877680192034,0.70741247163537,-6.39614493381815));
#5137=CARTESIAN_POINT('Ctrl Pts',(4.61546539872469,0.666110259798259,-6.39922866265882));
#5138=CARTESIAN_POINT('Ctrl Pts',(4.63963574546676,0.623460910792302,-6.40231239149948));
#5139=CARTESIAN_POINT('Ctrl Pts',(4.66393659500647,0.580581285430692,-6.40541277029743));
#5140=CARTESIAN_POINT('Ctrl Pts',(4.68569167562811,0.536340448700378,-6.40851314909538));
#5141=CARTESIAN_POINT('Ctrl Pts',(4.70476677812757,0.49107838791715,-6.41161352789333));
#5142=CARTESIAN_POINT('Ctrl Pts',(4.72384188062704,0.445816327133923,-6.41471390669127));
#5143=CARTESIAN_POINT('Ctrl Pts',(4.74023689245796,0.399533602083208,-6.41781428548922));
#5144=CARTESIAN_POINT('Ctrl Pts',(4.75386885489192,0.352583043248368,-6.42091466428717));
#5145=CARTESIAN_POINT('Ctrl Pts',(4.76835751896294,0.302681873244369,-6.42420988660854));
#5146=CARTESIAN_POINT('Ctrl Pts',(4.77979240021909,0.251794251730069,-6.42750510892991));
#5147=CARTESIAN_POINT('Ctrl Pts',(4.78805146309887,0.200317409372577,-6.43080033125128));
#5148=CARTESIAN_POINT('Ctrl Pts',(4.79607098831799,0.150333550247694,-6.43399998221574));
#5149=CARTESIAN_POINT('Ctrl Pts',(4.8010963166219,0.0997947297249169,-6.43719963318019));
#5150=CARTESIAN_POINT('Ctrl Pts',(4.80306622942805,0.0490792871622248,-6.44039928414465));
#5151=CARTESIAN_POINT('Ctrl Pts',(4.80503359056896,-0.00157046273056229,
-6.44359479054083));
#5152=CARTESIAN_POINT('Ctrl Pts',(4.80395336896427,-0.0523958723376958,
-6.44679029693701));
#5153=CARTESIAN_POINT('Ctrl Pts',(4.79981605772876,-0.103013122349091,-6.44998580333318));
#5154=CARTESIAN_POINT('Ctrl Pts',(4.79568270901791,-0.153581893508067,-6.45317824922167));
#5155=CARTESIAN_POINT('Ctrl Pts',(4.78849812398825,-0.20394239251437,-6.45637069511015));
#5156=CARTESIAN_POINT('Ctrl Pts',(4.778304816312,-0.253712585873823,-6.45956314099864));
#5157=CARTESIAN_POINT('Ctrl Pts',(4.76811783502728,-0.303451889777174,-6.46275360552217));
#5158=CARTESIAN_POINT('Ctrl Pts',(4.75492594267193,-0.352601115387661,-6.46594407004569));
#5159=CARTESIAN_POINT('Ctrl Pts',(4.73882294389742,-0.400787251664849,-6.46913453456922));
#5160=CARTESIAN_POINT('Ctrl Pts',(4.72271981198959,-0.448973786326264,-6.47232502547027));
#5161=CARTESIAN_POINT('Ctrl Pts',(4.70370567730319,-0.496196727080413,-6.47551551637131));
#5162=CARTESIAN_POINT('Ctrl Pts',(4.68192401564236,-0.542098833647634,-6.47870600727236));
#5163=CARTESIAN_POINT('Ctrl Pts',(4.66014245444853,-0.588000728493317,-6.4818964834574));
#5164=CARTESIAN_POINT('Ctrl Pts',(4.63559361893804,-0.632581342776674,-6.48508695964244));
#5165=CARTESIAN_POINT('Ctrl Pts',(4.6084678042507,-0.675506337268713,-6.48827743582748));
#5166=CARTESIAN_POINT('Ctrl Pts',(4.58132277162687,-0.718461743006546,-6.49147017238218));
#5167=CARTESIAN_POINT('Ctrl Pts',(4.55159739891111,-0.7597587613696,-6.49466290893689));
#5168=CARTESIAN_POINT('Ctrl Pts',(4.51952538136017,-0.799091885406837,-6.4978556454916));
#5169=CARTESIAN_POINT('Ctrl Pts',(4.5123451485358,-0.807897723326088,-6.49857043032773));
#5170=CARTESIAN_POINT('Ctrl Pts',(4.50504745829283,-0.816605259011897,-6.49928521516387));
#5171=CARTESIAN_POINT('Ctrl Pts',(4.49763520314539,-0.825211298936477,-6.5));
#5172=CARTESIAN_POINT('',(2.58129066896548,-0.825080977219403,-6.49999893616038));
#5173=CARTESIAN_POINT('Origin',(3.53951905042299,8.32667268468867E-16,-6.5));
#5174=CARTESIAN_POINT('Ctrl Pts',(2.58129066896548,-0.825080977219403,-6.49999893616038));
#5175=CARTESIAN_POINT('Ctrl Pts',(2.61412671854531,-0.863215942769539,-6.49681298227165));
#5176=CARTESIAN_POINT('Ctrl Pts',(2.64931926798332,-0.899476323465664,-6.49362702838292));
#5177=CARTESIAN_POINT('Ctrl Pts',(2.68662301217427,-0.933556960200953,-6.49044107449419));
#5178=CARTESIAN_POINT('Ctrl Pts',(2.72294455751986,-0.966740261755096,-6.48733900602497));
#5179=CARTESIAN_POINT('Ctrl Pts',(2.7612670549967,-0.997856790145826,-6.48423693755575));
#5180=CARTESIAN_POINT('Ctrl Pts',(2.80132380814607,-1.02665867467222,-6.48113486908654));
#5181=CARTESIAN_POINT('Ctrl Pts',(2.84134145438787,-1.05543244027864,-6.478035829128));
#5182=CARTESIAN_POINT('Ctrl Pts',(2.88308955800233,-1.08189571288545,-6.47493678916947));
#5183=CARTESIAN_POINT('Ctrl Pts',(2.92626824205562,-1.10584071910776,-6.47183774921094));
#5184=CARTESIAN_POINT('Ctrl Pts',(2.96942356684567,-1.12977277130621,-6.46874038580397));
#5185=CARTESIAN_POINT('Ctrl Pts',(3.01400745582359,-1.15118898787877,-6.465643022397));
#5186=CARTESIAN_POINT('Ctrl Pts',(3.05969320088253,-1.16992623874874,-6.46254565899003));
#5187=CARTESIAN_POINT('Ctrl Pts',(3.10764213745995,-1.18959170009648,-6.45929485764343));
#5188=CARTESIAN_POINT('Ctrl Pts',(3.1568043809889,-1.20630549959918,-6.45604405629683));
#5189=CARTESIAN_POINT('Ctrl Pts',(3.20677870465072,-1.21993610992353,-6.45279325495023));
#5190=CARTESIAN_POINT('Ctrl Pts',(3.2544370462731,-1.23293503088453,-6.44969310691879));
#5191=CARTESIAN_POINT('Ctrl Pts',(3.30283326198768,-1.24313020620206,-6.44659295888735));
#5192=CARTESIAN_POINT('Ctrl Pts',(3.35160723959285,-1.2504596760194,-6.44349281085591));
#5193=CARTESIAN_POINT('Ctrl Pts',(3.4004119123784,-1.25779375853,-6.44039071179223));
#5194=CARTESIAN_POINT('Ctrl Pts',(3.44959426890379,-1.2622584995746,-6.43728861272854));
#5195=CARTESIAN_POINT('Ctrl Pts',(3.49879002678772,-1.26384389725698,-6.43418651366486));
#5196=CARTESIAN_POINT('Ctrl Pts',(3.54806997554175,-1.26543200810034,-6.43107910584224));
#5197=CARTESIAN_POINT('Ctrl Pts',(3.59736281976622,-1.26413097060597,-6.42797169801961));
#5198=CARTESIAN_POINT('Ctrl Pts',(3.64630722476824,-1.25998275219148,-6.42486429019699));
#5199=CARTESIAN_POINT('Ctrl Pts',(3.65328091267178,-1.25939170648202,-6.42442154107494));
#5200=CARTESIAN_POINT('Ctrl Pts',(3.66024754291994,-1.25874294487555,-6.42397879195289));
#5201=CARTESIAN_POINT('Ctrl Pts',(3.66720608834692,-1.258036672894,-6.42353604283084));
#5202=CARTESIAN_POINT('Ctrl Pts',(3.7163503009999,-1.25304867923693,-6.42040915988751));
#5203=CARTESIAN_POINT('Ctrl Pts',(3.76530520024984,-1.24516622469272,-6.41728227694418));
#5204=CARTESIAN_POINT('Ctrl Pts',(3.81370450644581,-1.23441588846934,-6.41415539400084));
#5205=CARTESIAN_POINT('Ctrl Pts',(3.86201822470779,-1.22368456282978,-6.41103404054692));
#5206=CARTESIAN_POINT('Ctrl Pts',(3.90977776996751,-1.21009553271363,-6.40791268709299));
#5207=CARTESIAN_POINT('Ctrl Pts',(3.95662365314126,-1.19372693711386,-6.40479133363907));
#5208=CARTESIAN_POINT('Ctrl Pts',(4.00342399311994,-1.17737425493255,-6.40167301474015));
#5209=CARTESIAN_POINT('Ctrl Pts',(4.04931191683946,-1.15824753723455,-6.39855469584123));
#5210=CARTESIAN_POINT('Ctrl Pts',(4.09394188046512,-1.13647506595089,-6.39543637694231));
#5211=CARTESIAN_POINT('Ctrl Pts',(4.13854724887414,-1.11471459330232,-6.39231977652404));
#5212=CARTESIAN_POINT('Ctrl Pts',(4.18189554117391,-1.09031149514611,-6.38920317610577));
#5213=CARTESIAN_POINT('Ctrl Pts',(4.22366242409282,-1.06344162710685,-6.3860865756875));
#5214=CARTESIAN_POINT('Ctrl Pts',(4.26542387626861,-1.03657525282487,-6.38297038050551));
#5215=CARTESIAN_POINT('Ctrl Pts',(4.30560386937867,-1.00724304192177,-6.37985418532352));
#5216=CARTESIAN_POINT('Ctrl Pts',(4.34390607352076,-0.975664782121349,-6.37673799014153));
#5217=CARTESIAN_POINT('Ctrl Pts',(4.3822464430242,-0.944055056881205,-6.37361868989764));
#5218=CARTESIAN_POINT('Ctrl Pts',(4.41870486724809,-0.91019516380421,-6.37049938965374));
#5219=CARTESIAN_POINT('Ctrl Pts',(4.45301863913752,-0.874344755470276,-6.36738008940984));
#5220=CARTESIAN_POINT('Ctrl Pts',(4.48735166185403,-0.838474234220356,-6.36425903916568));
#5221=CARTESIAN_POINT('Ctrl Pts',(4.5195372825782,-0.800611390248026,-6.36113798892153));
#5222=CARTESIAN_POINT('Ctrl Pts',(4.54935255743518,-0.761049629206565,-6.35801693867737));
#5223=CARTESIAN_POINT('Ctrl Pts',(4.57922266965563,-0.721415104701414,-6.35489014808142));
#5224=CARTESIAN_POINT('Ctrl Pts',(4.60671343338299,-0.680075881820579,-6.35176335748547));
#5225=CARTESIAN_POINT('Ctrl Pts',(4.63164568014743,-0.637353649590818,-6.34863656688951));
#5226=CARTESIAN_POINT('Ctrl Pts',(4.64277134670996,-0.618289450720728,-6.34724128029902));
#5227=CARTESIAN_POINT('Ctrl Pts',(4.65338816691601,-0.598950168489519,-6.34584599370852));
#5228=CARTESIAN_POINT('Ctrl Pts',(4.66348329935251,-0.579365702409359,-6.34445070711802));
#5229=CARTESIAN_POINT('Ctrl Pts',(4.68604213954088,-0.535601755452205,-6.34133276414798));
#5230=CARTESIAN_POINT('Ctrl Pts',(4.70609159237177,-0.490420275785111,-6.33821482117794));
#5231=CARTESIAN_POINT('Ctrl Pts',(4.72345315202669,-0.444139947606419,-6.3350968782079));
#5232=CARTESIAN_POINT('Ctrl Pts',(4.74078251756512,-0.397945438576851,-6.33198471694303));
#5233=CARTESIAN_POINT('Ctrl Pts',(4.75543368336745,-0.350656632335413,-6.32887255567816));
#5234=CARTESIAN_POINT('Ctrl Pts',(4.76727490792033,-0.302614944080707,-6.32576039441329));
#5235=CARTESIAN_POINT('Ctrl Pts',(4.77910402283558,-0.254622386507843,-6.32265141585516));
#5236=CARTESIAN_POINT('Ctrl Pts',(4.78812875400986,-0.205879001956756,-6.31954243729703));
#5237=CARTESIAN_POINT('Ctrl Pts',(4.79426689094177,-0.15674216635436,-6.31643345873889));
#5238=CARTESIAN_POINT('Ctrl Pts',(4.80040137886605,-0.107634541681869,-6.31332632841038));
#5239=CARTESIAN_POINT('Ctrl Pts',(4.80365260386734,-0.0581344735108271,
-6.31021919808186));
#5240=CARTESIAN_POINT('Ctrl Pts',(4.80398975244913,-0.00860777076329439,
-6.30711206775334));
#5241=CARTESIAN_POINT('Ctrl Pts',(4.8043268449561,0.0409106946627478,-6.30400545420527));
#5242=CARTESIAN_POINT('Ctrl Pts',(4.80175082049702,0.0904552366909444,-6.3008988406572));
#5243=CARTESIAN_POINT('Ctrl Pts',(4.7962829578317,0.139659339232284,-6.29779222710913));
#5244=CARTESIAN_POINT('Ctrl Pts',(4.79080979264191,0.188911158033825,-6.29468260088583));
#5245=CARTESIAN_POINT('Ctrl Pts',(4.78243925225903,0.237821331195318,-6.29157297466254));
#5246=CARTESIAN_POINT('Ctrl Pts',(4.77124438860737,0.286029616079496,-6.28846334843925));
#5247=CARTESIAN_POINT('Ctrl Pts',(4.76004346383081,0.334264001901106,-6.28535203860162));
#5248=CARTESIAN_POINT('Ctrl Pts',(4.74601532686642,0.381795215322045,-6.282240728764));
#5249=CARTESIAN_POINT('Ctrl Pts',(4.72928304450845,0.42827781681733,-6.27912941892637));
#5250=CARTESIAN_POINT('Ctrl Pts',(4.71251983522219,0.474846333912903,-6.27601235833376));
#5251=CARTESIAN_POINT('Ctrl Pts',(4.69304272248403,0.520361865968394,-6.27289529774114));
#5252=CARTESIAN_POINT('Ctrl Pts',(4.67102239639318,0.564500157713225,-6.26977823714853));
#5253=CARTESIAN_POINT('Ctrl Pts',(4.66063090310688,0.585329220845309,-6.26830728190075));
#5254=CARTESIAN_POINT('Ctrl Pts',(4.64967370496905,0.605851960151309,-6.26683632665297));
#5255=CARTESIAN_POINT('Ctrl Pts',(4.63817208739712,0.626036543939347,-6.26536537140519));
#5256=CARTESIAN_POINT('Ctrl Pts',(4.61376229710427,0.668874123465282,-6.26224357493579));
#5257=CARTESIAN_POINT('Ctrl Pts',(4.58679013796971,0.710375291807168,-6.25912177846638));
#5258=CARTESIAN_POINT('Ctrl Pts',(4.55742651536473,0.750216397325387,-6.25599998199698));
#5259=CARTESIAN_POINT('Ctrl Pts',(4.52810762303525,0.789996811979615,-6.25288294103129));
#5260=CARTESIAN_POINT('Ctrl Pts',(4.49640480327601,0.82812173430381,-6.24976590006559));
#5261=CARTESIAN_POINT('Ctrl Pts',(4.46253361238668,0.864294144607594,-6.24664885909989));
#5262=CARTESIAN_POINT('Ctrl Pts',(4.42869624467415,0.900430433777259,-6.2435349307566));
#5263=CARTESIAN_POINT('Ctrl Pts',(4.39269516505254,0.934617672677172,-6.24042100241331));
#5264=CARTESIAN_POINT('Ctrl Pts',(4.35478626440368,0.966591754469368,-6.23730707407002));
#5265=CARTESIAN_POINT('Ctrl Pts',(4.31690142905875,0.998545538495526,-6.23419512250872));
#5266=CARTESIAN_POINT('Ctrl Pts',(4.27711159225709,1.02828859884005,-6.23108317094741));
#5267=CARTESIAN_POINT('Ctrl Pts',(4.235707637073,1.05559542525452,-6.22797121938611));
#5268=CARTESIAN_POINT('Ctrl Pts',(4.19428956444941,1.08291156243333,-6.22485820674773));
#5269=CARTESIAN_POINT('Ctrl Pts',(4.15125672490063,1.10778949401323,-6.22174519410934));
#5270=CARTESIAN_POINT('Ctrl Pts',(4.10692943142985,1.13004677315838,-6.21863218147096));
#5271=CARTESIAN_POINT('Ctrl Pts',(4.06575484195602,1.1507210408578,-6.21574057660687));
#5272=CARTESIAN_POINT('Ctrl Pts',(4.0234639866436,1.16913446809706,-6.21284897174278));
#5273=CARTESIAN_POINT('Ctrl Pts',(3.98033068509731,1.1851773507521,-6.20995736687868));
#5274=CARTESIAN_POINT('Origin',(3.53951905042299,8.32667268468867E-16,-6.5));
#5275=CARTESIAN_POINT('',(2.27501933211556,-0.00084403816866925,-6.05658032632122));
#5276=CARTESIAN_POINT('Ctrl Pts',(3.98033068509731,1.1851773507521,-6.20995736687868));
#5277=CARTESIAN_POINT('Ctrl Pts',(3.93385133118698,1.20246475500667,-6.20684144667251));
#5278=CARTESIAN_POINT('Ctrl Pts',(3.88639406205051,1.21699885353846,-6.20372552646634));
#5279=CARTESIAN_POINT('Ctrl Pts',(3.83831564831889,1.22869070277505,-6.20060960626016));
#5280=CARTESIAN_POINT('Ctrl Pts',(3.79014801406301,1.24040424891961,-6.19748790374936));
#5281=CARTESIAN_POINT('Ctrl Pts',(3.7413574735584,1.24926491911046,-6.19436620123856));
#5282=CARTESIAN_POINT('Ctrl Pts',(3.69230960462601,1.25523515587572,-6.19124449872775));
#5283=CARTESIAN_POINT('Ctrl Pts',(3.66630922700763,1.25839999083688,-6.18958967771596));
#5284=CARTESIAN_POINT('Ctrl Pts',(3.64023660268906,1.26075347117176,-6.18793485670416));
#5285=CARTESIAN_POINT('Ctrl Pts',(3.61414616017263,1.26229594172302,-6.18628003569237));
#5286=CARTESIAN_POINT('Ctrl Pts',(3.56491893879061,1.26520626182413,-6.18315773371363));
#5287=CARTESIAN_POINT('Ctrl Pts',(3.51541402755449,1.26523895392596,-6.18003543173489));
#5288=CARTESIAN_POINT('Ctrl Pts',(3.4659961307317,1.26236073698451,-6.17691312975614));
#5289=CARTESIAN_POINT('Ctrl Pts',(3.41666811577358,1.25948775497862,-6.17379650665777));
#5290=CARTESIAN_POINT('Ctrl Pts',(3.36742734378295,1.25371439647113,-6.17067988355939));
#5291=CARTESIAN_POINT('Ctrl Pts',(3.31864021813992,1.24505935258094,-6.16756326046101));
#5292=CARTESIAN_POINT('Ctrl Pts',(3.26990197615981,1.23641298086076,-6.16444976015274));
#5293=CARTESIAN_POINT('Ctrl Pts',(3.22161701740165,1.22489073538295,-6.16133625984446));
#5294=CARTESIAN_POINT('Ctrl Pts',(3.17414614658414,1.21056304715631,-6.15822275953619));
#5295=CARTESIAN_POINT('Ctrl Pts',(3.12670267433917,1.19624362838414,-6.15511105623442));
#5296=CARTESIAN_POINT('Ctrl Pts',(3.08007288253499,1.1791221328155,-6.15199935293266));
#5297=CARTESIAN_POINT('Ctrl Pts',(3.0346043656427,1.15931937406964,-6.1488876496309));
#5298=CARTESIAN_POINT('Ctrl Pts',(2.989142777331,1.13951963290648,-6.1457764204965));
#5299=CARTESIAN_POINT('Ctrl Pts',(2.94484261399633,1.11703965943637,-6.14266519136211));
#5300=CARTESIAN_POINT('Ctrl Pts',(2.90203094213092,1.09204814993946,-6.13955396222772));
#5301=CARTESIAN_POINT('Ctrl Pts',(2.85917742828406,1.06703221499427,-6.13643969233397));
#5302=CARTESIAN_POINT('Ctrl Pts',(2.81781578352711,1.03950012118479,-6.13332542244023));
#5303=CARTESIAN_POINT('Ctrl Pts',(2.77824631821777,1.00966532930511,-6.13021115254648));
#5304=CARTESIAN_POINT('Ctrl Pts',(2.73865517234765,0.979814190603118,-6.12709517630878));
#5305=CARTESIAN_POINT('Ctrl Pts',(2.70085857873599,0.947658196795133,-6.12397920007109));
#5306=CARTESIAN_POINT('Ctrl Pts',(2.66512302989052,0.913450518242225,-6.12086322383339));
#5307=CARTESIAN_POINT('Ctrl Pts',(2.62932174457812,0.879179913779319,-6.11774151567676));
#5308=CARTESIAN_POINT('Ctrl Pts',(2.5955894429348,0.842850494239972,-6.11461980752013));
#5309=CARTESIAN_POINT('Ctrl Pts',(2.56415394704208,0.804750374406088,-6.11149809936351));
#5310=CARTESIAN_POINT('Ctrl Pts',(2.54970891813782,0.787242862066077,-6.11006363290218));
#5311=CARTESIAN_POINT('Ctrl Pts',(2.53574827647228,0.769361887651816,-6.10862916644086));
#5312=CARTESIAN_POINT('Ctrl Pts',(2.52229100852905,0.751137378103785,-6.10719469997954));
#5313=CARTESIAN_POINT('Ctrl Pts',(2.49287301930624,0.71129805650176,-6.10405891349764));
#5314=CARTESIAN_POINT('Ctrl Pts',(2.4657340203538,0.669640051077935,-6.10092312701574));
#5315=CARTESIAN_POINT('Ctrl Pts',(2.4411031690058,0.626452553231681,-6.09778734053384));
#5316=CARTESIAN_POINT('Ctrl Pts',(2.41651339891891,0.583337086873545,-6.094656784162));
#5317=CARTESIAN_POINT('Ctrl Pts',(2.3944237547299,0.538697647781062,-6.09152622779015));
#5318=CARTESIAN_POINT('Ctrl Pts',(2.37502105402754,0.492853595290712,-6.08839567141831));
#5319=CARTESIAN_POINT('Ctrl Pts',(2.35564416242351,0.44707052367499,-6.08526927925219));
#5320=CARTESIAN_POINT('Ctrl Pts',(2.33894733547462,0.400086512493713,-6.08214288708606));
#5321=CARTESIAN_POINT('Ctrl Pts',(2.32507100364992,0.352244505548458,-6.07901649491994));
#5322=CARTESIAN_POINT('Ctrl Pts',(2.3112053781611,0.304439411283135,-6.07589251493342));
#5323=CARTESIAN_POINT('Ctrl Pts',(2.30015608341166,0.255778152169922,-6.0727685349469));
#5324=CARTESIAN_POINT('Ctrl Pts',(2.29201423199374,0.206620371686356,-6.06964455496038));
#5325=CARTESIAN_POINT('Ctrl Pts',(2.28387383969977,0.157471400906018,-6.06652113483105));
#5326=CARTESIAN_POINT('Ctrl Pts',(2.27863995220415,0.107826617675868,-6.06339771470171));
#5327=CARTESIAN_POINT('Ctrl Pts',(2.27635245514721,0.0580551684123632,-6.06027429457238));
#5328=CARTESIAN_POINT('Ctrl Pts',(2.27545067216389,0.038434139452019,-6.05904297184178));
#5329=CARTESIAN_POINT('Ctrl Pts',(2.27500622432079,0.0187934877093903,-6.05781164911118));
#5330=CARTESIAN_POINT('Ctrl Pts',(2.27501933211493,-0.000844037222033078,
-6.05658032638058));
#5331=CARTESIAN_POINT('Ctrl Pts',(2.27501933211556,-0.000844038168669184,
-6.05658032632122));
#5332=CARTESIAN_POINT('Ctrl Pts',(2.27505698654879,-0.0572562029046497,
-6.05304314019587));
#5333=CARTESIAN_POINT('Ctrl Pts',(2.27887371445784,-0.113521864639994,-6.04950595407052));
#5334=CARTESIAN_POINT('Ctrl Pts',(2.2863868355746,-0.16917417683907,-6.04596876794517));
#5335=CARTESIAN_POINT('Ctrl Pts',(2.29396582199884,-0.225314376375244,-6.04240057235675));
#5336=CARTESIAN_POINT('Ctrl Pts',(2.30530616689083,-0.280830190252909,-6.03883237676834));
#5337=CARTESIAN_POINT('Ctrl Pts',(2.32027339706781,-0.335261519972844,-6.03526418117992));
#5338=CARTESIAN_POINT('Ctrl Pts',(2.3302773135162,-0.371642765417343,-6.03287924220886));
#5339=CARTESIAN_POINT('Ctrl Pts',(2.34190049367822,-0.407539927551625,-6.03049430323779));
#5340=CARTESIAN_POINT('Ctrl Pts',(2.35509102814013,-0.442821081285782,-6.02810936426672));
#5341=CARTESIAN_POINT('Ctrl Pts',(2.3723573653824,-0.489003917957764,-6.02498749223829));
#5342=CARTESIAN_POINT('Ctrl Pts',(2.39236660219172,-0.534276316559383,-6.02186562020986));
#5343=CARTESIAN_POINT('Ctrl Pts',(2.41500167232912,-0.578291376699397,-6.01874374818142));
#5344=CARTESIAN_POINT('Ctrl Pts',(2.43759542894926,-0.622226100576454,-6.01562757419206));
#5345=CARTESIAN_POINT('Ctrl Pts',(2.46280526458397,-0.66490755431047,-6.01251140020269));
#5346=CARTESIAN_POINT('Ctrl Pts',(2.4904658960776,-0.706008306861882,-6.00939522621333));
#5347=CARTESIAN_POINT('Ctrl Pts',(2.51809870624658,-0.747067719887846,-6.00628218650122));
#5348=CARTESIAN_POINT('Ctrl Pts',(2.54817712765057,-0.786549126907373,-6.00316914678911));
#5349=CARTESIAN_POINT('Ctrl Pts',(2.58049082464027,-0.824151146424035,-6.000056107077));
#5350=CARTESIAN_POINT('Ctrl Pts',(2.61278575862353,-0.861731332260242,-5.99694487495701));
#5351=CARTESIAN_POINT('Ctrl Pts',(2.64731304035497,-0.897433877815161,-5.99383364283702));
#5352=CARTESIAN_POINT('Ctrl Pts',(2.68382160328835,-0.930989865125965,-5.99072241071704));
#5353=CARTESIAN_POINT('Ctrl Pts',(2.72032448831636,-0.964540633723522,-5.98761166246385));
#5354=CARTESIAN_POINT('Ctrl Pts',(2.75880763883495,-0.995945137171808,-5.98450091421067));
#5355=CARTESIAN_POINT('Ctrl Pts',(2.79898450572692,-1.02497260359084,-5.98139016595749));
#5356=CARTESIAN_POINT('Ctrl Pts',(2.83920050514222,-1.05402834294638,-5.97827638781576));
#5357=CARTESIAN_POINT('Ctrl Pts',(2.88111306881727,-1.08070210253111,-5.97516260967404));
#5358=CARTESIAN_POINT('Ctrl Pts',(2.92440553907012,-1.10480569248676,-5.97204883153231));
#5359=CARTESIAN_POINT('Ctrl Pts',(2.96772163741902,-1.12892243766167,-5.96893335395767));
#5360=CARTESIAN_POINT('Ctrl Pts',(3.01241864799431,-1.15046598192878,-5.96581787638303));
#5361=CARTESIAN_POINT('Ctrl Pts',(3.05815728581959,-1.16929513022928,-5.96270239880838));
#5362=CARTESIAN_POINT('Ctrl Pts',(3.10398000247744,-1.18815889112172,-5.95958119422197));
#5363=CARTESIAN_POINT('Ctrl Pts',(3.15084764941867,-1.20429811992803,-5.95645998963555));
#5364=CARTESIAN_POINT('Ctrl Pts',(3.19840463755624,-1.2176211263503,-5.95333878504913));
#5365=CARTESIAN_POINT('Ctrl Pts',(3.22031891432334,-1.22376037236947,-5.95190053288405));
#5366=CARTESIAN_POINT('Ctrl Pts',(3.24237941204166,-1.22930234408423,-5.95046228071898));
#5367=CARTESIAN_POINT('Ctrl Pts',(3.26455079222824,-1.23424175386564,-5.9490240285539));
#5368=CARTESIAN_POINT('Ctrl Pts',(3.31267501798266,-1.24496302017447,-5.94590222146288));
#5369=CARTESIAN_POINT('Ctrl Pts',(3.36153242312082,-1.2528888973427,-5.94278041437187));
#5370=CARTESIAN_POINT('Ctrl Pts',(3.41076841946522,-1.25792826704386,-5.93965860728085));
#5371=CARTESIAN_POINT('Ctrl Pts',(3.45991456907007,-1.26295844081175,-5.93654249692006));
#5372=CARTESIAN_POINT('Ctrl Pts',(3.5094373989117,-1.26511249897277,-5.93342638655928));
#5373=CARTESIAN_POINT('Ctrl Pts',(3.55897233558323,-1.26435035480537,-5.93031027619849));
#5374=CARTESIAN_POINT('Ctrl Pts',(3.6084574623759,-1.2635889770124,-5.92719729924394));
#5375=CARTESIAN_POINT('Ctrl Pts',(3.6579541266216,-1.25991721067633,-5.92408432228939));
#5376=CARTESIAN_POINT('Ctrl Pts',(3.7070950113436,-1.25334693813067,-5.92097134533484));
#5377=CARTESIAN_POINT('Ctrl Pts',(3.75620737743784,-1.24678047860463,-5.91786017497843));
#5378=CARTESIAN_POINT('Ctrl Pts',(3.80496383097999,-1.23731891793616,-5.91474900462202));
#5379=CARTESIAN_POINT('Ctrl Pts',(3.85300204483451,-1.22502598430188,-5.91163783426561));
#5380=CARTESIAN_POINT('Ctrl Pts',(3.90103280477825,-1.21273495811634,-5.90852714665792));
#5381=CARTESIAN_POINT('Ctrl Pts',(3.9483450160688,-1.19761356809752,-5.90541645905024));
#5382=CARTESIAN_POINT('Ctrl Pts',(3.994588967302,-1.17977608924394,-5.90230577144255));
#5383=CARTESIAN_POINT('Ctrl Pts',(4.04087799371517,-1.16192122373658,-5.89919205176688));
#5384=CARTESIAN_POINT('Ctrl Pts',(4.08609616954537,-1.14134518260638,-5.89607833209122));
#5385=CARTESIAN_POINT('Ctrl Pts',(4.12991304844692,-1.11821070335483,-5.89296461241555));
#5386=CARTESIAN_POINT('Ctrl Pts',(4.17375385850482,-1.09506358890759,-5.88984919214153));
#5387=CARTESIAN_POINT('Ctrl Pts',(4.21619137863636,-1.06935553811172,-5.8867337718675));
#5388=CARTESIAN_POINT('Ctrl Pts',(4.25692220755705,-1.04129388749482,-5.88361835159347));
#5389=CARTESIAN_POINT('Ctrl Pts',(4.2977279433308,-1.01318062953295,-5.88049720184291));
#5390=CARTESIAN_POINT('Ctrl Pts',(4.33682029192501,-0.982705470712209,-5.87737605209235));
#5391=CARTESIAN_POINT('Ctrl Pts',(4.37392844987612,-0.950116416079766,-5.87425490234178));
#5392=CARTESIAN_POINT('Ctrl Pts',(4.39103396084727,-0.935094047351874,-5.87281616584154));
#5393=CARTESIAN_POINT('Ctrl Pts',(4.40771837197739,-0.919623019014169,-5.87137742934131));
#5394=CARTESIAN_POINT('Ctrl Pts',(4.42395795142166,-0.903730092671621,-5.86993869284107));
#5395=CARTESIAN_POINT('Ctrl Pts',(4.45919242271407,-0.869247742996835,-5.86681711447206));
#5396=CARTESIAN_POINT('Ctrl Pts',(4.49248440852953,-0.83262626144501,-5.86369553610306));
#5397=CARTESIAN_POINT('Ctrl Pts',(4.52356411872374,-0.794113060938407,-5.86057395773406));
#5398=CARTESIAN_POINT('Ctrl Pts',(4.55458706730217,-0.755670198008187,-5.85745808037806));
#5399=CARTESIAN_POINT('Ctrl Pts',(4.58340541236112,-0.715342891540266,-5.85434220302206));
#5400=CARTESIAN_POINT('Ctrl Pts',(4.60978668200981,-0.673414765785208,-5.85122632566606));
#5401=CARTESIAN_POINT('Ctrl Pts',(4.6361414012232,-0.631528837013262,-5.84811358416748));
#5402=CARTESIAN_POINT('Ctrl Pts',(4.66006361025982,-0.588045740121642,-5.8450008426689));
#5403=CARTESIAN_POINT('Ctrl Pts',(4.68136289272615,-0.543279752792577,-5.84188810117032));
#5404=CARTESIAN_POINT('Ctrl Pts',(4.70264979966691,-0.498539775852419,-5.83877716826843));
#5405=CARTESIAN_POINT('Ctrl Pts',(4.72131656430274,-0.452518879168679,-5.83566623536655));
#5406=CARTESIAN_POINT('Ctrl Pts',(4.73721894244515,-0.405555444606648,-5.83255530246467));
#5407=CARTESIAN_POINT('Ctrl Pts',(4.75311884496686,-0.358599321130413,-5.82944485386079));
#5408=CARTESIAN_POINT('Ctrl Pts',(4.76625504083263,-0.310701470233705,-5.82633440525691));
#5409=CARTESIAN_POINT('Ctrl Pts',(4.77653253037065,-0.262217277134401,-5.82322395665302));
#5410=CARTESIAN_POINT('Ctrl Pts',(4.78682003688283,-0.213685828826787,-5.82011047644467));
#5411=CARTESIAN_POINT('Ctrl Pts',(4.79424316182307,-0.164567434723309,-5.81699699623631));
#5412=CARTESIAN_POINT('Ctrl Pts',(4.79875803108361,-0.115227772627966,-5.81388351602795));
#5413=CARTESIAN_POINT('Ctrl Pts',(4.80327536551357,-0.0658611705219124,
-5.81076833582437));
#5414=CARTESIAN_POINT('Ctrl Pts',(4.80488126460168,-0.0162736080643454,
-5.80765315562078));
#5415=CARTESIAN_POINT('Ctrl Pts',(4.8035839862753,0.0331675737536573,-5.80453797541719));
#5416=CARTESIAN_POINT('Ctrl Pts',(4.80228432121647,0.0826997174496432,-5.80141706390559));
#5417=CARTESIAN_POINT('Ctrl Pts',(4.79807086613848,0.13208439691815,-5.79829615239399));
#5418=CARTESIAN_POINT('Ctrl Pts',(4.79100374597293,0.180959406509492,-5.79517524088239));
#5419=CARTESIAN_POINT('Ctrl Pts',(4.78774152896586,0.203520348417172,-5.79373461296434));
#5420=CARTESIAN_POINT('Ctrl Pts',(4.78387197165841,0.225972841006474,-5.7922939850463));
#5421=CARTESIAN_POINT('Ctrl Pts',(4.7794045979522,0.248282256772818,-5.79085335712825));
#5422=CARTESIAN_POINT('Ctrl Pts',(4.76972387646597,0.296626374537997,-5.78773154136868));
#5423=CARTESIAN_POINT('Ctrl Pts',(4.75719029232652,0.344509166555588,-5.78460972560912));
#5424=CARTESIAN_POINT('Ctrl Pts',(4.74186407797352,0.391569514549487,-5.78148790984956));
#5425=CARTESIAN_POINT('Ctrl Pts',(4.7265658473038,0.438543936440369,-5.77837179412143));
#5426=CARTESIAN_POINT('Ctrl Pts',(4.70848526800516,0.484698375887524,-5.77525567839329));
#5427=CARTESIAN_POINT('Ctrl Pts',(4.68773327755313,0.529683243661652,-5.77213956266516));
#5428=CARTESIAN_POINT('Ctrl Pts',(4.66700216788444,0.574622847378835,-5.76902658239227));
#5429=CARTESIAN_POINT('Ctrl Pts',(4.64360519704529,0.618394714065538,-5.76591360211939));
#5430=CARTESIAN_POINT('Ctrl Pts',(4.61770193321154,0.660667784337773,-5.7628006218465));
#5431=CARTESIAN_POINT('Ctrl Pts',(4.59181371917313,0.702916293957703,-5.75968945021504));
#5432=CARTESIAN_POINT('Ctrl Pts',(4.56342238277836,0.743667266039175,-5.75657827858358));
#5433=CARTESIAN_POINT('Ctrl Pts',(4.53273287956449,0.782615192544894,-5.75346710695212));
#5434=CARTESIAN_POINT('Ctrl Pts',(4.50204815845055,0.821557050106605,-5.75035642010966));
#5435=CARTESIAN_POINT('Ctrl Pts',(4.46906632132525,0.858695990482074,-5.74724573326721));
#5436=CARTESIAN_POINT('Ctrl Pts',(4.43403343612197,0.893758504170771,-5.74413504642475));
#5437=CARTESIAN_POINT('Ctrl Pts',(4.39896643785363,0.928855159775088,-5.74102133056935));
#5438=CARTESIAN_POINT('Ctrl Pts',(4.36184479304868,0.961870964602486,-5.73790761471396));
#5439=CARTESIAN_POINT('Ctrl Pts',(4.32295108406249,0.992569644240386,-5.73479389885856));
#5440=CARTESIAN_POINT('Ctrl Pts',(4.2840361546326,1.02328507310636,-5.7316784841569));
#5441=CARTESIAN_POINT('Ctrl Pts',(4.24334768554216,1.05168054557615,-5.72856306945525));
#5442=CARTESIAN_POINT('Ctrl Pts',(4.20119809161407,1.07756257194116,-5.72544765475359));
#5443=CARTESIAN_POINT('Ctrl Pts',(4.15897101688686,1.10349217551627,-5.722326513192));
#5444=CARTESIAN_POINT('Ctrl Pts',(4.11527794034272,1.12689885374361,-5.71920537163041));
#5445=CARTESIAN_POINT('Ctrl Pts',(4.07045526709899,1.14763538801389,-5.71608423006883));
#5446=CARTESIAN_POINT('Ctrl Pts',(4.0497935950466,1.1571941992045,-5.71464549385102));
#5447=CARTESIAN_POINT('Ctrl Pts',(4.02889216040453,1.16618631635696,-5.71320675763322));
#5448=CARTESIAN_POINT('Ctrl Pts',(4.00778504162465,1.17460087326884,-5.71176802141541));
#5449=CARTESIAN_POINT('Ctrl Pts',(3.99867889501626,1.17823112662949,-5.71114731410492));
#5450=CARTESIAN_POINT('Ctrl Pts',(3.98952658961544,1.18175705108102,-5.71052660679442));
#5451=CARTESIAN_POINT('Ctrl Pts',(3.98033068509731,1.1851773507521,-5.70990589948393));
#5452=CARTESIAN_POINT('',(2.27501930025681,-0.000794877133459826,-6.19341967365965));
#5453=CARTESIAN_POINT('Ctrl Pts',(3.98033068509731,1.1851773507521,-5.8467115517674));
#5454=CARTESIAN_POINT('Ctrl Pts',(4.02678408443536,1.16789959997042,-5.84982766259815));
#5455=CARTESIAN_POINT('Ctrl Pts',(4.07217160066956,1.14790474819601,-5.8529437734289));
#5456=CARTESIAN_POINT('Ctrl Pts',(4.1161668623606,1.12536107582747,-5.85605988425965));
#5457=CARTESIAN_POINT('Ctrl Pts',(4.16023964775348,1.10277767943258,-5.85918148596458));
#5458=CARTESIAN_POINT('Ctrl Pts',(4.20291481653079,1.07763678585611,-5.86230308766952));
#5459=CARTESIAN_POINT('Ctrl Pts',(4.2438935636827,1.05015084396012,-5.86542468937446));
#5460=CARTESIAN_POINT('Ctrl Pts',(4.2521753588957,1.04459594153289,-5.86605556434877));
#5461=CARTESIAN_POINT('Ctrl Pts',(4.26038797288695,1.03894538892574,-5.86668643932309));
#5462=CARTESIAN_POINT('Ctrl Pts',(4.26852910855665,1.03320113489096,-5.8673173142974));
#5463=CARTESIAN_POINT('Ctrl Pts',(4.30880622153057,1.00478225353377,-5.87043847867099));
#5464=CARTESIAN_POINT('Ctrl Pts',(4.34750735369413,0.973942382796071,-5.87355964304458));
#5465=CARTESIAN_POINT('Ctrl Pts',(4.38432675561076,0.940882666040445,-5.87668080741817));
#5466=CARTESIAN_POINT('Ctrl Pts',(4.42107892076406,0.907883320399928,-5.87979627216115));
#5467=CARTESIAN_POINT('Ctrl Pts',(4.45595576640711,0.872672532001327,-5.88291173690413));
#5468=CARTESIAN_POINT('Ctrl Pts',(4.48868260359977,0.835493147381136,-5.88602720164711));
#5469=CARTESIAN_POINT('Ctrl Pts',(4.5213765124808,0.798351171030969,-5.88913953174578));
#5470=CARTESIAN_POINT('Ctrl Pts',(4.55192433502822,0.759244929232485,-5.89225186184445));
#5471=CARTESIAN_POINT('Ctrl Pts',(4.5800880081899,0.718454239413951,-5.89536419194312));
#5472=CARTESIAN_POINT('Ctrl Pts',(4.60823533313529,0.677687227438016,-5.89847471542213));
#5473=CARTESIAN_POINT('Ctrl Pts',(4.63400093956425,0.635238154809938,-5.90158523890114));
#5474=CARTESIAN_POINT('Ctrl Pts',(4.65718850053871,0.59141799962296,-5.90469576238015));
#5475=CARTESIAN_POINT('Ctrl Pts',(4.68037247173167,0.54760462845189,-5.90780580430357));
#5476=CARTESIAN_POINT('Ctrl Pts',(4.70097893465621,0.502421080937199,-5.91091584622699));
#5477=CARTESIAN_POINT('Ctrl Pts',(4.71885746514283,0.456202974087311,-5.91402588815041));
#5478=CARTESIAN_POINT('Ctrl Pts',(4.73675346520262,0.40993970633336,-5.91713896897599));
#5479=CARTESIAN_POINT('Ctrl Pts',(4.7519160142661,0.362640373691391,-5.92025204980157));
#5480=CARTESIAN_POINT('Ctrl Pts',(4.76424351847546,0.314658906363046,-5.92336513062716));
#5481=CARTESIAN_POINT('Ctrl Pts',(4.77657776878623,0.266651181664317,-5.92647991505459));
#5482=CARTESIAN_POINT('Ctrl Pts',(4.7860737800577,0.217961117506413,-5.92959469948201));
#5483=CARTESIAN_POINT('Ctrl Pts',(4.79268115908479,0.168952595168909,-5.93270948390944));
#5484=CARTESIAN_POINT('Ctrl Pts',(4.79930071728701,0.119853736954804,-5.9358300097216));
#5485=CARTESIAN_POINT('Ctrl Pts',(4.80302097636537,0.0704357958584122,-5.93895053553375));
#5486=CARTESIAN_POINT('Ctrl Pts',(4.80384356571167,0.021065850090915,-5.94207106134591));
#5487=CARTESIAN_POINT('Ctrl Pts',(4.80422417664097,-0.00177755412125762,
-5.94351492423402));
#5488=CARTESIAN_POINT('Ctrl Pts',(4.80398515884719,-0.0246107176948163,
-5.94495878712213));
#5489=CARTESIAN_POINT('Ctrl Pts',(4.80313042611029,-0.0473976922820038,
-5.94640265001023));
#5490=CARTESIAN_POINT('Ctrl Pts',(4.80128205614194,-0.0966748027493485,
-5.94952502111592));
#5491=CARTESIAN_POINT('Ctrl Pts',(4.79654284474449,-0.145951235456336,-5.9526473922216));
#5492=CARTESIAN_POINT('Ctrl Pts',(4.7889147137975,-0.194860787078774,-5.95576976332729));
#5493=CARTESIAN_POINT('Ctrl Pts',(4.78130052307174,-0.243680957701523,-5.95888642837676));
#5494=CARTESIAN_POINT('Ctrl Pts',(4.77080796784645,-0.292135040197593,-5.96200309342623));
#5495=CARTESIAN_POINT('Ctrl Pts',(4.75749086411774,-0.339860134533483,-5.9651197584757));
#5496=CARTESIAN_POINT('Ctrl Pts',(4.74418717573548,-0.387537151698246,-5.96823328386791));
#5497=CARTESIAN_POINT('Ctrl Pts',(4.72806471860148,-0.434486109513725,-5.97134680926013));
#5498=CARTESIAN_POINT('Ctrl Pts',(4.70922827104811,-0.480354649383736,-5.97446033465234));
#5499=CARTESIAN_POINT('Ctrl Pts',(4.69040279690021,-0.526196467968576,-5.97757204622183));
#5500=CARTESIAN_POINT('Ctrl Pts',(4.66886667241962,-0.570958609873898,-5.98068375779132));
#5501=CARTESIAN_POINT('Ctrl Pts',(4.64477355657755,-0.614306704037186,-5.98379546936081));
#5502=CARTESIAN_POINT('Ctrl Pts',(4.62068424206337,-0.657647958889199,-5.98690668997528));
#5503=CARTESIAN_POINT('Ctrl Pts',(4.59403900408932,-0.699575131033123,-5.99001791058976));
#5504=CARTESIAN_POINT('Ctrl Pts',(4.56503719138121,-0.739778880859403,-5.99312913120424));
#5505=CARTESIAN_POINT('Ctrl Pts',(4.53600726781207,-0.780021599354146,-5.99624336746092));
#5506=CARTESIAN_POINT('Ctrl Pts',(4.50461653120828,-0.818537116168381,-5.9993576037176));
#5507=CARTESIAN_POINT('Ctrl Pts',(4.47110631650094,-0.855047025421062,-6.00247183997428));
#5508=CARTESIAN_POINT('Ctrl Pts',(4.43757789602443,-0.891576770147373,-6.00558776816481));
#5509=CARTESIAN_POINT('Ctrl Pts',(4.40192809828093,-0.926098356163972,-6.00870369635533));
#5510=CARTESIAN_POINT('Ctrl Pts',(4.36443453707344,-0.958370851958811,-6.01181962454586));
#5511=CARTESIAN_POINT('Ctrl Pts',(4.32687226299319,-0.990702492199404,-6.01494126316693));
#5512=CARTESIAN_POINT('Ctrl Pts',(4.28745991766333,-1.02077648414758,-6.018062901788));
#5513=CARTESIAN_POINT('Ctrl Pts',(4.24650618298384,-1.04839374492286,-6.02118454040908));
#5514=CARTESIAN_POINT('Ctrl Pts',(4.22768677657697,-1.06108466208688,-6.0226190221804));
#5515=CARTESIAN_POINT('Ctrl Pts',(4.20854224778094,-1.0732574273192,-6.02405350395173));
#5516=CARTESIAN_POINT('Ctrl Pts',(4.18910421403698,-1.08489601585248,-6.02548798572305));
#5517=CARTESIAN_POINT('Ctrl Pts',(4.14679330469148,-1.11022981611375,-6.02861043262194));
#5518=CARTESIAN_POINT('Ctrl Pts',(4.1029060216482,-1.13313989086988,-6.03173287952083));
#5519=CARTESIAN_POINT('Ctrl Pts',(4.05775042182792,-1.15342814934081,-6.03485532641971));
#5520=CARTESIAN_POINT('Ctrl Pts',(4.01267703349248,-1.1736794704693,-6.03797208850881));
#5521=CARTESIAN_POINT('Ctrl Pts',(3.96634040393713,-1.19131822019731,-6.04108885059791));
#5522=CARTESIAN_POINT('Ctrl Pts',(3.9190741173137,-1.20619161048218,-6.04420561268701));
#5523=CARTESIAN_POINT('Ctrl Pts',(3.87185524659392,-1.22105008029642,-6.0473192481482));
#5524=CARTESIAN_POINT('Ctrl Pts',(3.82370908510954,-1.23314851921892,-6.05043288360939));
#5525=CARTESIAN_POINT('Ctrl Pts',(3.77498816693699,-1.24238260820414,-6.05354651907058));
#5526=CARTESIAN_POINT('Ctrl Pts',(3.72629543266342,-1.25161135548725,-6.05665835336728));
#5527=CARTESIAN_POINT('Ctrl Pts',(3.67702913750895,-1.25797893382598,-6.05977018766399));
#5528=CARTESIAN_POINT('Ctrl Pts',(3.62755338927646,-1.2614318075832,-6.0628820219607));
#5529=CARTESIAN_POINT('Ctrl Pts',(3.57808525121624,-1.26488415023246,-6.06599337760684));
#5530=CARTESIAN_POINT('Ctrl Pts',(3.52840827013993,-1.26542264149081,-6.06910473325298));
#5531=CARTESIAN_POINT('Ctrl Pts',(3.47889048383974,-1.26304569470548,-6.07221608889912));
#5532=CARTESIAN_POINT('Ctrl Pts',(3.42932442986109,-1.26066643098089,-6.07533047735276));
#5533=CARTESIAN_POINT('Ctrl Pts',(3.37991842841813,-1.25536608318217,-6.0784448658064));
#5534=CARTESIAN_POINT('Ctrl Pts',(3.33103748293375,-1.24719512748296,-6.08155925426005));
#5535=CARTESIAN_POINT('Ctrl Pts',(3.28212982503215,-1.23901970652687,-6.08467534466202));
#5536=CARTESIAN_POINT('Ctrl Pts',(3.2337483288176,-1.22797067597364,-6.087791435064));
#5537=CARTESIAN_POINT('Ctrl Pts',(3.18624636692195,-1.21414935699525,-6.09090752546598));
#5538=CARTESIAN_POINT('Ctrl Pts',(3.13865715259362,-1.20030265077693,-6.0940293395572));
#5539=CARTESIAN_POINT('Ctrl Pts',(3.09195121267526,-1.18367367764803,-6.09715115364841));
#5540=CARTESIAN_POINT('Ctrl Pts',(3.04646378297013,-1.16441262155517,-6.10027296773963));
#5541=CARTESIAN_POINT('Ctrl Pts',(3.02557720540658,-1.15556847395995,-6.10170641897171));
#5542=CARTESIAN_POINT('Ctrl Pts',(3.00494721266106,-1.14617002862237,-6.1031398702038));
#5543=CARTESIAN_POINT('Ctrl Pts',(2.98460441055827,-1.13623500758593,-6.10457332143588));
#5544=CARTESIAN_POINT('Ctrl Pts',(2.94035875657203,-1.1146263078157,-6.10769108205217));
#5545=CARTESIAN_POINT('Ctrl Pts',(2.89727891392357,-1.09038131290469,-6.11080884266845));
#5546=CARTESIAN_POINT('Ctrl Pts',(2.85569836475949,-1.06364915261504,-6.11392660328474));
#5547=CARTESIAN_POINT('Ctrl Pts',(2.8141938897277,-1.03696590043122,-6.1170386597692));
#5548=CARTESIAN_POINT('Ctrl Pts',(2.77418372665897,-1.00780480194085,-6.12015071625367));
#5549=CARTESIAN_POINT('Ctrl Pts',(2.73597740755509,-0.976361141267487,-6.12326277273813));
#5550=CARTESIAN_POINT('Ctrl Pts',(2.69780957157364,-0.944949152062927,-6.12637169461938));
#5551=CARTESIAN_POINT('Ctrl Pts',(2.66144240521671,-0.911259499285034,-6.12948061650063));
#5552=CARTESIAN_POINT('Ctrl Pts',(2.6271552208983,-0.875529835342595,-6.13258953838188));
#5553=CARTESIAN_POINT('Ctrl Pts',(2.59288789143865,-0.839820861563135,-6.13569665996351));
#5554=CARTESIAN_POINT('Ctrl Pts',(2.56069853780505,-0.802074612489938,-6.13880378154514));
#5555=CARTESIAN_POINT('Ctrl Pts',(2.53083026355083,-0.76256618154647,-6.14191090312677));
#5556=CARTESIAN_POINT('Ctrl Pts',(2.50096649733004,-0.723063713630052,-6.145017555749));
#5557=CARTESIAN_POINT('Ctrl Pts',(2.47342344525313,-0.681800030670023,-6.14812420837123));
#5558=CARTESIAN_POINT('Ctrl Pts',(2.44840283402651,-0.639081882325442,-6.15123086099346));
#5559=CARTESIAN_POINT('Ctrl Pts',(2.42335738307379,-0.596321324661008,-6.15434059780894));
#5560=CARTESIAN_POINT('Ctrl Pts',(2.40083964946336,-0.552103894614342,-6.15745033462442));
#5561=CARTESIAN_POINT('Ctrl Pts',(2.38100607732538,-0.506762213631349,-6.1605600714399));
#5562=CARTESIAN_POINT('Ctrl Pts',(2.36116150573799,-0.461395386722895,-6.16367153287627));
#5563=CARTESIAN_POINT('Ctrl Pts',(2.34400424945267,-0.41490358359502,-6.16678299431264));
#5564=CARTESIAN_POINT('Ctrl Pts',(2.32964178545537,-0.367637394336423,-6.16989445574901));
#5565=CARTESIAN_POINT('Ctrl Pts',(2.31525249379191,-0.32028291649819,-6.17301172908845));
#5566=CARTESIAN_POINT('Ctrl Pts',(2.30366854040601,-0.272151700368794,-6.1761290024279));
#5567=CARTESIAN_POINT('Ctrl Pts',(2.29494654851669,-0.223605763563201,-6.17924627576734));
#5568=CARTESIAN_POINT('Ctrl Pts',(2.29083133302437,-0.200700790276553,-6.18071706956113));
#5569=CARTESIAN_POINT('Ctrl Pts',(2.28735248171025,-0.177703579422882,-6.18218786335492));
#5570=CARTESIAN_POINT('Ctrl Pts',(2.28451191880524,-0.154652350737349,-6.1836586571487));
#5571=CARTESIAN_POINT('Ctrl Pts',(2.27822806006649,-0.103658702767496,-6.18691232930561));
#5572=CARTESIAN_POINT('Ctrl Pts',(2.27505166281584,-0.0522775696465564,
-6.19016600146251));
#5573=CARTESIAN_POINT('Ctrl Pts',(2.27501930025721,-0.000794877769987878,
-6.19341967361942));
#5574=CARTESIAN_POINT('Ctrl Pts',(2.27501930025681,-0.000794877133460714,
-6.19341967365965));
#5575=CARTESIAN_POINT('Ctrl Pts',(2.27498866481498,0.0479403385423533,-6.19649970713347));
#5576=CARTESIAN_POINT('Ctrl Pts',(2.27777974167085,0.0967837354840311,-6.19957974060728));
#5577=CARTESIAN_POINT('Ctrl Pts',(2.28340368707692,0.145376903137893,-6.2026597740811));
#5578=CARTESIAN_POINT('Ctrl Pts',(2.28902068514398,0.193910042967064,-6.20573600274617));
#5579=CARTESIAN_POINT('Ctrl Pts',(2.29746356813488,0.242193009571163,-6.20881223141124));
#5580=CARTESIAN_POINT('Ctrl Pts',(2.30869149746577,0.28986856483816,-6.21188846007631));
#5581=CARTESIAN_POINT('Ctrl Pts',(2.31991062224023,0.337506734572732,-6.21496227646855));
#5582=CARTESIAN_POINT('Ctrl Pts',(2.33391034355925,0.384537889114209,-6.21803609286079));
#5583=CARTESIAN_POINT('Ctrl Pts',(2.35059855415923,0.430613868290296,-6.22110990925304));
#5584=CARTESIAN_POINT('Ctrl Pts',(2.36728120520785,0.476674497601834,-6.22418270162656));
#5585=CARTESIAN_POINT('Ctrl Pts',(2.38665037854992,0.521780053466338,-6.22725549400008));
#5586=CARTESIAN_POINT('Ctrl Pts',(2.4085646527477,0.565599151678052,-6.2303282863736));
#5587=CARTESIAN_POINT('Ctrl Pts',(2.43049637673816,0.60945314195016,-6.23340352553543));
#5588=CARTESIAN_POINT('Ctrl Pts',(2.45497699765719,0.652018123811447,-6.23647876469726));
#5589=CARTESIAN_POINT('Ctrl Pts',(2.48181851722148,0.692986170183253,-6.23955400385908));
#5590=CARTESIAN_POINT('Ctrl Pts',(2.50867171307318,0.733972038000772,-6.24263058077588));
#5591=CARTESIAN_POINT('Ctrl Pts',(2.53788751699157,0.773359134237717,-6.24570715769268));
#5592=CARTESIAN_POINT('Ctrl Pts',(2.56923596999665,0.810870516074163,-6.24878373460948));
#5593=CARTESIAN_POINT('Ctrl Pts',(2.60064014758636,0.84844857763388,-6.25186578040766));
#5594=CARTESIAN_POINT('Ctrl Pts',(2.63418415230918,0.884143862022931,-6.25494782620583));
#5595=CARTESIAN_POINT('Ctrl Pts',(2.66960061631979,0.91771573376914,-6.25802987200401));
#5596=CARTESIAN_POINT('Ctrl Pts',(2.68765761510404,0.934832271634837,-6.25960124562318));
#5597=CARTESIAN_POINT('Ctrl Pts',(2.70620080772796,0.951397482579278,-6.26117261924236));
#5598=CARTESIAN_POINT('Ctrl Pts',(2.72519170678115,0.967383702259465,-6.26274399286153));
#5599=CARTESIAN_POINT('Ctrl Pts',(2.76296112936729,0.999177367475883,-6.26586916740419));
#5600=CARTESIAN_POINT('Ctrl Pts',(2.80267577049992,1.02882352473978,-6.26899434194685));
#5601=CARTESIAN_POINT('Ctrl Pts',(2.84406211499685,1.05607760177351,-6.27211951648951));
#5602=CARTESIAN_POINT('Ctrl Pts',(2.88537441929957,1.08328292124767,-6.27523910009311));
#5603=CARTESIAN_POINT('Ctrl Pts',(2.92835204198969,1.10810435070506,-6.27835868369671));
#5604=CARTESIAN_POINT('Ctrl Pts',(2.97268912824492,1.13033804205804,-6.28147826730031));
#5605=CARTESIAN_POINT('Ctrl Pts',(3.01698256327074,1.15254984365588,-6.2845947795776));
#5606=CARTESIAN_POINT('Ctrl Pts',(3.0626323255472,1.17217870774427,-6.28771129185488));
#5607=CARTESIAN_POINT('Ctrl Pts',(3.10930621329362,1.18906566882115,-6.29082780413217));
#5608=CARTESIAN_POINT('Ctrl Pts',(3.15595385882097,1.20594313526725,-6.29394256416207));
#5609=CARTESIAN_POINT('Ctrl Pts',(3.20362397598171,1.22008156773149,-6.29705732419197));
#5610=CARTESIAN_POINT('Ctrl Pts',(3.25196492088847,1.23137032309035,-6.30017208422187));
#5611=CARTESIAN_POINT('Ctrl Pts',(3.30029909838449,1.24265749809857,-6.30328640820609));
#5612=CARTESIAN_POINT('Ctrl Pts',(3.34930338505032,1.25109566524075,-6.3064007321903));
#5613=CARTESIAN_POINT('Ctrl Pts',(3.39861404298749,1.25662485606469,-6.30951505617452));
#5614=CARTESIAN_POINT('Ctrl Pts',(3.44797333837544,1.26215950059292,-6.31263245196483));
#5615=CARTESIAN_POINT('Ctrl Pts',(3.49763906418198,1.26477938096814,-6.31574984775513));
#5616=CARTESIAN_POINT('Ctrl Pts',(3.54724222921144,1.2644764143745,-6.31886724354544));
#5617=CARTESIAN_POINT('Ctrl Pts',(3.59687289428225,1.2641732798159,-6.32198636762291));
#5618=CARTESIAN_POINT('Ctrl Pts',(3.64644038379152,1.26094410710264,-6.32510549170037));
#5619=CARTESIAN_POINT('Ctrl Pts',(3.69557912019877,1.25483285923727,-6.32822461577784));
#5620=CARTESIAN_POINT('Ctrl Pts',(3.7448080925388,1.24871038898012,-6.3313494676597));
#5621=CARTESIAN_POINT('Ctrl Pts',(3.793606203084,1.23969538077051,-6.33447431954156));
#5622=CARTESIAN_POINT('Ctrl Pts',(3.84161801442852,1.22788292029281,-6.33759917142343));
#5623=CARTESIAN_POINT('Ctrl Pts',(3.86328277537995,1.22255268747444,-6.33900922380707));
#5624=CARTESIAN_POINT('Ctrl Pts',(3.88478764633446,1.21665352349932,-6.34041927619071));
#5625=CARTESIAN_POINT('Ctrl Pts',(3.90610121351515,1.21019740856716,-6.34182932857435));
#5626=CARTESIAN_POINT('Ctrl Pts',(3.93106378827338,1.20263596893224,-6.34348079018757));
#5627=CARTESIAN_POINT('Ctrl Pts',(3.95582479527397,1.19429200464362,-6.34513225180078));
#5628=CARTESIAN_POINT('Ctrl Pts',(3.98033068509731,1.1851773507521,-6.346783713414));
#5629=CARTESIAN_POINT('Origin',(3.53951905042299,8.32667268468867E-16,-7.60421172358873));
#5630=CARTESIAN_POINT('',(1.99651962906757,0.00133629967821312,-5.85421172358873));
#5631=CARTESIAN_POINT('Ctrl Pts',(4.4805026613161,-1.22496740309806,-6.17703688246106));
#5632=CARTESIAN_POINT('Ctrl Pts',(4.8351830152191,-0.947966885397602,-6.15375615496722));
#5633=CARTESIAN_POINT('Ctrl Pts',(5.3296905430907,-0.00766043899371661,
-6.10411364890244));
#5634=CARTESIAN_POINT('Ctrl Pts',(4.58962568481027,1.48829617865197,-6.02810936426672));
#5635=CARTESIAN_POINT('Ctrl Pts',(2.86500634349213,1.69194423152176,-5.94902402855389));
#5636=CARTESIAN_POINT('Ctrl Pts',(2.05033956475987,0.713964383672213,-5.8910581483279));
#5637=CARTESIAN_POINT('Ctrl Pts',(1.99506637965176,0.10286799783797,-5.85945404667284));
#5638=CARTESIAN_POINT('Ctrl Pts',(1.99598824456801,0.00133675987860297,
-5.85421172358873));
#5639=CARTESIAN_POINT('Ctrl Pts',(1.99651962906757,0.00133629967821312,
-5.85421172358873));
#5640=CARTESIAN_POINT('Ctrl Pts',(1.99647063856088,-0.0552320919015559,
-5.85128991870194));
#5641=CARTESIAN_POINT('Ctrl Pts',(1.99953669991828,-0.111900437912663,-5.84836811381516));
#5642=CARTESIAN_POINT('Ctrl Pts',(2.00572420093829,-0.168292482583732,-5.84544630892837));
#5643=CARTESIAN_POINT('Ctrl Pts',(2.01190613034431,-0.22463374832097,-5.84252713501796));
#5644=CARTESIAN_POINT('Ctrl Pts',(2.02120387741375,-0.280698672975614,-5.83960796110754));
#5645=CARTESIAN_POINT('Ctrl Pts',(2.03357181527654,-0.336112964574063,-5.83668878719712));
#5646=CARTESIAN_POINT('Ctrl Pts',(2.04593370493793,-0.39150015733038,-5.83377104082879));
#5647=CARTESIAN_POINT('Ctrl Pts',(2.06136269399849,-0.446236823221072,-5.83085329446045));
#5648=CARTESIAN_POINT('Ctrl Pts',(2.07976194100033,-0.499958179741059,-5.82793554809211));
#5649=CARTESIAN_POINT('Ctrl Pts',(2.09815975929864,-0.55367536479188,-5.82501802828709));
#5650=CARTESIAN_POINT('Ctrl Pts',(2.11952720091026,-0.606376889209763,-5.82210050848208));
#5651=CARTESIAN_POINT('Ctrl Pts',(2.14371812919713,-0.657714822932431,-5.81918298867706));
#5652=CARTESIAN_POINT('Ctrl Pts',(2.1679326246043,-0.709102770744913,-5.81626262658591));
#5653=CARTESIAN_POINT('Ctrl Pts',(2.19497586222247,-0.759123991599414,-5.81334226449475));
#5654=CARTESIAN_POINT('Ctrl Pts',(2.22465502102199,-0.807453765975103,-5.81042190240359));
#5655=CARTESIAN_POINT('Ctrl Pts',(2.25435184685727,-0.855812309490017,-5.80749980191608));
#5656=CARTESIAN_POINT('Ctrl Pts',(2.28668740535122,-0.902476964311451,-5.80457770142857));
#5657=CARTESIAN_POINT('Ctrl Pts',(2.3214265789633,-0.947153488603201,-5.80165560094106));
#5658=CARTESIAN_POINT('Ctrl Pts',(2.35622433730217,-0.991905356137118,-5.79872857257412));
#5659=CARTESIAN_POINT('Ctrl Pts',(2.39343343625151,-1.03466200763537,-5.79580154420719));
#5660=CARTESIAN_POINT('Ctrl Pts',(2.43278086258591,-1.07516490994781,-5.79287451584026));
#5661=CARTESIAN_POINT('Ctrl Pts',(2.44183753298804,-1.08448753840783,-5.79220079626958));
#5662=CARTESIAN_POINT('Ctrl Pts',(2.45100735116571,-1.09369093355053,-5.79152707669891));
#5663=CARTESIAN_POINT('Ctrl Pts',(2.46028674854408,-1.10277225145592,-5.79085335712824));
#5664=CARTESIAN_POINT('Ctrl Pts',(2.50119736372677,-1.14280958222535,-5.78788309074425));
#5665=CARTESIAN_POINT('Ctrl Pts',(2.54442403981831,-1.18065055045223,-5.78491282436025));
#5666=CARTESIAN_POINT('Ctrl Pts',(2.5897016260704,-1.21601638985509,-5.78194255797625));
#5667=CARTESIAN_POINT('Ctrl Pts',(2.63489924292426,-1.25131976601445,-5.77897753768497));
#5668=CARTESIAN_POINT('Ctrl Pts',(2.68214017261957,-1.28415637209005,-5.77601251739368));
#5669=CARTESIAN_POINT('Ctrl Pts',(2.73112360642299,-1.3142852833841,-5.7730474971024));
#5670=CARTESIAN_POINT('Ctrl Pts',(2.78005870122236,-1.3443844621451,-5.77008540282337));
#5671=CARTESIAN_POINT('Ctrl Pts',(2.83073245125779,-1.37178096864678,-5.76712330854435));
#5672=CARTESIAN_POINT('Ctrl Pts',(2.88281369051602,-1.39627614398781,-5.76416121426532));
#5673=CARTESIAN_POINT('Ctrl Pts',(2.93486358072305,-1.42075657504631,-5.76120090294781));
#5674=CARTESIAN_POINT('Ctrl Pts',(2.98831880993198,-1.4423389154832,-5.7582405916303));
#5675=CARTESIAN_POINT('Ctrl Pts',(3.04282409600851,-1.46087067266723,-5.75528028031279));
#5676=CARTESIAN_POINT('Ctrl Pts',(3.09731755283789,-1.47939840791592,-5.75232061146974));
#5677=CARTESIAN_POINT('Ctrl Pts',(3.15286012075714,-1.49487670675489,-5.74936094262669));
#5678=CARTESIAN_POINT('Ctrl Pts',(3.20907914364962,-1.50720219878144,-5.74640127378364));
#5679=CARTESIAN_POINT('Ctrl Pts',(3.26534886690617,-1.51953880638597,-5.74343893580334));
#5680=CARTESIAN_POINT('Ctrl Pts',(3.32229575398386,-1.52871681276762,-5.74047659782305));
#5681=CARTESIAN_POINT('Ctrl Pts',(3.37953602790866,-1.53468382167376,-5.73751425984275));
#5682=CARTESIAN_POINT('Ctrl Pts',(3.43680046940972,-1.54065334992743,-5.73455067112545));
#5683=CARTESIAN_POINT('Ctrl Pts',(3.49435802300424,-1.54340915196995,-5.73158708240814));
#5684=CARTESIAN_POINT('Ctrl Pts',(3.55182208858797,-1.54295095037137,-5.72862349369083));
#5685=CARTESIAN_POINT('Ctrl Pts',(3.60939633838999,-1.54249187019616,-5.72565422245346));
#5686=CARTESIAN_POINT('Ctrl Pts',(3.6668762199932,-1.53880650470921,-5.72268495121608));
#5687=CARTESIAN_POINT('Ctrl Pts',(3.72387841604006,-1.53194667802416,-5.7197156799787));
#5688=CARTESIAN_POINT('Ctrl Pts',(3.77473646114266,-1.52582625812565,-5.71706646045761));
#5689=CARTESIAN_POINT('Ctrl Pts',(3.82521408602547,-1.51717961894724,-5.71441724093651));
#5690=CARTESIAN_POINT('Ctrl Pts',(3.87504773869695,-1.50607752102777,-5.71176802141542));
#5691=CARTESIAN_POINT('Ctrl Pts',(3.93090212592116,-1.49363410492333,-5.70879873208902));
#5692=CARTESIAN_POINT('Ctrl Pts',(3.98617942899864,-1.47805350283576,-5.70582944276262));
#5693=CARTESIAN_POINT('Ctrl Pts',(4.04050175195703,-1.45940581496842,-5.70286015343622));
#5694=CARTESIAN_POINT('Ctrl Pts',(4.09474970761238,-1.44078365580052,-5.69989492906925));
#5695=CARTESIAN_POINT('Ctrl Pts',(4.14804478403148,-1.41910289486014,-5.69692970470228));
#5696=CARTESIAN_POINT('Ctrl Pts',(4.20002090048548,-1.39448424374893,-5.69396448033531));
#5697=CARTESIAN_POINT('Ctrl Pts',(4.2519448213428,-1.36989031524633,-5.691002233714));
#5698=CARTESIAN_POINT('Ctrl Pts',(4.30255193818079,-1.34236456518616,-5.68803998709269));
#5699=CARTESIAN_POINT('Ctrl Pts',(4.35149505667516,-1.31207620406391,-5.68507774047138));
#5700=CARTESIAN_POINT('Ctrl Pts',(4.39558502363139,-1.28479120706905,-5.68240922731432));
#5701=CARTESIAN_POINT('Ctrl Pts',(4.43832462406854,-1.25526506293894,-5.67974071415726));
#5702=CARTESIAN_POINT('Ctrl Pts',(4.47947725029973,-1.22365337513712,-5.6770722010002));
#5703=CARTESIAN_POINT('',(1.99651939415668,-0.0010299330301491,-5.89578827637539));
#5704=CARTESIAN_POINT('Ctrl Pts',(1.99651939415668,-0.00102993303015119,
-5.89578827637539));
#5705=CARTESIAN_POINT('Ctrl Pts',(1.99656311124628,-0.0665249237226865,
-5.89242280315063));
#5706=CARTESIAN_POINT('Ctrl Pts',(2.00078094053252,-0.131858231058162,-5.88905732992587));
#5707=CARTESIAN_POINT('Ctrl Pts',(2.00908724191393,-0.196538748097368,-5.88569185670111));
#5708=CARTESIAN_POINT('Ctrl Pts',(2.01746504072735,-0.261776010029041,-5.88229741478355));
#5709=CARTESIAN_POINT('Ctrl Pts',(2.03000187710493,-0.326348970253648,-5.87890297286599));
#5710=CARTESIAN_POINT('Ctrl Pts',(2.04656016328037,-0.389772704665002,-5.87550853094842));
#5711=CARTESIAN_POINT('Ctrl Pts',(2.0598792412247,-0.440789195936822,-5.87277812539808));
#5712=CARTESIAN_POINT('Ctrl Pts',(2.07579929237439,-0.491062442571037,-5.87004771984774));
#5713=CARTESIAN_POINT('Ctrl Pts',(2.09422649337875,-0.54035027949703,-5.8673173142974));
#5714=CARTESIAN_POINT('Ctrl Pts',(2.11427285398687,-0.593968935546792,-5.86434699372318));
#5715=CARTESIAN_POINT('Ctrl Pts',(2.13734871336475,-0.646582004481705,-5.86137667314896));
#5716=CARTESIAN_POINT('Ctrl Pts',(2.16333231133361,-0.697824518883177,-5.85840635257474));
#5717=CARTESIAN_POINT('Ctrl Pts',(2.18927003388335,-0.74897656191007,-5.8554412762589));
#5718=CARTESIAN_POINT('Ctrl Pts',(2.21810507132652,-0.798762392239985,-5.85247619994305));
#5719=CARTESIAN_POINT('Ctrl Pts',(2.24966731486717,-0.846836170864018,-5.84951112362721));
#5720=CARTESIAN_POINT('Ctrl Pts',(2.28119842340232,-0.894862526453641,-5.84654897225133));
#5721=CARTESIAN_POINT('Ctrl Pts',(2.31545112299997,-0.941179742998912,-5.84358682087544));
#5722=CARTESIAN_POINT('Ctrl Pts',(2.35220987785363,-0.985467365635541,-5.84062466949955));
#5723=CARTESIAN_POINT('Ctrl Pts',(2.38894651900094,-1.02972834527281,-5.83766430012488));
#5724=CARTESIAN_POINT('Ctrl Pts',(2.42818589452722,-1.07196175113325,-5.83470393075021));
#5725=CARTESIAN_POINT('Ctrl Pts',(2.46967103689842,-1.11187869300456,-5.83174356137554));
#5726=CARTESIAN_POINT('Ctrl Pts',(2.51114718785878,-1.15178698335383,-5.82878383362569));
#5727=CARTESIAN_POINT('Ctrl Pts',(2.55486776378531,-1.18937944535614,-5.82582410587584));
#5728=CARTESIAN_POINT('Ctrl Pts',(2.60053921513923,-1.2244042914538,-5.82286437812599));
#5729=CARTESIAN_POINT('Ctrl Pts',(2.64625186667548,-1.25946073343909,-5.81990198040794));
#5730=CARTESIAN_POINT('Ctrl Pts',(2.69391849626159,-1.29194461244608,-5.81693958268989));
#5731=CARTESIAN_POINT('Ctrl Pts',(2.74321384782584,-1.32164557439455,-5.81397718497184));
#5732=CARTESIAN_POINT('Ctrl Pts',(2.79253002127664,-1.35135908174621,-5.81101353596523));
#5733=CARTESIAN_POINT('Ctrl Pts',(2.84347582688872,-1.3782870836566,-5.80804988695863));
#5734=CARTESIAN_POINT('Ctrl Pts',(2.89570132904561,-1.40226521800993,-5.80508623795202));
#5735=CARTESIAN_POINT('Ctrl Pts',(2.94802697090794,-1.42628932919856,-5.80211690630138));
#5736=CARTESIAN_POINT('Ctrl Pts',(3.00163672595878,-1.44735207851464,-5.79914757465073));
#5737=CARTESIAN_POINT('Ctrl Pts',(3.0561615146613,-1.46533767187716,-5.79617824300008));
#5738=CARTESIAN_POINT('Ctrl Pts',(3.10479966393815,-1.48138149333188,-5.79352948819492));
#5739=CARTESIAN_POINT('Ctrl Pts',(3.15416545298975,-1.49497737112332,-5.79088073338975));
#5740=CARTESIAN_POINT('Ctrl Pts',(3.20399036525539,-1.50607752171981,-5.78823197858458));
#5741=CARTESIAN_POINT('Ctrl Pts',(3.25984361339259,-1.51852068393395,-5.78526274988631));
#5742=CARTESIAN_POINT('Ctrl Pts',(3.31650607033671,-1.5278785066749,-5.78229352118805));
#5743=CARTESIAN_POINT('Ctrl Pts',(3.37360583569431,-1.53405404245691,-5.77932429248978));
#5744=CARTESIAN_POINT('Ctrl Pts',(3.43062525672136,-1.54022088872356,-5.77635924175426));
#5745=CARTESIAN_POINT('Ctrl Pts',(3.48808025361493,-1.54321426355827,-5.77339419101873));
#5746=CARTESIAN_POINT('Ctrl Pts',(3.545588182638,-1.54298806399601,-5.7704291402832));
#5747=CARTESIAN_POINT('Ctrl Pts',(3.60303733296054,-1.54276209563171,-5.76746712011811));
#5748=CARTESIAN_POINT('Ctrl Pts',(3.66053878950446,-1.53932307715738,-5.76450509995301));
#5749=CARTESIAN_POINT('Ctrl Pts',(3.71770644176347,-1.53267682619895,-5.76154307978792));
#5750=CARTESIAN_POINT('Ctrl Pts',(3.77483766885917,-1.52603480999158,-5.7585829469151));
#5751=CARTESIAN_POINT('Ctrl Pts',(3.83163499688114,-1.51618967455776,-5.75562281404227));
#5752=CARTESIAN_POINT('Ctrl Pts',(3.88771620729142,-1.50319916842338,-5.75266268116945));
#5753=CARTESIAN_POINT('Ctrl Pts',(3.94381019864848,-1.49020570174363,-5.74970187368028));
#5754=CARTESIAN_POINT('Ctrl Pts',(3.99918723471621,-1.47406553478078,-5.74674106619112));
#5755=CARTESIAN_POINT('Ctrl Pts',(4.05347574099386,-1.4548874596399,-5.74378025870196));
#5756=CARTESIAN_POINT('Ctrl Pts',(4.10776768221337,-1.43570817106403,-5.74081926387662));
#5757=CARTESIAN_POINT('Ctrl Pts',(4.16097046861186,-1.41349077698758,-5.73785826905127));
#5758=CARTESIAN_POINT('Ctrl Pts',(4.21273086404559,-1.38839290332347,-5.73489727422593));
#5759=CARTESIAN_POINT('Ctrl Pts',(4.26455729142666,-1.36326301171478,-5.73193250199022));
#5760=CARTESIAN_POINT('Ctrl Pts',(4.31493718855317,-1.33524554149718,-5.7289677297545));
#5761=CARTESIAN_POINT('Ctrl Pts',(4.36354152761078,-1.30454434845631,-5.72600295751879));
#5762=CARTESIAN_POINT('Ctrl Pts',(4.40343807886671,-1.27934347656869,-5.72356934377653));
#5763=CARTESIAN_POINT('Ctrl Pts',(4.44213866194226,-1.252335282131,-5.72113573003426));
#5764=CARTESIAN_POINT('Ctrl Pts',(4.47947725029973,-1.22365337513712,-5.718702116292));
#5765=CARTESIAN_POINT('Ctrl Pts',(4.47947725029973,-1.22365337513712,-6.21868039134515));
#5766=CARTESIAN_POINT('Ctrl Pts',(4.52523315907666,-1.1885056425181,-6.21571279242732));
#5767=CARTESIAN_POINT('Ctrl Pts',(4.56900329419267,-1.15079704745477,-6.21274519350949));
#5768=CARTESIAN_POINT('Ctrl Pts',(4.61049943673485,-1.11078801404016,-6.20977759459167));
#5769=CARTESIAN_POINT('Ctrl Pts',(4.65201300551891,-1.0707621788929,-6.20680874943519));
#5770=CARTESIAN_POINT('Ctrl Pts',(4.6912503230112,-1.02843436000381,-6.20383990427871));
#5771=CARTESIAN_POINT('Ctrl Pts',(4.72796119069533,-0.984100746481225,-6.20087105912224));
#5772=CARTESIAN_POINT('Ctrl Pts',(4.76474313047905,-0.939681303252234,-6.19789646629288));
#5773=CARTESIAN_POINT('Ctrl Pts',(4.79898853545788,-0.89324872378389,-6.19492187346353));
#5774=CARTESIAN_POINT('Ctrl Pts',(4.83048911952562,-0.845130333546938,-6.19194728063417));
#5775=CARTESIAN_POINT('Ctrl Pts',(4.85974763162996,-0.800436797066403,-6.18918440613901));
#5776=CARTESIAN_POINT('Ctrl Pts',(4.88663845078139,-0.754289480962414,-6.18642153164386));
#5777=CARTESIAN_POINT('Ctrl Pts',(4.91103098090795,-0.706968192026646,-6.18365865714871));
#5778=CARTESIAN_POINT('Ctrl Pts',(4.93722198129047,-0.656157886978836,-6.18069207489651));
#5779=CARTESIAN_POINT('Ctrl Pts',(4.96064138038873,-0.603781949096697,-6.17772549264432));
#5780=CARTESIAN_POINT('Ctrl Pts',(4.98110043515803,-0.550174618812436,-6.17475891039213));
#5781=CARTESIAN_POINT('Ctrl Pts',(5.00152279065203,-0.496663448893067,-6.1717976495695));
#5782=CARTESIAN_POINT('Ctrl Pts',(5.01899515628914,-0.441925754840174,-6.16883638874687));
#5783=CARTESIAN_POINT('Ctrl Pts',(5.03337538817453,-0.386318834849605,-6.16587512792423));
#5784=CARTESIAN_POINT('Ctrl Pts',(5.04774120080218,-0.330767672688111,-6.16291683639885));
#5785=CARTESIAN_POINT('Ctrl Pts',(5.05902089194744,-0.27434951481704,-6.15995854487347));
#5786=CARTESIAN_POINT('Ctrl Pts',(5.06712160528695,-0.217438346142331,-6.15700025334809));
#5787=CARTESIAN_POINT('Ctrl Pts',(5.07521733588585,-0.160562183470108,-6.15404378146485));
#5788=CARTESIAN_POINT('Ctrl Pts',(5.08013789098226,-0.103194127555836,-6.15108730958161));
#5789=CARTESIAN_POINT('Ctrl Pts',(5.08184161392253,-0.045717722167791,-6.14813083769836));
#5790=CARTESIAN_POINT('Ctrl Pts',(5.08354494926005,0.0117456071428263,-6.14517503842251));
#5791=CARTESIAN_POINT('Ctrl Pts',(5.08203288981773,0.0693167147109322,-6.14221923914666));
#5792=CARTESIAN_POINT('Ctrl Pts',(5.07731583509648,0.126609829981231,-6.13926343987081));
#5793=CARTESIAN_POINT('Ctrl Pts',(5.07259454704983,0.183954363014137,-6.13630498790999));
#5794=CARTESIAN_POINT('Ctrl Pts',(5.0646625579511,0.241019882873989,-6.13334653594918));
#5795=CARTESIAN_POINT('Ctrl Pts',(5.05358226242277,0.297424931821321,-6.13038808398836));
#5796=CARTESIAN_POINT('Ctrl Pts',(5.0424973401078,0.353853533761988,-6.12742839667006));
#5797=CARTESIAN_POINT('Ctrl Pts',(5.02826161926058,0.40962060716878,-6.12446870935177));
#5798=CARTESIAN_POINT('Ctrl Pts',(5.01098814647375,0.464357297097349,-6.12150902203347));
#5799=CARTESIAN_POINT('Ctrl Pts',(4.99368136679308,0.519199530893311,-6.11854362781462));
#5800=CARTESIAN_POINT('Ctrl Pts',(4.9733253157744,0.57300692032904,-6.11557823359577));
#5801=CARTESIAN_POINT('Ctrl Pts',(4.95008188101104,0.625429053501209,-6.11261283937692));
#5802=CARTESIAN_POINT('Ctrl Pts',(4.9290766905821,0.672803157250667,-6.10993300006324));
#5803=CARTESIAN_POINT('Ctrl Pts',(4.9057141893479,0.719045982025723,-6.10725316074956));
#5804=CARTESIAN_POINT('Ctrl Pts',(4.88014509712215,0.763918060338797,-6.10457332143588));
#5805=CARTESIAN_POINT('Ctrl Pts',(4.85179886425067,0.813663838173202,-6.10160241622841));
#5806=CARTESIAN_POINT('Ctrl Pts',(4.82062127632723,0.861932893587305,-6.09863151102094));
#5807=CARTESIAN_POINT('Ctrl Pts',(4.78679087939057,0.908384271475387,-6.09566060581347));
#5808=CARTESIAN_POINT('Ctrl Pts',(4.75302018267901,0.954753676996385,-6.09269494333815));
#5809=CARTESIAN_POINT('Ctrl Pts',(4.71660627330049,0.999311354084992,-6.08972928086283));
#5810=CARTESIAN_POINT('Ctrl Pts',(4.67777236989149,1.04174295328499,-6.08676361838751));
#5811=CARTESIAN_POINT('Ctrl Pts',(4.6389767606605,1.08413271061307,-6.08380088035699));
#5812=CARTESIAN_POINT('Ctrl Pts',(4.59776623569061,1.12440016161227,-6.08083814232647));
#5813=CARTESIAN_POINT('Ctrl Pts',(4.5544048047997,1.16226326861138,-6.07787540429594));
#5814=CARTESIAN_POINT('Ctrl Pts',(4.51106946267869,1.20010359495345,-6.0749144488217));
#5815=CARTESIAN_POINT('Ctrl Pts',(4.46558617173701,1.23554210300131,-6.07195349334745));
#5816=CARTESIAN_POINT('Ctrl Pts',(4.41825480438215,1.26833452791991,-6.0689925378732));
#5817=CARTESIAN_POINT('Ctrl Pts',(4.37093371915363,1.30111982910906,-6.06603222562816));
#5818=CARTESIAN_POINT('Ctrl Pts',(4.32176578271883,1.3312598919607,-6.06307191338313));
#5819=CARTESIAN_POINT('Ctrl Pts',(4.2710810612163,1.35855291555539,-6.06011160113809));
#5820=CARTESIAN_POINT('Ctrl Pts',(4.22035075106559,1.38587048800846,-6.05714862622413));
#5821=CARTESIAN_POINT('Ctrl Pts',(4.1681013890533,1.41033565572674,-6.05418565131016));
#5822=CARTESIAN_POINT('Ctrl Pts',(4.11468773232934,1.43179257832764,-6.05122267639619));
#5823=CARTESIAN_POINT('Ctrl Pts',(4.06125157419493,1.45325854002176,-6.04825845327869));
#5824=CARTESIAN_POINT('Ctrl Pts',(4.0066506377794,1.47171356196304,-6.04529423016119));
#5825=CARTESIAN_POINT('Ctrl Pts',(3.95125671194513,1.48705114171782,-6.0423300070437));
#5826=CARTESIAN_POINT('Ctrl Pts',(3.8957568288956,1.50241805911595,-6.03936011397553));
#5827=CARTESIAN_POINT('Ctrl Pts',(3.83946143611798,1.51465550703195,-6.03639022090737));
#5828=CARTESIAN_POINT('Ctrl Pts',(3.78275347878595,1.52370798149086,-6.0334203278392));
#5829=CARTESIAN_POINT('Ctrl Pts',(3.7322660360912,1.53176745509902,-6.03077621380048));
#5830=CARTESIAN_POINT('Ctrl Pts',(3.68145194585289,1.53730309517344,-6.02813209976177));
#5831=CARTESIAN_POINT('Ctrl Pts',(3.63058241961525,1.54031050856357,-6.02548798572305));
#5832=CARTESIAN_POINT('Ctrl Pts',(3.5734292076912,1.54368941431603,-6.02251725607048));
#5833=CARTESIAN_POINT('Ctrl Pts',(3.51596930837668,1.54389000739262,-6.01954652641792));
#5834=CARTESIAN_POINT('Ctrl Pts',(3.45858585276228,1.54087599031084,-6.01657579676535));
#5835=CARTESIAN_POINT('Ctrl Pts',(3.40130335532185,1.53786727597108,-6.01361029369661));
#5836=CARTESIAN_POINT('Ctrl Pts',(3.34409755080177,1.53165520442107,-6.01064479062787));
#5837=CARTESIAN_POINT('Ctrl Pts',(3.28735363447812,1.52225543290256,-6.00767928755913));
#5838=CARTESIAN_POINT('Ctrl Pts',(3.2306654857854,1.51286489943145,-6.00471669897165));
#5839=CARTESIAN_POINT('Ctrl Pts',(3.17443883741385,1.50029295806146,-6.00175411038417));
#5840=CARTESIAN_POINT('Ctrl Pts',(3.11905404576029,1.48460707928192,-5.99879152179669));
#5841=CARTESIAN_POINT('Ctrl Pts',(3.06370238715066,1.4689305843223,-5.99583070552928));
#5842=CARTESIAN_POINT('Ctrl Pts',(3.00919208724658,1.45014398657061,-5.99286988926187));
#5843=CARTESIAN_POINT('Ctrl Pts',(2.95589139740111,1.42836541635121,-5.98990907299446));
#5844=CARTESIAN_POINT('Ctrl Pts',(2.90260209758853,1.40659150007967,-5.98694888943546));
#5845=CARTESIAN_POINT('Ctrl Pts',(2.85052237671371,1.38182707787297,-5.98398870587646));
#5846=CARTESIAN_POINT('Ctrl Pts',(2.80000135672649,1.35423874583096,-5.98102852231746));
#5847=CARTESIAN_POINT('Ctrl Pts',(2.7494345918152,1.32662543356973,-5.9780656584212));
#5848=CARTESIAN_POINT('Ctrl Pts',(2.70042980679601,1.29618335169555,-5.97510279452494));
#5849=CARTESIAN_POINT('Ctrl Pts',(2.65331106399839,1.26312485716862,-5.97213993062869));
#5850=CARTESIAN_POINT('Ctrl Pts',(2.60617231945885,1.23005232942611,-5.96917580900704));
#5851=CARTESIAN_POINT('Ctrl Pts',(2.56092162380492,1.19436149745353,-5.9662116873854));
#5852=CARTESIAN_POINT('Ctrl Pts',(2.51785096846392,1.15630589824063,-5.96324756576375));
#5853=CARTESIAN_POINT('Ctrl Pts',(2.47469767089845,1.11817727948931,-5.96027775670591));
#5854=CARTESIAN_POINT('Ctrl Pts',(2.43373314442815,1.07767519380697,-5.95730794764806));
#5855=CARTESIAN_POINT('Ctrl Pts',(2.39521271537853,1.03509033981442,-5.95433813859021));
#5856=CARTESIAN_POINT('Ctrl Pts',(2.36090316675489,0.997160670941657,-5.95169297573022));
#5857=CARTESIAN_POINT('Ctrl Pts',(2.32853216646961,0.957579404572623,-5.94904781287022));
#5858=CARTESIAN_POINT('Ctrl Pts',(2.2982514595631,0.91657174726307,-5.94640265001023));
#5859=CARTESIAN_POINT('Ctrl Pts',(2.26409693031632,0.870317964772287,-5.94341909046048));
#5860=CARTESIAN_POINT('Ctrl Pts',(2.23245953901597,0.822055478003167,-5.94043553091072));
#5861=CARTESIAN_POINT('Ctrl Pts',(2.2035811354599,0.77208735733987,-5.93745197136097));
#5862=CARTESIAN_POINT('Ctrl Pts',(2.17474883426353,0.722199007300613,-5.93447317485622));
#5863=CARTESIAN_POINT('Ctrl Pts',(2.14866704348227,0.670610863712113,-5.93149437835146));
#5864=CARTESIAN_POINT('Ctrl Pts',(2.12553550006044,0.617656473538582,-5.9285155818467));
#5865=CARTESIAN_POINT('Ctrl Pts',(2.10243419074161,0.564771297444616,-5.92554067878039));
#5866=CARTESIAN_POINT('Ctrl Pts',(2.08227568039562,0.510523888301181,-5.92256577571407));
#5867=CARTESIAN_POINT('Ctrl Pts',(2.06521366265845,0.455272032534889,-5.91959087264776));
#5868=CARTESIAN_POINT('Ctrl Pts',(2.04816489876985,0.400063096647172,-5.91661828049891));
#5869=CARTESIAN_POINT('Ctrl Pts',(2.03420800733172,0.34385175250833,-5.91364568835005));
#5870=CARTESIAN_POINT('Ctrl Pts',(2.02344773952354,0.287013554153131,-5.9106730962012));
#5871=CARTESIAN_POINT('Ctrl Pts',(2.01268935513701,0.230185304462381,-5.90770102435952));
#5872=CARTESIAN_POINT('Ctrl Pts',(2.00512659039881,0.172730921831388,-5.90472895251783));
#5873=CARTESIAN_POINT('Ctrl Pts',(2.00081326718839,0.115037005526063,-5.90175688067614));
#5874=CARTESIAN_POINT('Ctrl Pts',(1.99792588528997,0.0764161182281746,-5.89976734592118));
#5875=CARTESIAN_POINT('Ctrl Pts',(1.99649355035822,0.037688117570368,-5.89777781116623));
#5876=CARTESIAN_POINT('Ctrl Pts',(1.99651939415621,-0.0010299323318173,
-5.89578827641127));
#5877=CARTESIAN_POINT('Ctrl Pts',(4.49572832313563,-0.823999039924152,-6.49872963456835));
#5878=CARTESIAN_POINT('Ctrl Pts',(4.76877456504554,-0.507155625959688,-6.47236100750229));
#5879=CARTESIAN_POINT('Ctrl Pts',(4.97052119895137,0.41371606398221,-6.41963060186529));
#5880=CARTESIAN_POINT('Ctrl Pts',(3.97155283172513,1.42700839004805,-6.34053841765734));
#5881=CARTESIAN_POINT('Ctrl Pts',(2.58001075957843,1.1395105179617,-6.26145308194453));
#5882=CARTESIAN_POINT('Ctrl Pts',(2.0606601689097,-0.182061886182395,-6.18236774623168));
#5883=CARTESIAN_POINT('Ctrl Pts',(2.88560714750128,-1.33903079709423,-6.10328241051888));
#5884=CARTESIAN_POINT('Ctrl Pts',(4.30496409563768,-1.27835189863699,-6.02419707480604));
#5885=CARTESIAN_POINT('Ctrl Pts',(5.02852611711507,-0.0558761027051249,
-5.94511173909324));
#5886=CARTESIAN_POINT('Ctrl Pts',(4.39856758010236,1.21751315736083,-5.8660264033804));
#5887=CARTESIAN_POINT('Ctrl Pts',(2.98772827969131,1.38410915310173,-5.78694106766758));
#5888=CARTESIAN_POINT('Ctrl Pts',(2.07846881472217,0.292573992443711,-5.70785573195475));
#5889=CARTESIAN_POINT('Ctrl Pts',(2.49732074732185,-1.06493663159316,-5.62877039624192));
#5890=CARTESIAN_POINT('Ctrl Pts',(3.86353027867868,-1.45438919355478,-5.5496850605291));
#5891=CARTESIAN_POINT('Ctrl Pts',(4.93522883507102,-0.521820717995012,-5.47059972481628));
#5892=CARTESIAN_POINT('Ctrl Pts',(4.73818094463292,0.885140580293045,-5.39151438910345));
#5893=CARTESIAN_POINT('Ctrl Pts',(3.45160733055285,1.48740082812334,-5.31242905339063));
#5894=CARTESIAN_POINT('Ctrl Pts',(2.2448142609951,0.737796557718971,-5.2333437176778));
#5895=CARTESIAN_POINT('Ctrl Pts',(2.21517534366209,-0.682849813790565,-5.15425838196498));
#5896=CARTESIAN_POINT('Ctrl Pts',(3.38887522286638,-1.48204143598075,-5.07517304625216));
#5897=CARTESIAN_POINT('Ctrl Pts',(4.70048975466964,-0.93549620915041,-4.99608771053934));
#5898=CARTESIAN_POINT('Ctrl Pts',(4.95482897497733,0.464382385782661,-4.91700237482651));
#5899=CARTESIAN_POINT('Ctrl Pts',(4.26949223942085,1.11144110680237,-4.86427881768463));
#5900=CARTESIAN_POINT('Ctrl Pts',(3.86552663736113,1.21943825288345,-4.83791703911368));
#5901=CARTESIAN_POINT('Ctrl Pts',(4.56709408744317,-0.885497419986959,-6.55312057472045));
#5902=CARTESIAN_POINT('Ctrl Pts',(4.86051887440726,-0.54500670093076,-6.52675194765439));
#5903=CARTESIAN_POINT('Ctrl Pts',(5.07732267533294,0.444593366634419,-6.47402154201738));
#5904=CARTESIAN_POINT('Ctrl Pts',(4.00379725968579,1.53351179608608,-6.39492935780944));
#5905=CARTESIAN_POINT('Ctrl Pts',(2.50839877620863,1.22455679535254,-6.31584402209662));
#5906=CARTESIAN_POINT('Ctrl Pts',(1.95028695104414,-0.195649900887397,-6.23675868638379));
#5907=CARTESIAN_POINT('Ctrl Pts',(2.83680305819412,-1.43896807964627,-6.15767335067098));
#5908=CARTESIAN_POINT('Ctrl Pts',(4.36209235432126,-1.37376046965137,-6.07858801495814));
#5909=CARTESIAN_POINT('Ctrl Pts',(5.13965673507314,-0.0600463621764277,
-5.99950267924533));
#5910=CARTESIAN_POINT('Ctrl Pts',(4.46268184530282,1.3083810871217,-5.92041734353249));
#5911=CARTESIAN_POINT('Ctrl Pts',(2.94654590339056,1.48741081563,-5.84133200781968));
#5912=CARTESIAN_POINT('Ctrl Pts',(1.96942472810011,0.314409972477684,-5.76224667210684));
#5913=CARTESIAN_POINT('Ctrl Pts',(2.41953727399302,-1.14441715831629,-5.68316133639403));
#5914=CARTESIAN_POINT('Ctrl Pts',(3.88771254673291,-1.56293613966857,-5.60407600068119));
#5915=CARTESIAN_POINT('Ctrl Pts',(5.03939629963695,-0.560766308080723,-5.52499066496838));
#5916=CARTESIAN_POINT('Ctrl Pts',(4.82764192840266,0.951202200729989,-5.44590532925554));
#5917=CARTESIAN_POINT('Ctrl Pts',(3.44504612344143,1.59841156600245,-5.36681999354273));
#5918=CARTESIAN_POINT('Ctrl Pts',(2.14818520762059,0.79286129798834,-5.28773465782989));
#5919=CARTESIAN_POINT('Ctrl Pts',(2.11633421804662,-0.733813656391856,-5.20864932211708));
#5920=CARTESIAN_POINT('Ctrl Pts',(3.37763206491069,-1.59265218075439,-5.12956398640425));
#5921=CARTESIAN_POINT('Ctrl Pts',(4.78713769253389,-1.00531607377421,-5.05047865069143));
#5922=CARTESIAN_POINT('Ctrl Pts',(5.06045927723462,0.499041120892308,-4.9713933149786));
#5923=CARTESIAN_POINT('Ctrl Pts',(4.32397309004998,1.19439245054404,-4.91866975783672));
#5924=CARTESIAN_POINT('Ctrl Pts',(3.88985790173582,1.31044986030698,-4.89230797926578));
#5925=CARTESIAN_POINT('Ctrl Pts',(4.63845985175071,-0.946995800049766,-6.60751151487254));
#5926=CARTESIAN_POINT('Ctrl Pts',(4.95226318376898,-0.58285777590183,-6.58114288780649));
#5927=CARTESIAN_POINT('Ctrl Pts',(5.18412415171451,0.475470669286626,-6.52841248216948));
#5928=CARTESIAN_POINT('Ctrl Pts',(4.03604168764646,1.64001520212411,-6.44932029796154));
#5929=CARTESIAN_POINT('Ctrl Pts',(2.43678679283885,1.30960307274338,-6.37023496224872));
#5930=CARTESIAN_POINT('Ctrl Pts',(1.83991373317858,-0.209237915592398,-6.29114962653589));
#5931=CARTESIAN_POINT('Ctrl Pts',(2.78799896888696,-1.53890536219829,-6.21206429082307));
#5932=CARTESIAN_POINT('Ctrl Pts',(4.41922061300483,-1.46916904066575,-6.13297895511024));
#5933=CARTESIAN_POINT('Ctrl Pts',(5.25078735303124,-0.0642166216477319,
-6.05389361939743));
#5934=CARTESIAN_POINT('Ctrl Pts',(4.52679611050327,1.39924901688256,-5.97480828368459));
#5935=CARTESIAN_POINT('Ctrl Pts',(2.90536352708983,1.59071247815826,-5.89572294797179));
#5936=CARTESIAN_POINT('Ctrl Pts',(1.86038064147805,0.336245952511657,-5.81663761225893));
#5937=CARTESIAN_POINT('Ctrl Pts',(2.34175380066418,-1.22389768503941,-5.73755227654613));
#5938=CARTESIAN_POINT('Ctrl Pts',(3.91189481478717,-1.67148308578238,-5.6584669408333));
#5939=CARTESIAN_POINT('Ctrl Pts',(5.14356376420288,-0.599711898166432,-5.57938160512047));
#5940=CARTESIAN_POINT('Ctrl Pts',(4.91710291217238,1.01726382116693,-5.50029626940765));
#5941=CARTESIAN_POINT('Ctrl Pts',(3.43848491633001,1.70942230388156,-5.42121093369482));
#5942=CARTESIAN_POINT('Ctrl Pts',(2.05155615424608,0.847926038257708,-5.34212559798201));
#5943=CARTESIAN_POINT('Ctrl Pts',(2.01749309243115,-0.784777498993147,-5.26304026226917));
#5944=CARTESIAN_POINT('Ctrl Pts',(3.36638890695502,-1.70326292552803,-5.18395492655636));
#5945=CARTESIAN_POINT('Ctrl Pts',(4.87378563039813,-1.07513593839801,-5.10486959084353));
#5946=CARTESIAN_POINT('Ctrl Pts',(5.16608957949192,0.533699856001957,-5.0257842551307));
#5947=CARTESIAN_POINT('Ctrl Pts',(4.3784539406791,1.27734379428573,-4.97306069798882));
#5948=CARTESIAN_POINT('Ctrl Pts',(3.91418916611049,1.40146146773053,-4.94669891941788));
#5949=CARTESIAN_POINT('Ctrl Pts',(4.70982561605824,-1.00849418011257,-6.66190245502464));
#5950=CARTESIAN_POINT('Ctrl Pts',(5.0440074931307,-0.620708850872902,-6.63553382795858));
#5951=CARTESIAN_POINT('Ctrl Pts',(5.29092562809607,0.506347971938834,-6.58280342232159));
#5952=CARTESIAN_POINT('Ctrl Pts',(4.06828611560712,1.74651860816213,-6.50371123811363));
#5953=CARTESIAN_POINT('Ctrl Pts',(2.36517480946905,1.39464935013422,-6.42462590240083));
#5954=CARTESIAN_POINT('Ctrl Pts',(1.72954051531302,-0.2228259302974,-6.34554056668798));
#5955=CARTESIAN_POINT('Ctrl Pts',(2.7391948795798,-1.63884264475033,-6.26645523097519));
#5956=CARTESIAN_POINT('Ctrl Pts',(4.47634887168841,-1.56457761168014,-6.18736989526234));
#5957=CARTESIAN_POINT('Ctrl Pts',(5.36191797098931,-0.0683868811190347,
-6.10828455954952));
#5958=CARTESIAN_POINT('Ctrl Pts',(4.59091037570374,1.49011694664342,-6.0291992238367));
#5959=CARTESIAN_POINT('Ctrl Pts',(2.86418115078907,1.69401414068653,-5.95011388812387));
#5960=CARTESIAN_POINT('Ctrl Pts',(1.75133655485599,0.358081932545629,-5.87102855241105));
#5961=CARTESIAN_POINT('Ctrl Pts',(2.26397032733535,-1.30337821176254,-5.79194321669822));
#5962=CARTESIAN_POINT('Ctrl Pts',(3.93607708284141,-1.78003003189618,-5.71285788098541));
#5963=CARTESIAN_POINT('Ctrl Pts',(5.24773122876883,-0.638657488252143,-5.63377254527257));
#5964=CARTESIAN_POINT('Ctrl Pts',(5.00656389594211,1.08332544160388,-5.55468720955976));
#5965=CARTESIAN_POINT('Ctrl Pts',(3.43192370921861,1.82043304176068,-5.47560187384691));
#5966=CARTESIAN_POINT('Ctrl Pts',(1.95492710087157,0.902990778527077,-5.39651653813412));
#5967=CARTESIAN_POINT('Ctrl Pts',(1.91865196681568,-0.835741341594439,-5.31743120242126));
#5968=CARTESIAN_POINT('Ctrl Pts',(3.35514574899934,-1.81387367030167,-5.23834586670847));
#5969=CARTESIAN_POINT('Ctrl Pts',(4.96043356826237,-1.14495580302182,-5.15926053099562));
#5970=CARTESIAN_POINT('Ctrl Pts',(5.27171988174921,0.568358591111605,-5.08017519528281));
#5971=CARTESIAN_POINT('Ctrl Pts',(4.43293479130822,1.3602951380274,-5.02745163814092));
#5972=CARTESIAN_POINT('Ctrl Pts',(3.93852043048518,1.49247307515406,-5.00108985956998));
#5973=CARTESIAN_POINT('',(4.49856554501718,-0.825828034651814,-4.99935673527973));
#5974=CARTESIAN_POINT('Ctrl Pts',(3.93803289228021,1.49064942821852,-5.));
#5975=CARTESIAN_POINT('Ctrl Pts',(3.99409065643514,1.47016615192376,-5.));
#5976=CARTESIAN_POINT('Ctrl Pts',(4.04865786654016,1.44624046411167,-5.));
#5977=CARTESIAN_POINT('Ctrl Pts',(4.10155167689883,1.41915239541907,-5.));
#5978=CARTESIAN_POINT('Ctrl Pts',(4.15531048656907,1.39162134179853,-5.));
#5979=CARTESIAN_POINT('Ctrl Pts',(4.20734148705644,1.36082280343506,-5.));
#5980=CARTESIAN_POINT('Ctrl Pts',(4.25742159252753,1.32700667838438,-5.));
#5981=CARTESIAN_POINT('Ctrl Pts',(4.30733738857824,1.29330150174034,-5.));
#5982=CARTESIAN_POINT('Ctrl Pts',(4.35531573175224,1.2565975723992,-5.));
#5983=CARTESIAN_POINT('Ctrl Pts',(4.40109443402577,1.21711234501117,-5.));
#5984=CARTESIAN_POINT('Ctrl Pts',(4.41061728847052,1.20889865492255,-5.));
#5985=CARTESIAN_POINT('Ctrl Pts',(4.42004479737223,1.20056453633304,-5.));
#5986=CARTESIAN_POINT('Ctrl Pts',(4.42937433420408,1.19211184027005,-5.));
#5987=CARTESIAN_POINT('Ctrl Pts',(4.43709254019515,1.18511903338479,-5.));
#5988=CARTESIAN_POINT('Ctrl Pts',(4.44474353367624,1.17804508607658,-5.));
#5989=CARTESIAN_POINT('Ctrl Pts',(4.4523156979883,1.17090094418241,-5.));
#5990=CARTESIAN_POINT('Ctrl Pts',(4.49538755285076,1.13026375907898,-5.));
#5991=CARTESIAN_POINT('Ctrl Pts',(4.53599880545883,1.08728056038843,-5.));
#5992=CARTESIAN_POINT('Ctrl Pts',(4.57394274742331,1.0421920409728,-5.));
#5993=CARTESIAN_POINT('Ctrl Pts',(4.61123044145062,0.997883336366205,-5.));
#5994=CARTESIAN_POINT('Ctrl Pts',(4.64594276168599,0.951540565975969,-5.));
#5995=CARTESIAN_POINT('Ctrl Pts',(4.67784006477363,0.903368830373567,-5.));
#5996=CARTESIAN_POINT('Ctrl Pts',(4.70128120204354,0.867967709981565,-5.));
#5997=CARTESIAN_POINT('Ctrl Pts',(4.72320117972997,0.831578293288047,-5.));
#5998=CARTESIAN_POINT('Ctrl Pts',(4.74348727685767,0.794278015648549,-5.));
#5999=CARTESIAN_POINT('Ctrl Pts',(4.75387319409623,0.77518131143282,-5.));
#6000=CARTESIAN_POINT('Ctrl Pts',(4.76383059074213,0.755845823276845,-5.));
#6001=CARTESIAN_POINT('Ctrl Pts',(4.77334264614643,0.736281858177808,-5.));
#6002=CARTESIAN_POINT('Ctrl Pts',(4.77823393014549,0.72622168659768,-5.));
#6003=CARTESIAN_POINT('Ctrl Pts',(4.78300365060887,0.716108772548597,-5.));
#6004=CARTESIAN_POINT('Ctrl Pts',(4.78764749050887,0.705950521112731,-5.));
#6005=CARTESIAN_POINT('Ctrl Pts',(4.81080973037988,0.655283861302306,-5.));
#6006=CARTESIAN_POINT('Ctrl Pts',(4.83086651830312,0.603444698612965,-5.));
#6007=CARTESIAN_POINT('Ctrl Pts',(4.84760491848966,0.550623118129289,-5.));
#6008=CARTESIAN_POINT('Ctrl Pts',(4.8593983757285,0.513406356444801,-5.));
#6009=CARTESIAN_POINT('Ctrl Pts',(4.86954356797092,0.475701506087563,-5.));
#6010=CARTESIAN_POINT('Ctrl Pts',(4.87795053537239,0.437572846428279,-5.));
#6011=CARTESIAN_POINT('Ctrl Pts',(4.88985018734038,0.383603589943183,-5.));
#6012=CARTESIAN_POINT('Ctrl Pts',(4.89826878476809,0.328784212898911,-5.));
#6013=CARTESIAN_POINT('Ctrl Pts',(4.9032634076361,0.273432028782955,-5.));
#6014=CARTESIAN_POINT('Ctrl Pts',(4.90468835253674,0.257640283424103,-5.));
#6015=CARTESIAN_POINT('Ctrl Pts',(4.90583433078692,0.241805257431463,-5.));
#6016=CARTESIAN_POINT('Ctrl Pts',(4.90670202416689,0.225934580336756,-5.));
#6017=CARTESIAN_POINT('Ctrl Pts',(4.90737234904755,0.213673901651028,-5.));
#6018=CARTESIAN_POINT('Ctrl Pts',(4.90787651819931,0.201389247372144,-5.));
#6019=CARTESIAN_POINT('Ctrl Pts',(4.90821450591308,0.189107888094874,-5.));
#6020=CARTESIAN_POINT('Ctrl Pts',(4.90974223500557,0.133595249324311,-5.));
#6021=CARTESIAN_POINT('Ctrl Pts',(4.907886088605,0.078048827692731,-5.));
#6022=CARTESIAN_POINT('Ctrl Pts',(4.9027539571184,0.0227840637894804,-5.));
#6023=CARTESIAN_POINT('Ctrl Pts',(4.89762247605141,-0.0324736961456407,
-5.));
#6024=CARTESIAN_POINT('Ctrl Pts',(4.88921538506426,-0.0874510038276154,
-5.));
#6025=CARTESIAN_POINT('Ctrl Pts',(4.87759161308525,-0.14181744386592,-5.));
#6026=CARTESIAN_POINT('Ctrl Pts',(4.87038507021592,-0.175523721096468,-5.));
#6027=CARTESIAN_POINT('Ctrl Pts',(4.86194116529405,-0.208994828372916,-5.));
#6028=CARTESIAN_POINT('Ctrl Pts',(4.85226563868636,-0.242146239785466,-5.));
#6029=CARTESIAN_POINT('Ctrl Pts',(4.84728116924316,-0.259224607081082,-5.));
#6030=CARTESIAN_POINT('Ctrl Pts',(4.84196973886336,-0.276218043618959,-5.));
#6031=CARTESIAN_POINT('Ctrl Pts',(4.83633153787352,-0.293114371811587,-5.));
#6032=CARTESIAN_POINT('Ctrl Pts',(4.83137886705509,-0.307956331459553,-5.00000000000001));
#6033=CARTESIAN_POINT('Ctrl Pts',(4.82617357016375,-0.322723784665042,-5.));
#6034=CARTESIAN_POINT('Ctrl Pts',(4.82072625926819,-0.33738190195413,-5.));
#6035=CARTESIAN_POINT('Ctrl Pts',(4.8020408199964,-0.38766237349243,-5.));
#6036=CARTESIAN_POINT('Ctrl Pts',(4.78048542226647,-0.436737790266667,-5.));
#6037=CARTESIAN_POINT('Ctrl Pts',(4.75610356324102,-0.484292455085576,-5.));
#6038=CARTESIAN_POINT('Ctrl Pts',(4.74073117822194,-0.514274935760493,-5.));
#6039=CARTESIAN_POINT('Ctrl Pts',(4.72423443746592,-0.543652342157504,-5.));
#6040=CARTESIAN_POINT('Ctrl Pts',(4.70661689619086,-0.572337713302352,-5.));
#6041=CARTESIAN_POINT('Ctrl Pts',(4.69812236738934,-0.586168741569455,-5.));
#6042=CARTESIAN_POINT('Ctrl Pts',(4.68936481385441,-0.599841995803325,-5.));
#6043=CARTESIAN_POINT('Ctrl Pts',(4.68035979413337,-0.613324827934156,-5.));
#6044=CARTESIAN_POINT('Ctrl Pts',(4.65190463621292,-0.655929522802452,-5.));
#6045=CARTESIAN_POINT('Ctrl Pts',(4.62095551630975,-0.696679989535698,-5.));
#6046=CARTESIAN_POINT('Ctrl Pts',(4.58753688857224,-0.735275095170701,-5.));
#6047=CARTESIAN_POINT('Ctrl Pts',(4.56897483790831,-0.756712369968577,-5.));
#6048=CARTESIAN_POINT('Ctrl Pts',(4.54965034106223,-0.777484018727688,-5.));
#6049=CARTESIAN_POINT('Ctrl Pts',(4.52956373601773,-0.797532559017432,-5.));
#6050=CARTESIAN_POINT('Ctrl Pts',(4.51970691265084,-0.807370703390872,-5.));
#6051=CARTESIAN_POINT('Ctrl Pts',(4.50966652692015,-0.817034646361409,-5.));
#6052=CARTESIAN_POINT('Ctrl Pts',(4.49944832123852,-0.826521983932989,-5.));
#6053=CARTESIAN_POINT('Ctrl Pts',(4.4976352031454,-0.825211298936469,-6.5));
#6054=CARTESIAN_POINT('Ctrl Pts',(4.53473403611661,-0.790565919373912,-6.5));
#6055=CARTESIAN_POINT('Ctrl Pts',(4.56942439597947,-0.753655314382007,-6.5));
#6056=CARTESIAN_POINT('Ctrl Pts',(4.60170505482589,-0.714805016616039,-6.5));
#6057=CARTESIAN_POINT('Ctrl Pts',(4.63521429205091,-0.674476104796233,-6.5));
#6058=CARTESIAN_POINT('Ctrl Pts',(4.66612750740978,-0.632056529770239,-6.5));
#6059=CARTESIAN_POINT('Ctrl Pts',(4.69441520294597,-0.587860718560562,-6.5));
#6060=CARTESIAN_POINT('Ctrl Pts',(4.71720257347233,-0.552258443201673,-6.5));
#6061=CARTESIAN_POINT('Ctrl Pts',(4.73828573819916,-0.515502374121504,-6.5));
#6062=CARTESIAN_POINT('Ctrl Pts',(4.75763279341486,-0.477738744113682,-6.5));
#6063=CARTESIAN_POINT('Ctrl Pts',(4.76647244363112,-0.460484579257903,-6.5));
#6064=CARTESIAN_POINT('Ctrl Pts',(4.77494945031063,-0.443019888823993,-6.5));
#6065=CARTESIAN_POINT('Ctrl Pts',(4.78305959925634,-0.425357785247147,-6.5));
#6066=CARTESIAN_POINT('Ctrl Pts',(4.78684697504658,-0.417109721748024,-6.5));
#6067=CARTESIAN_POINT('Ctrl Pts',(4.79055297375982,-0.408821425564243,-6.5));
#6068=CARTESIAN_POINT('Ctrl Pts',(4.7941739531994,-0.40050235122582,-6.5));
#6069=CARTESIAN_POINT('Ctrl Pts',(4.81595160644151,-0.350468950246823,-6.5));
#6070=CARTESIAN_POINT('Ctrl Pts',(4.83469510425185,-0.299242701997503,-6.5));
#6071=CARTESIAN_POINT('Ctrl Pts',(4.85037713536496,-0.247156898168492,-6.5));
#6072=CARTESIAN_POINT('Ctrl Pts',(4.86632338221363,-0.194193536523689,-6.5));
#6073=CARTESIAN_POINT('Ctrl Pts',(4.87910472028871,-0.14034047034307,-6.5));
#6074=CARTESIAN_POINT('Ctrl Pts',(4.88865141719124,-0.0859136452486175,
-6.5));
#6075=CARTESIAN_POINT('Ctrl Pts',(4.89555760061471,-0.0465406934206672,
-6.5));
#6076=CARTESIAN_POINT('Ctrl Pts',(4.90077019034692,-0.00686669826656089,
-6.5));
#6077=CARTESIAN_POINT('Ctrl Pts',(4.90424708276949,0.0329952762835868,-6.5));
#6078=CARTESIAN_POINT('Ctrl Pts',(4.90544059215015,0.0466786563756833,-6.5));
#6079=CARTESIAN_POINT('Ctrl Pts',(4.9064294554003,0.060384216236401,-6.5));
#6080=CARTESIAN_POINT('Ctrl Pts',(4.90721157306747,0.0741074501673721,-6.5));
#6081=CARTESIAN_POINT('Ctrl Pts',(4.90776877420489,0.0838842419165997,-6.5));
#6082=CARTESIAN_POINT('Ctrl Pts',(4.90822089056527,0.0936690684444187,-6.5));
#6083=CARTESIAN_POINT('Ctrl Pts',(4.90856697997868,0.103447389902126,-6.5));
#6084=CARTESIAN_POINT('Ctrl Pts',(4.91057764169525,0.16025610997759,-6.5));
#6085=CARTESIAN_POINT('Ctrl Pts',(4.90902053110958,0.216957470431213,-6.49999999999999));
#6086=CARTESIAN_POINT('Ctrl Pts',(4.90383821984126,0.273218400759099,-6.5));
#6087=CARTESIAN_POINT('Ctrl Pts',(4.90018706316735,0.312856597040903,-6.5));
#6088=CARTESIAN_POINT('Ctrl Pts',(4.89473554441125,0.352276864102268,-6.5));
#6089=CARTESIAN_POINT('Ctrl Pts',(4.88744880947781,0.39136760658551,-6.5));
#6090=CARTESIAN_POINT('Ctrl Pts',(4.87737256927013,0.445423053195733,-6.5));
#6091=CARTESIAN_POINT('Ctrl Pts',(4.86378936361766,0.498849002961625,-6.5));
#6092=CARTESIAN_POINT('Ctrl Pts',(4.8469261375644,0.551442578692384,-6.5));
#6093=CARTESIAN_POINT('Ctrl Pts',(4.84228985765719,0.565902358667974,-6.5));
#6094=CARTESIAN_POINT('Ctrl Pts',(4.83740534317848,0.580299187094379,-6.5));
#6095=CARTESIAN_POINT('Ctrl Pts',(4.83227664561688,0.594628735492603,-6.5));
#6096=CARTESIAN_POINT('Ctrl Pts',(4.8279040034594,0.606845869895838,-6.5));
#6097=CARTESIAN_POINT('Ctrl Pts',(4.82335243093813,0.619017360734909,-6.5));
#6098=CARTESIAN_POINT('Ctrl Pts',(4.81863426849385,0.631116085607377,-6.5));
#6099=CARTESIAN_POINT('Ctrl Pts',(4.79819471062682,0.68352898789047,-6.5));
#6100=CARTESIAN_POINT('Ctrl Pts',(4.77460300293305,0.734665692265129,-6.5));
#6101=CARTESIAN_POINT('Ctrl Pts',(4.7481393208072,0.784323343086663,-6.5));
#6102=CARTESIAN_POINT('Ctrl Pts',(4.72080038497767,0.835623359569603,-6.5));
#6103=CARTESIAN_POINT('Ctrl Pts',(4.69039609513946,0.885345769139235,-6.5));
#6104=CARTESIAN_POINT('Ctrl Pts',(4.65717979150465,0.933261327103311,-6.5));
#6105=CARTESIAN_POINT('Ctrl Pts',(4.63626695867212,0.963428743225127,-6.5));
#6106=CARTESIAN_POINT('Ctrl Pts',(4.61423837261579,0.9928797854586,-6.5));
#6107=CARTESIAN_POINT('Ctrl Pts',(4.59114735991414,1.02155360927412,-6.5));
#6108=CARTESIAN_POINT('Ctrl Pts',(4.58004021989682,1.03534616917896,-6.5));
#6109=CARTESIAN_POINT('Ctrl Pts',(4.56868715418712,1.04895884536489,-6.5));
#6110=CARTESIAN_POINT('Ctrl Pts',(4.55709354204463,1.0623845162606,-6.5));
#6111=CARTESIAN_POINT('Ctrl Pts',(4.54985583002559,1.07076595410856,-6.5));
#6112=CARTESIAN_POINT('Ctrl Pts',(4.54252436265672,1.07907450530581,-6.5));
#6113=CARTESIAN_POINT('Ctrl Pts',(4.53510038293429,1.0873083833382,-6.5));
#6114=CARTESIAN_POINT('Ctrl Pts',(4.52747285907183,1.09576801058945,-6.5));
#6115=CARTESIAN_POINT('Ctrl Pts',(4.51975341789829,1.10414241451658,-6.5));
#6116=CARTESIAN_POINT('Ctrl Pts',(4.51194611870614,1.11242760866335,-6.5));
#6117=CARTESIAN_POINT('Ctrl Pts',(4.47050176490355,1.15640882535441,-6.5));
#6118=CARTESIAN_POINT('Ctrl Pts',(4.42656593670862,1.19789966714169,-6.5));
#6119=CARTESIAN_POINT('Ctrl Pts',(4.3803955573361,1.23664844871276,-6.5));
#6120=CARTESIAN_POINT('Ctrl Pts',(4.34807267706821,1.26377562947823,-6.5));
#6121=CARTESIAN_POINT('Ctrl Pts',(4.31465351835422,1.28955859641289,-6.5));
#6122=CARTESIAN_POINT('Ctrl Pts',(4.28021363858723,1.3139024861197,-6.5));
#6123=CARTESIAN_POINT('Ctrl Pts',(4.26678858690377,1.32339200756117,-6.5));
#6124=CARTESIAN_POINT('Ctrl Pts',(4.25320628510412,1.33266389379897,-6.5));
#6125=CARTESIAN_POINT('Ctrl Pts',(4.23949101849253,1.34169951148356,-6.5));
#6126=CARTESIAN_POINT('Ctrl Pts',(4.18870128727318,1.37515978656226,-6.5));
#6127=CARTESIAN_POINT('Ctrl Pts',(4.13603515427771,1.40542369855342,-6.5));
#6128=CARTESIAN_POINT('Ctrl Pts',(4.08173184346464,1.4322271097713,-6.5));
#6129=CARTESIAN_POINT('Ctrl Pts',(4.05045913624191,1.44766291320642,-6.5));
#6130=CARTESIAN_POINT('Ctrl Pts',(4.01864270350732,1.46195048487063,-6.5));
#6131=CARTESIAN_POINT('Ctrl Pts',(3.98632298496835,1.47503347997995,-6.5));
#6132=CARTESIAN_POINT('Ctrl Pts',(3.97074861183692,1.48133797323423,-6.5));
#6133=CARTESIAN_POINT('Ctrl Pts',(3.9550573186525,1.48736267540842,-6.5));
#6134=CARTESIAN_POINT('Ctrl Pts',(3.93925596516474,1.49310957330526,-6.49999999999999));
#6135=CARTESIAN_POINT('Ctrl Pts',(4.49772637506564,-0.825105431445688,-4.99935673527973));
#6136=CARTESIAN_POINT('Ctrl Pts',(4.49344280469424,-0.830080006026179,-4.99957115685316));
#6137=CARTESIAN_POINT('Ctrl Pts',(4.48912049496684,-0.835021222417506,-4.99978557842658));
#6138=CARTESIAN_POINT('Ctrl Pts',(4.48475997009368,-0.83992848134833,-5.));
#6139=CARTESIAN_POINT('Ctrl Pts',(3.14049567003405,1.49255536784005,-6.49886096014758));
#6140=CARTESIAN_POINT('Ctrl Pts',(2.64605404795825,1.36037014262379,-6.47249918157664));
#6141=CARTESIAN_POINT('Ctrl Pts',(1.80722122039271,0.568399038714978,-6.41977562443476));
#6142=CARTESIAN_POINT('Ctrl Pts',(2.11852749381716,-1.14502364307201,-6.34069028872192));
#6143=CARTESIAN_POINT('Ctrl Pts',(3.72390230442703,-1.8139700754625,-6.26160495300911));
#6144=CARTESIAN_POINT('Ctrl Pts',(5.16047486326952,-0.835788897306109,-6.18251961729628));
#6145=CARTESIAN_POINT('Ctrl Pts',(5.12419795286652,0.903041288099895,-6.10343428158346));
#6146=CARTESIAN_POINT('Ctrl Pts',(3.64712017679401,1.82053219154147,-6.02434894587063));
#6147=CARTESIAN_POINT('Ctrl Pts',(2.07239390111447,1.08338514516621,-5.9452636101578));
#6148=CARTESIAN_POINT('Ctrl Pts',(1.83121321908415,-0.638692684208562,-5.86617827444498));
#6149=CARTESIAN_POINT('Ctrl Pts',(3.14293932672556,-1.78012743927191,-5.78709293873216));
#6150=CARTESIAN_POINT('Ctrl Pts',(4.81513763610179,-1.3034497215919,-5.70800760301933));
#6151=CARTESIAN_POINT('Ctrl Pts',(5.32779955515347,0.35810164653081,-5.62892226730652));
#6152=CARTESIAN_POINT('Ctrl Pts',(4.21489391379536,1.69410683583459,-5.54983693159369));
#6153=CARTESIAN_POINT('Ctrl Pts',(2.48807018469715,1.4901987924474,-5.47075159588087));
#6154=CARTESIAN_POINT('Ctrl Pts',(1.71702014690403,-0.0683909582657119,
-5.39166626016802));
#6155=CARTESIAN_POINT('Ctrl Pts',(2.60263814280788,-1.56466278404689,-5.31258092445522));
#6156=CARTESIAN_POINT('Ctrl Pts',(4.3398865979832,-1.63893336675877,-5.2334955887424));
#6157=CARTESIAN_POINT('Ctrl Pts',(5.34959768449681,-0.222836636419013,-5.15441025302956));
#6158=CARTESIAN_POINT('Ctrl Pts',(4.7139258330361,1.39472338762311,-5.07532491731675));
#6159=CARTESIAN_POINT('Ctrl Pts',(3.01072656391766,1.74661806167074,-4.99623958160391));
#6160=CARTESIAN_POINT('Ctrl Pts',(1.7881154138621,0.506476594702042,-4.9171542458911));
#6161=CARTESIAN_POINT('Ctrl Pts',(2.03488352866203,-0.620450306009015,-4.86443068874921));
#6162=CARTESIAN_POINT('Ctrl Pts',(2.36888760166378,-1.0082475863304,-4.83806891017827));
#6163=CARTESIAN_POINT('Ctrl Pts',(3.16479427350219,1.40166592922615,-6.55317888899264));
#6164=CARTESIAN_POINT('Ctrl Pts',(2.70046176658963,1.27753014805185,-6.5268171104217));
#6165=CARTESIAN_POINT('Ctrl Pts',(1.9127098211348,0.533786272816551,-6.47409355327982));
#6166=CARTESIAN_POINT('Ctrl Pts',(2.20505904074524,-1.07529721391509,-6.39500821756699));
#6167=CARTESIAN_POINT('Ctrl Pts',(3.71267425164766,-1.70350802804124,-6.31592288185417));
#6168=CARTESIAN_POINT('Ctrl Pts',(5.06176645551324,-0.784893375898539,-6.23683754614134));
#6169=CARTESIAN_POINT('Ctrl Pts',(5.0276986343623,0.848050419761554,-6.15775221042852));
#6170=CARTESIAN_POINT('Ctrl Pts',(3.64056778605475,1.70967054283278,-6.0786668747157));
#6171=CARTESIAN_POINT('Ctrl Pts',(2.16173476180896,1.01741220388143,-5.99958153900286));
#6172=CARTESIAN_POINT('Ctrl Pts',(1.93524082257328,-0.599799373604929,-5.92049620329005));
#6173=CARTESIAN_POINT('Ctrl Pts',(3.16708912326188,-1.6717262455187,-5.84141086757722));
#6174=CARTESIAN_POINT('Ctrl Pts',(4.7374586034602,-1.22407590671736,-5.7623255318644));
#6175=CARTESIAN_POINT('Ctrl Pts',(5.21890187895245,0.336294979708794,-5.68324019615157));
#6176=CARTESIAN_POINT('Ctrl Pts',(4.1737668350226,1.59094388283553,-5.60415486043875));
#6177=CARTESIAN_POINT('Ctrl Pts',(2.55209836026517,1.39945285793332,-5.52506952472592));
#6178=CARTESIAN_POINT('Ctrl Pts',(1.82800155890686,-0.064226278055535,-5.4459841890131));
#6179=CARTESIAN_POINT('Ctrl Pts',(2.65968968111326,-1.46938235082056,-5.36689885330027));
#6180=CARTESIAN_POINT('Ctrl Pts',(4.29114806630124,-1.53913021249062,-5.28781351758746));
#6181=CARTESIAN_POINT('Ctrl Pts',(5.23937260712761,-0.209266957716878,-5.20872818187462));
#6182=CARTESIAN_POINT('Ctrl Pts',(4.64241011209466,1.30979144576409,-5.12964284616181));
#6183=CARTESIAN_POINT('Ctrl Pts',(3.04292748140275,1.64025742774137,-5.05055751044898));
#6184=CARTESIAN_POINT('Ctrl Pts',(1.89476746627053,0.475634607627104,-4.97147217473615));
#6185=CARTESIAN_POINT('Ctrl Pts',(2.12650859051101,-0.58266786844183,-4.91874861759427));
#6186=CARTESIAN_POINT('Ctrl Pts',(2.44017342294322,-0.946850160760849,-4.89238683902333));
#6187=CARTESIAN_POINT('Ctrl Pts',(3.18909287697032,1.31077649061224,-6.6074968178377));
#6188=CARTESIAN_POINT('Ctrl Pts',(2.754869485221,1.19469015347991,-6.58113503926676));
#6189=CARTESIAN_POINT('Ctrl Pts',(2.01819842187689,0.499173506918126,-6.52841148212487));
#6190=CARTESIAN_POINT('Ctrl Pts',(2.29159058767332,-1.00557078475819,-6.44932614641205));
#6191=CARTESIAN_POINT('Ctrl Pts',(3.7014461988683,-1.59304598061997,-6.37024081069922));
#6192=CARTESIAN_POINT('Ctrl Pts',(4.96305804775698,-0.733997854490971,-6.29115547498641));
#6193=CARTESIAN_POINT('Ctrl Pts',(4.93119931585807,0.793059551423215,-6.21207013927357));
#6194=CARTESIAN_POINT('Ctrl Pts',(3.63401539531548,1.5988088941241,-6.13298480356076));
#6195=CARTESIAN_POINT('Ctrl Pts',(2.25107562250343,0.951439262596645,-6.05389946784793));
#6196=CARTESIAN_POINT('Ctrl Pts',(2.03926842606242,-0.560906063001296,-5.9748141321351));
#6197=CARTESIAN_POINT('Ctrl Pts',(3.19123891979818,-1.56332505176548,-5.89572879642229));
#6198=CARTESIAN_POINT('Ctrl Pts',(4.65977957081863,-1.14470209184282,-5.81664346070945));
#6199=CARTESIAN_POINT('Ctrl Pts',(5.11000420275143,0.314488312886777,-5.73755812499664));
#6200=CARTESIAN_POINT('Ctrl Pts',(4.13263975624985,1.48778092983647,-5.65847278928381));
#6201=CARTESIAN_POINT('Ctrl Pts',(2.61612653583318,1.30870692341923,-5.57938745357099));
#6202=CARTESIAN_POINT('Ctrl Pts',(1.93898297090969,-0.0600615978453574,
-5.50030211785817));
#6203=CARTESIAN_POINT('Ctrl Pts',(2.71674121941864,-1.37410191759422,-5.42121678214533));
#6204=CARTESIAN_POINT('Ctrl Pts',(4.24240953461929,-1.43932705822246,-5.34213144643252));
#6205=CARTESIAN_POINT('Ctrl Pts',(5.12914752975841,-0.195697279014745,-5.26304611071968));
#6206=CARTESIAN_POINT('Ctrl Pts',(4.57089439115325,1.22485950390509,-5.18396077500686));
#6207=CARTESIAN_POINT('Ctrl Pts',(3.07512839888781,1.53389679381199,-5.10487543929403));
#6208=CARTESIAN_POINT('Ctrl Pts',(2.00141951867897,0.444792620552168,-5.02579010358122));
#6209=CARTESIAN_POINT('Ctrl Pts',(2.21813365236001,-0.544885430874644,-4.97306654643933));
#6210=CARTESIAN_POINT('Ctrl Pts',(2.51145924422265,-0.885452735191297,-4.94670476786839));
#6211=CARTESIAN_POINT('Ctrl Pts',(3.21339148043844,1.21988705199834,-6.66181474668277));
#6212=CARTESIAN_POINT('Ctrl Pts',(2.80927720385237,1.11185015890796,-6.63545296811183));
#6213=CARTESIAN_POINT('Ctrl Pts',(2.12368702261897,0.4645607410197,-6.58272941096994));
#6214=CARTESIAN_POINT('Ctrl Pts',(2.37812213460139,-0.935844355601279,-6.50364407525712));
#6215=CARTESIAN_POINT('Ctrl Pts',(3.69021814608893,-1.48258393319871,-6.4245587395443));
#6216=CARTESIAN_POINT('Ctrl Pts',(4.86434964000071,-0.6831023330834,-6.34547340383148));
#6217=CARTESIAN_POINT('Ctrl Pts',(4.83469999735384,0.738068683084873,-6.26638806811864));
#6218=CARTESIAN_POINT('Ctrl Pts',(3.6274630045762,1.48794724541542,-6.18730273240583));
#6219=CARTESIAN_POINT('Ctrl Pts',(2.34041648319791,0.885466321311861,-6.108217396693));
#6220=CARTESIAN_POINT('Ctrl Pts',(2.14329602955155,-0.522012752397661,-6.02913206098017));
#6221=CARTESIAN_POINT('Ctrl Pts',(3.21538871633449,-1.45492385801227,-5.95004672526736));
#6222=CARTESIAN_POINT('Ctrl Pts',(4.58210053817705,-1.06532827696828,-5.87096138955452));
#6223=CARTESIAN_POINT('Ctrl Pts',(5.00110652655041,0.29268164606476,-5.79187605384172));
#6224=CARTESIAN_POINT('Ctrl Pts',(4.0915126774771,1.3846179768374,-5.71279071812886));
#6225=CARTESIAN_POINT('Ctrl Pts',(2.68015471140121,1.21796098890514,-5.63370538241607));
#6226=CARTESIAN_POINT('Ctrl Pts',(2.04996438291253,-0.0558969176351795,
-5.55462004670322));
#6227=CARTESIAN_POINT('Ctrl Pts',(2.77379275772401,-1.27882148436788,-5.4755347109904));
#6228=CARTESIAN_POINT('Ctrl Pts',(4.19367100293735,-1.33952390395431,-5.39644937527758));
#6229=CARTESIAN_POINT('Ctrl Pts',(5.0189224523892,-0.182127600312612,-5.31736403956475));
#6230=CARTESIAN_POINT('Ctrl Pts',(4.49937867021184,1.13992756204607,-5.23827870385193));
#6231=CARTESIAN_POINT('Ctrl Pts',(3.10732931637288,1.42753615988261,-5.15919336813911));
#6232=CARTESIAN_POINT('Ctrl Pts',(2.1080715710874,0.413950633477231,-5.08010803242628));
#6233=CARTESIAN_POINT('Ctrl Pts',(2.30975871420901,-0.507102993307459,-5.0273844752844));
#6234=CARTESIAN_POINT('Ctrl Pts',(2.58274506550209,-0.824055309621745,-5.00102269671346));
#6235=CARTESIAN_POINT('Ctrl Pts',(2.58140289770062,-0.825211298936501,-5.));
#6236=CARTESIAN_POINT('Ctrl Pts',(2.5443038685143,-0.790565736135109,-5.));
#6237=CARTESIAN_POINT('Ctrl Pts',(2.5096133001869,-0.753654963622072,-5.));
#6238=CARTESIAN_POINT('Ctrl Pts',(2.4773324300738,-0.714804509422556,-5.));
#6239=CARTESIAN_POINT('Ctrl Pts',(2.44382302669503,-0.674475499186495,-5.));
#6240=CARTESIAN_POINT('Ctrl Pts',(2.41290963390399,-0.632055844314543,-5.));
#6241=CARTESIAN_POINT('Ctrl Pts',(2.38462175988235,-0.587859965043762,-5.));
#6242=CARTESIAN_POINT('Ctrl Pts',(2.36183436288275,-0.552257818133782,-5.));
#6243=CARTESIAN_POINT('Ctrl Pts',(2.34075115345325,-0.515501897022739,-5.));
#6244=CARTESIAN_POINT('Ctrl Pts',(2.32140404015463,-0.477738428764528,-5.));
#6245=CARTESIAN_POINT('Ctrl Pts',(2.31256386104482,-0.460483357268475,-5.));
#6246=CARTESIAN_POINT('Ctrl Pts',(2.30408636388687,-0.443017739150525,-5.));
#6247=CARTESIAN_POINT('Ctrl Pts',(2.29597576406928,-0.425354688536879,-5.));
#6248=CARTESIAN_POINT('Ctrl Pts',(2.29064587076453,-0.413747387310767,-5.));
#6249=CARTESIAN_POINT('Ctrl Pts',(2.28547842331998,-0.402063202260178,-5.));
#6250=CARTESIAN_POINT('Ctrl Pts',(2.28047895461962,-0.390318443110687,-5.));
#6251=CARTESIAN_POINT('Ctrl Pts',(2.25908332594452,-0.340055801077734,-5.));
#6252=CARTESIAN_POINT('Ctrl Pts',(2.24073091648794,-0.288620954181535,-5.));
#6253=CARTESIAN_POINT('Ctrl Pts',(2.22545160263789,-0.236345852796058,-5.));
#6254=CARTESIAN_POINT('Ctrl Pts',(2.20993735019612,-0.183266956238725,-5.));
#6255=CARTESIAN_POINT('Ctrl Pts',(2.19759084383281,-0.12932081162433,-5.));
#6256=CARTESIAN_POINT('Ctrl Pts',(2.18848488354503,-0.0748214956571345,
-5.));
#6257=CARTESIAN_POINT('Ctrl Pts',(2.18251502859455,-0.039091819605201,-5.));
#6258=CARTESIAN_POINT('Ctrl Pts',(2.17793885768262,-0.00312372539428411,
-5.));
#6259=CARTESIAN_POINT('Ctrl Pts',(2.17478819450278,0.0329987838147586,-5.));
#6260=CARTESIAN_POINT('Ctrl Pts',(2.17359339586394,0.0466972093114556,-5.));
#6261=CARTESIAN_POINT('Ctrl Pts',(2.17260369603544,0.0604178640169256,-5.));
#6262=CARTESIAN_POINT('Ctrl Pts',(2.17182120172493,0.0741562274991369,-5.));
#6263=CARTESIAN_POINT('Ctrl Pts',(2.17126458820083,0.0839287700089929,-5.));
#6264=CARTESIAN_POINT('Ctrl Pts',(2.17081297188068,0.0937093000099677,-5.));
#6265=CARTESIAN_POINT('Ctrl Pts',(2.17046729064728,0.103483333436382,-5.));
#6266=CARTESIAN_POINT('Ctrl Pts',(2.16845812804063,0.160291804880593,-5.));
#6267=CARTESIAN_POINT('Ctrl Pts',(2.17001676354188,0.21699286492916,-5.));
#6268=CARTESIAN_POINT('Ctrl Pts',(2.17520064633437,0.273253460289501,-5.));
#6269=CARTESIAN_POINT('Ctrl Pts',(2.17885174648405,0.312878790638097,-5.));
#6270=CARTESIAN_POINT('Ctrl Pts',(2.18430208543024,0.352286313487869,-5.));
#6271=CARTESIAN_POINT('Ctrl Pts',(2.19158648959198,0.391364544701194,-5.));
#6272=CARTESIAN_POINT('Ctrl Pts',(2.20166270408611,0.445419842981498,-5.));
#6273=CARTESIAN_POINT('Ctrl Pts',(2.21524590860259,0.498845689754294,-5.));
#6274=CARTESIAN_POINT('Ctrl Pts',(2.23210915118275,0.55143920077537,-5.));
#6275=CARTESIAN_POINT('Ctrl Pts',(2.23674543347051,0.565898956213224,-5.));
#6276=CARTESIAN_POINT('Ctrl Pts',(2.24162995143373,0.580295763058249,-5.));
#6277=CARTESIAN_POINT('Ctrl Pts',(2.24675865344609,0.594625292699198,-5.));
#6278=CARTESIAN_POINT('Ctrl Pts',(2.25113136684655,0.606842599560134,-5.));
#6279=CARTESIAN_POINT('Ctrl Pts',(2.25568301689667,0.619014263661864,-5.));
#6280=CARTESIAN_POINT('Ctrl Pts',(2.26040126263906,0.631113161664277,-5.));
#6281=CARTESIAN_POINT('Ctrl Pts',(2.2808408613784,0.68352599343681,-5.));
#6282=CARTESIAN_POINT('Ctrl Pts',(2.30443261947429,0.734662665201017,-5.));
#6283=CARTESIAN_POINT('Ctrl Pts',(2.33089635496046,0.784320314073398,-5.));
#6284=CARTESIAN_POINT('Ctrl Pts',(2.35823540126121,0.835620432396352,-5.));
#6285=CARTESIAN_POINT('Ctrl Pts',(2.38863981713511,0.885342970150477,-5.));
#6286=CARTESIAN_POINT('Ctrl Pts',(2.42185625359725,0.933258674009797,-5.));
#6287=CARTESIAN_POINT('Ctrl Pts',(2.44276922138912,0.963426256034342,-5.));
#6288=CARTESIAN_POINT('Ctrl Pts',(2.46479795057879,0.992877467689253,-5.));
#6289=CARTESIAN_POINT('Ctrl Pts',(2.48788911204523,1.02155146193549,-5.));
#6290=CARTESIAN_POINT('Ctrl Pts',(2.49899636447663,1.03534415455392,-5.));
#6291=CARTESIAN_POINT('Ctrl Pts',(2.51034954571346,1.04895696236408,-5.));
#6292=CARTESIAN_POINT('Ctrl Pts',(2.52194327615918,1.06238276343662,-5.));
#6293=CARTESIAN_POINT('Ctrl Pts',(2.52918083973574,1.07076402512661,-5.));
#6294=CARTESIAN_POINT('Ctrl Pts',(2.53651215398541,1.07907240407868,-5.));
#6295=CARTESIAN_POINT('Ctrl Pts',(2.54393597594497,1.08730611385574,-5.));
#6296=CARTESIAN_POINT('Ctrl Pts',(2.56001623173551,1.10514061474239,-5.));
#6297=CARTESIAN_POINT('Ctrl Pts',(2.57650160603444,1.12259268997826,-5.));
#6298=CARTESIAN_POINT('Ctrl Pts',(2.59336983697945,1.13964202052506,-5.));
#6299=CARTESIAN_POINT('Ctrl Pts',(2.63584485418862,1.18257305524596,-5.));
#6300=CARTESIAN_POINT('Ctrl Pts',(2.68075393598663,1.22296307876887,-5.));
#6301=CARTESIAN_POINT('Ctrl Pts',(2.72784980179568,1.26055525794552,-5.));
#6302=CARTESIAN_POINT('Ctrl Pts',(2.75098798760318,1.27902428514687,-5.));
#6303=CARTESIAN_POINT('Ctrl Pts',(2.77465471369495,1.29681760412996,-5.));
#6304=CARTESIAN_POINT('Ctrl Pts',(2.79882434356303,1.31390198293556,-5.));
#6305=CARTESIAN_POINT('Ctrl Pts',(2.81224950241102,1.32339159864487,-5.));
#6306=CARTESIAN_POINT('Ctrl Pts',(2.82583191164499,1.33266357611002,-5.));
#6307=CARTESIAN_POINT('Ctrl Pts',(2.83954728536104,1.34169928144364,-5.));
#6308=CARTESIAN_POINT('Ctrl Pts',(2.89033718890059,1.37515973332831,-5.));
#6309=CARTESIAN_POINT('Ctrl Pts',(2.94300347308374,1.40542380145655,-5.));
#6310=CARTESIAN_POINT('Ctrl Pts',(2.99730690408547,1.43222733834652,-5.));
#6311=CARTESIAN_POINT('Ctrl Pts',(3.0285797562309,1.44766325152312,-5.));
#6312=CARTESIAN_POINT('Ctrl Pts',(3.06039632623927,1.46195091726861,-5.));
#6313=CARTESIAN_POINT('Ctrl Pts',(3.0927161721997,1.47503398848531,-5.));
#6314=CARTESIAN_POINT('Ctrl Pts',(3.10834477213784,1.48136044456614,-5.));
#6315=CARTESIAN_POINT('Ctrl Pts',(3.12409110440959,1.48740515602026,-5.));
#6316=CARTESIAN_POINT('Ctrl Pts',(3.13994823780237,1.49317013007988,-5.));
#6317=CARTESIAN_POINT('Ctrl Pts',(3.14100520856575,1.49064942821851,-6.5));
#6318=CARTESIAN_POINT('Ctrl Pts',(3.08494727205938,1.47016608894724,-6.5));
#6319=CARTESIAN_POINT('Ctrl Pts',(3.03037988871937,1.44624037846191,-6.5));
#6320=CARTESIAN_POINT('Ctrl Pts',(2.97748590856093,1.41915231489488,-6.5));
#6321=CARTESIAN_POINT('Ctrl Pts',(2.92372703313026,1.39162132118641,-6.5));
#6322=CARTESIAN_POINT('Ctrl Pts',(2.871695963559,1.36082288444892,-6.5));
#6323=CARTESIAN_POINT('Ctrl Pts',(2.82161578916584,1.32700688826385,-6.5));
#6324=CARTESIAN_POINT('Ctrl Pts',(2.77170003062915,1.29330191177955,-6.5));
#6325=CARTESIAN_POINT('Ctrl Pts',(2.72372171689141,1.25659822244747,-6.5));
#6326=CARTESIAN_POINT('Ctrl Pts',(2.67794303793286,1.21711325915177,-6.5));
#6327=CARTESIAN_POINT('Ctrl Pts',(2.6684202947039,1.20889971574195,-6.5));
#6328=CARTESIAN_POINT('Ctrl Pts',(2.65899289462306,1.20056574756288,-6.5));
#6329=CARTESIAN_POINT('Ctrl Pts',(2.64966346414571,1.19211320543645,-6.5));
#6330=CARTESIAN_POINT('Ctrl Pts',(2.64194525774896,1.18512044581758,-6.5));
#6331=CARTESIAN_POINT('Ctrl Pts',(2.63429426375662,1.17804654637327,-6.5));
#6332=CARTESIAN_POINT('Ctrl Pts',(2.62672209878259,1.17090245274249,-6.5));
#6333=CARTESIAN_POINT('Ctrl Pts',(2.58365694565614,1.13027186859452,-6.5));
#6334=CARTESIAN_POINT('Ctrl Pts',(2.54305162503511,1.08729601398087,-6.5));
#6335=CARTESIAN_POINT('Ctrl Pts',(2.50511274754567,1.04221545654921,-6.5));
#6336=CARTESIAN_POINT('Ctrl Pts',(2.46574912979395,0.995441963283155,-6.50000000000001));
#6337=CARTESIAN_POINT('Ctrl Pts',(2.42925494262276,0.946401837425422,-6.5));
#6338=CARTESIAN_POINT('Ctrl Pts',(2.39591368681376,0.89533584763873,-6.5));
#6339=CARTESIAN_POINT('Ctrl Pts',(2.36502342126014,0.84802383292922,-6.5));
#6340=CARTESIAN_POINT('Ctrl Pts',(2.33683964378032,0.798971905014553,-6.50000000000001));
#6341=CARTESIAN_POINT('Ctrl Pts',(2.31163738960224,0.74836188306999,-6.5));
#6342=CARTESIAN_POINT('Ctrl Pts',(2.30963771500258,0.744346227380796,-6.5));
#6343=CARTESIAN_POINT('Ctrl Pts',(2.30765683836007,0.740320761201582,-6.5));
#6344=CARTESIAN_POINT('Ctrl Pts',(2.30569491147364,0.736285575060568,-6.5));
#6345=CARTESIAN_POINT('Ctrl Pts',(2.30080361350804,0.726225415378344,-6.5));
#6346=CARTESIAN_POINT('Ctrl Pts',(2.29603387978872,0.716112511626207,-6.5));
#6347=CARTESIAN_POINT('Ctrl Pts',(2.29139002741425,0.70595426885953,-6.5));
#6348=CARTESIAN_POINT('Ctrl Pts',(2.26822780098137,0.655287817786391,-6.5));
#6349=CARTESIAN_POINT('Ctrl Pts',(2.24817102530427,0.603448830555026,-6.5));
#6350=CARTESIAN_POINT('Ctrl Pts',(2.23143263759802,0.550627378413331,-6.5));
#6351=CARTESIAN_POINT('Ctrl Pts',(2.21963915463869,0.513410598239972,-6.5));
#6352=CARTESIAN_POINT('Ctrl Pts',(2.20949394642941,0.475705703141791,-6.5));
#6353=CARTESIAN_POINT('Ctrl Pts',(2.20108697408611,0.437576967973437,-6.5));
#6354=CARTESIAN_POINT('Ctrl Pts',(2.1891873345697,0.383607692806106,-6.5));
#6355=CARTESIAN_POINT('Ctrl Pts',(2.18076876031134,0.328788238188614,-6.5));
#6356=CARTESIAN_POINT('Ctrl Pts',(2.17577416902111,0.273435929921917,-6.5));
#6357=CARTESIAN_POINT('Ctrl Pts',(2.17434923477101,0.257644167335565,-6.5));
#6358=CARTESIAN_POINT('Ctrl Pts',(2.17320326721325,0.241809120422912,-6.5));
#6359=CARTESIAN_POINT('Ctrl Pts',(2.17233558451626,0.225938418974115,-6.5));
#6360=CARTESIAN_POINT('Ctrl Pts',(2.17166526676672,0.213677700953913,-6.5));
#6361=CARTESIAN_POINT('Ctrl Pts',(2.17116110529721,0.201393005178454,-6.5));
#6362=CARTESIAN_POINT('Ctrl Pts',(2.17082312577695,0.189111602497678,-6.5));
#6363=CARTESIAN_POINT('Ctrl Pts',(2.16929543448595,0.133598795384436,-6.5));
#6364=CARTESIAN_POINT('Ctrl Pts',(2.17115162578008,0.0780521664174741,-6.5));
#6365=CARTESIAN_POINT('Ctrl Pts',(2.17628380677392,0.0227871693634732,-6.5));
#6366=CARTESIAN_POINT('Ctrl Pts',(2.18141533505767,-0.0324707990956518,
-6.5));
#6367=CARTESIAN_POINT('Ctrl Pts',(2.18982247496828,-0.0874483413955667,
-6.5));
#6368=CARTESIAN_POINT('Ctrl Pts',(2.20144629520756,-0.141815029635975,-6.5));
#6369=CARTESIAN_POINT('Ctrl Pts',(2.20865289933067,-0.175521607298768,-6.5));
#6370=CARTESIAN_POINT('Ctrl Pts',(2.21709687600562,-0.208993018190762,-6.5));
#6371=CARTESIAN_POINT('Ctrl Pts',(2.22677248421428,-0.24214473226519,-6.5));
#6372=CARTESIAN_POINT('Ctrl Pts',(2.23175694861537,-0.259223094170246,-6.5));
#6373=CARTESIAN_POINT('Ctrl Pts',(2.23706837039207,-0.276216526665636,-6.5));
#6374=CARTESIAN_POINT('Ctrl Pts',(2.24270655913964,-0.293112851925979,-6.5));
#6375=CARTESIAN_POINT('Ctrl Pts',(2.24692178219473,-0.305744883766785,-6.5));
#6376=CARTESIAN_POINT('Ctrl Pts',(2.25132049507297,-0.318324481904199,-6.5));
#6377=CARTESIAN_POINT('Ctrl Pts',(2.25589478335012,-0.330825919503712,-6.5));
#6378=CARTESIAN_POINT('Ctrl Pts',(2.2743421029172,-0.381242071803956,-6.5));
#6379=CARTESIAN_POINT('Ctrl Pts',(2.29566569186883,-0.4304646756,-6.5));
#6380=CARTESIAN_POINT('Ctrl Pts',(2.31982030634388,-0.478178835899828,-6.5));
#6381=CARTESIAN_POINT('Ctrl Pts',(2.3360728938977,-0.510283615242568,-6.5));
#6382=CARTESIAN_POINT('Ctrl Pts',(2.35360804649871,-0.541704938378982,-6.5));
#6383=CARTESIAN_POINT('Ctrl Pts',(2.3724212135575,-0.572337190454871,-6.5));
#6384=CARTESIAN_POINT('Ctrl Pts',(2.3809158305163,-0.58616842084565,-6.49999999999999));
#6385=CARTESIAN_POINT('Ctrl Pts',(2.38967347678636,-0.599841872207131,-6.5));
#6386=CARTESIAN_POINT('Ctrl Pts',(2.39867859342135,-0.613324895247866,-6.5));
#6387=CARTESIAN_POINT('Ctrl Pts',(2.42713371190609,-0.655929675808517,-6.5));
#6388=CARTESIAN_POINT('Ctrl Pts',(2.45808277339633,-0.696680211491728,-6.49999999999999));
#6389=CARTESIAN_POINT('Ctrl Pts',(2.49150132174337,-0.735275360483379,-6.5));
#6390=CARTESIAN_POINT('Ctrl Pts',(2.51006349039157,-0.756712846550875,-6.5));
#6391=CARTESIAN_POINT('Ctrl Pts',(2.5293881120533,-0.77748468706277,-6.5));
#6392=CARTESIAN_POINT('Ctrl Pts',(2.54947484834281,-0.797533396503153,-6.5));
#6393=CARTESIAN_POINT('Ctrl Pts',(2.55933167690434,-0.807371564784229,-6.5));
#6394=CARTESIAN_POINT('Ctrl Pts',(2.56937206717339,-0.817035528308793,-6.5));
#6395=CARTESIAN_POINT('Ctrl Pts',(2.579590276763,-0.826522883252263,-6.5));
#6396=CARTESIAN_POINT('Origin',(3.53951905042299,5.55111512312578E-16,-6.5));
#6397=CARTESIAN_POINT('',(2.38481851204374,2.,-6.5));
#6398=CARTESIAN_POINT('',(4.69421958880225,2.,-6.5));
#6399=CARTESIAN_POINT('',(2.38481851204374,2.,-6.5));
#6400=CARTESIAN_POINT('',(5.8489201271815,1.94289029309402E-15,-6.5));
#6401=CARTESIAN_POINT('',(4.69421958880225,2.,-6.5));
#6402=CARTESIAN_POINT('',(4.69421958880225,-2.,-6.5));
#6403=CARTESIAN_POINT('',(5.8489201271815,1.94289029309402E-15,-6.5));
#6404=CARTESIAN_POINT('',(2.38481851204374,-2.,-6.5));
#6405=CARTESIAN_POINT('',(4.69421958880225,-2.,-6.5));
#6406=CARTESIAN_POINT('',(1.23011797366449,-1.2490009027033E-15,-6.5));
#6407=CARTESIAN_POINT('',(2.38481851204374,-2.,-6.5));
#6408=CARTESIAN_POINT('',(1.23011797366449,-1.2490009027033E-15,-6.5));
#6409=CARTESIAN_POINT('Origin',(5.8489201271815,1.94289029309402E-15,-6.5));
#6410=CARTESIAN_POINT('',(4.69421958880225,2.,-5.));
#6411=CARTESIAN_POINT('',(4.69421958880225,2.,-6.5));
#6412=CARTESIAN_POINT('',(5.8489201271815,1.94289029309402E-15,-5.));
#6413=CARTESIAN_POINT('',(4.69421958880225,2.,-5.));
#6414=CARTESIAN_POINT('',(5.8489201271815,1.94289029309402E-15,-6.5));
#6415=CARTESIAN_POINT('Origin',(4.69421958880225,-2.,-6.5));
#6416=CARTESIAN_POINT('',(4.69421958880225,-2.,-5.));
#6417=CARTESIAN_POINT('',(5.8489201271815,1.94289029309402E-15,-5.));
#6418=CARTESIAN_POINT('',(4.69421958880225,-2.,-6.5));
#6419=CARTESIAN_POINT('Origin',(2.38481851204374,-2.,-6.5));
#6420=CARTESIAN_POINT('',(2.38481851204374,-2.,-5.));
#6421=CARTESIAN_POINT('',(4.69421958880225,-2.,-5.));
#6422=CARTESIAN_POINT('',(2.38481851204374,-2.,-6.5));
#6423=CARTESIAN_POINT('Origin',(1.23011797366449,-1.38777878078145E-15,
-6.5));
#6424=CARTESIAN_POINT('',(1.23011797366449,-1.2490009027033E-15,-5.));
#6425=CARTESIAN_POINT('',(2.38481851204374,-2.,-5.));
#6426=CARTESIAN_POINT('',(1.23011797366449,-1.2490009027033E-15,-6.5));
#6427=CARTESIAN_POINT('Origin',(2.38481851204374,2.,-6.5));
#6428=CARTESIAN_POINT('',(2.38481851204374,2.,-5.));
#6429=CARTESIAN_POINT('',(1.23011797366449,-1.2490009027033E-15,-5.));
#6430=CARTESIAN_POINT('',(2.38481851204374,2.,-6.5));
#6431=CARTESIAN_POINT('Origin',(4.69421958880225,2.,-6.5));
#6432=CARTESIAN_POINT('',(2.38481851204374,2.,-5.));
#6433=CARTESIAN_POINT('Origin',(3.53951905042299,5.55111512312578E-16,-5.));
#6434=CARTESIAN_POINT('',(0.,0.,0.));
#6435=CARTESIAN_POINT('Origin',(85.6487002358236,0.,-8.24265256448471E-15));
#6436=CARTESIAN_POINT('',(85.6487002358236,1.08063175605657,-8.37499178659588E-15));
#6437=CARTESIAN_POINT('Origin',(85.6487002358236,0.,-8.24265256448471E-15));
#6438=CARTESIAN_POINT('',(89.1487002358236,1.08063175605657,-8.37499178659588E-15));
#6439=CARTESIAN_POINT('',(85.6487002358236,1.08063175605657,-8.11031334237355E-15));
#6440=CARTESIAN_POINT('Origin',(89.1487002358236,0.,-8.24265256448471E-15));
#6441=CARTESIAN_POINT('Origin',(89.1487002358236,0.,-8.18789480661053E-15));
#6442=CARTESIAN_POINT('Origin',(86.6487002358236,-4.60471880688602E-46,
1.0611405339408E-14));
#6443=CARTESIAN_POINT('',(85.6487002358236,1.42213764307597E-16,-1.16126351211313));
#6444=CARTESIAN_POINT('Origin',(85.6487002358236,-4.60471880688602E-46,
1.04889406594932E-14));
#6445=CARTESIAN_POINT('',(86.6487002358236,-2.64678444222332E-16,-2.16126351211313));
#6446=CARTESIAN_POINT('Origin',(86.6487002358236,-1.42213764307597E-16,
-1.16126351211313));
#6447=CARTESIAN_POINT('',(86.6487002358236,5.29356888444664E-16,2.16126351211315));
#6448=CARTESIAN_POINT('Origin',(86.6487002358236,-4.60471880688602E-46,
1.0611405339408E-14));
#6449=CARTESIAN_POINT('Origin',(86.6487002358236,-4.60471880688602E-46,
1.0611405339408E-14));
#6450=CARTESIAN_POINT('Origin',(85.6487002358236,-2.18952885050753E-46,
1.04889406594933E-14));
#6451=CARTESIAN_POINT('Origin',(89.6530615045687,-4.60471880688602E-46,
1.09793334805331E-14));
#6452=CARTESIAN_POINT('',(93.6574227733139,5.29356888444664E-16,2.16126351211315));
#6453=CARTESIAN_POINT('',(89.6530615045687,5.29356888444664E-16,2.16126351211315));
#6454=CARTESIAN_POINT('',(93.6574227733139,-2.16126351211314,1.19990831900176E-14));
#6455=CARTESIAN_POINT('Origin',(93.6574227733139,-2.18952885050753E-46,
1.14697263015729E-14));
#6456=CARTESIAN_POINT('Origin',(93.6574227733139,-2.18952885050753E-46,
1.14697263015729E-14));
#6457=CARTESIAN_POINT('Origin',(96.460480949577,-8.32667268468867E-16,1.18130019239114E-14));
#6458=CARTESIAN_POINT('',(98.960480949577,-5.26505568682029E-16,1.21191636236982E-14));
#6459=CARTESIAN_POINT('Origin',(96.460480949577,-8.32667268468867E-16,1.18130019239114E-14));
#6460=CARTESIAN_POINT('',(98.960480949577,-8.33357072363267E-16,-2.50563267625309));
#6461=CARTESIAN_POINT('',(98.960480949577,-1.13882896825571E-15,1.21191636236982E-14));
#6462=CARTESIAN_POINT('Origin',(96.460480949577,-1.13951877215011E-15,-2.50563267625309));
#6463=CARTESIAN_POINT('Origin',(96.460480949577,-6.93889390390723E-16,1.18130019239114E-14));
#6464=CARTESIAN_POINT('Origin',(96.460480949577,-2.18952885050753E-46,1.18130019239114E-14));
#6465=CARTESIAN_POINT('',(100.,-2.1673303378108E-16,1.22464679914736E-14));
#6466=CARTESIAN_POINT('Origin',(96.460480949577,-2.18952885050753E-46,1.18130019239114E-14));
#6467=CARTESIAN_POINT('',(0.,0.,0.));
#6468=CARTESIAN_POINT('Origin',(85.6487002358236,0.,-8.18789480661053E-15));
#6469=CARTESIAN_POINT('',(85.6487002358236,-1.32339222111166E-16,1.08063175605657));
#6470=CARTESIAN_POINT('Origin',(85.6487002358236,0.,0.));
#6471=CARTESIAN_POINT('Origin',(78.2297384009075,0.,0.));
#6472=CARTESIAN_POINT('',(67.3063659679149,-1.32339222111166E-16,1.08063175605657));
#6473=CARTESIAN_POINT('',(78.2297384009075,-1.32339222111166E-16,1.08063175605657));
#6474=CARTESIAN_POINT('Origin',(67.3063659679149,0.,0.));
#6475=CARTESIAN_POINT('Origin',(67.3063659679149,0.,-1.08063175605657));
#6476=CARTESIAN_POINT('Origin',(89.1531108339,0.,0.));
#6477=CARTESIAN_POINT('',(89.1531108339,-1.32339222111166E-16,1.08063175605657));
#6478=CARTESIAN_POINT('Origin',(89.1531108339,0.,0.));
#6479=CARTESIAN_POINT('Origin',(78.2297384009075,0.,0.));
#6480=CARTESIAN_POINT('',(89.1487002358236,-1.32339222111166E-16,1.08063175605657));
#6481=CARTESIAN_POINT('',(78.2297384009075,-1.32339222111166E-16,1.08063175605657));
#6482=CARTESIAN_POINT('Origin',(89.1487002358236,0.,0.));
#6483=CARTESIAN_POINT('Origin',(89.1487002358236,0.,-8.18789480661053E-15));
#6484=CARTESIAN_POINT('',(0.,0.,0.));
#6485=CARTESIAN_POINT('Origin',(3.53951905042299,8.32667268468867E-16,0.924367114736157));
#6486=CARTESIAN_POINT('',(4.07816931076926,-1.04735426648718,-0.262501355395651));
#6487=CARTESIAN_POINT('',(4.07816926754758,-1.04735428871592,-0.162850680997093));
#6488=CARTESIAN_POINT('',(4.07816926754759,-1.04735428871592,0.924367114736157));
#6489=CARTESIAN_POINT('',(2.86617836717395,0.966285354738297,1.30764946397119E-15));
#6490=CARTESIAN_POINT('Ctrl Pts',(4.07816931076926,-1.04735426648718,-0.262501355395651));
#6491=CARTESIAN_POINT('Ctrl Pts',(4.13816550929519,-1.01649845294839,-0.257760959449959));
#6492=CARTESIAN_POINT('Ctrl Pts',(4.19540688115252,-0.980540763988985,-0.252855425799963));
#6493=CARTESIAN_POINT('Ctrl Pts',(4.30612909358366,-0.896929430168507,-0.242678032345055));
#6494=CARTESIAN_POINT('Ctrl Pts',(4.35898806098992,-0.848908539803626,-0.237423776835087));
#6495=CARTESIAN_POINT('Ctrl Pts',(4.41381673949112,-0.789173500392151,-0.231741146856556));
#6496=CARTESIAN_POINT('Ctrl Pts',(4.4203588187141,-0.781864809957386,-0.231059038775153));
#6497=CARTESIAN_POINT('Ctrl Pts',(4.42936456010577,-0.771547233408173,-0.230115323768185));
#6498=CARTESIAN_POINT('Ctrl Pts',(4.43190557214461,-0.768606831483667,-0.229848510688452));
#6499=CARTESIAN_POINT('Ctrl Pts',(4.43628102834384,-0.7634927025417,-0.22938821683561));
#6500=CARTESIAN_POINT('Ctrl Pts',(4.43812221904588,-0.76132483058054,-0.22919425806598));
#6501=CARTESIAN_POINT('Ctrl Pts',(4.4419940328539,-0.756732429561088,-0.228785856907052));
#6502=CARTESIAN_POINT('Ctrl Pts',(4.44402276326807,-0.754306368515252,-0.228571560869313));
#6503=CARTESIAN_POINT('Ctrl Pts',(4.44906391192553,-0.748228319777068,-0.228038218896995));
#6504=CARTESIAN_POINT('Ctrl Pts',(4.45206417443405,-0.744566230880235,-0.227720036311731));
#6505=CARTESIAN_POINT('Ctrl Pts',(4.4635118607649,-0.730420164685874,-0.226502596978593));
#6506=CARTESIAN_POINT('Ctrl Pts',(4.47180174820231,-0.719809238841447,-0.225613787694774));
#6507=CARTESIAN_POINT('Ctrl Pts',(4.49281897725252,-0.691935104910647,-0.2233344621005));
#6508=CARTESIAN_POINT('Ctrl Pts',(4.50526041034554,-0.674461769680659,-0.221959206687815));
#6509=CARTESIAN_POINT('Ctrl Pts',(4.54393811714973,-0.616874402055789,-0.217562693758889));
#6510=CARTESIAN_POINT('Ctrl Pts',(4.56820618750021,-0.575495412961658,-0.214608207433024));
#6511=CARTESIAN_POINT('Ctrl Pts',(4.62526109382569,-0.46300640102283,-0.206815767260325));
#6512=CARTESIAN_POINT('Ctrl Pts',(4.65359724115015,-0.389921160068868,-0.201974641152135));
#6513=CARTESIAN_POINT('Ctrl Pts',(4.67862153917193,-0.299634523535007,-0.195871749338333));
#6514=CARTESIAN_POINT('Ctrl Pts',(4.68246619326538,-0.284617496968038,-0.194853457399708));
#6515=CARTESIAN_POINT('Ctrl Pts',(4.68762666705435,-0.262666457670646,-0.193358256177876));
#6516=CARTESIAN_POINT('Ctrl Pts',(4.68917841867376,-0.255789172372448,-0.192888861792896));
#6517=CARTESIAN_POINT('Ctrl Pts',(4.69181882450146,-0.243577362041553,-0.192053506347722));
#6518=CARTESIAN_POINT('Ctrl Pts',(4.69293241996632,-0.238248395356479,-0.191688349687422));
#6519=CARTESIAN_POINT('Ctrl Pts',(4.69517493593701,-0.227132770342401,-0.190925282428703));
#6520=CARTESIAN_POINT('Ctrl Pts',(4.69629742865534,-0.22134498536421,-0.190527179087801));
#6521=CARTESIAN_POINT('Ctrl Pts',(4.6991075394683,-0.206250014609,-0.189486738128586));
#6522=CARTESIAN_POINT('Ctrl Pts',(4.70072654364688,-0.196930650270888,-0.188842255840524));
#6523=CARTESIAN_POINT('Ctrl Pts',(4.70755352597748,-0.154616561061837,-0.185905682610639));
#6524=CARTESIAN_POINT('Ctrl Pts',(4.71146816972925,-0.121431845216441,-0.183573664947217));
#6525=CARTESIAN_POINT('Ctrl Pts',(4.7222007063528,0.0215960176556974,-0.173392427299512));
#6526=CARTESIAN_POINT('Ctrl Pts',(4.7150171499791,0.131911029667048,-0.165146131316402));
#6527=CARTESIAN_POINT('Ctrl Pts',(4.68764035004445,0.263657969696757,-0.155483063352771));
#6528=CARTESIAN_POINT('Ctrl Pts',(4.6818933217096,0.287540033878893,-0.153742465559107));
#6529=CARTESIAN_POINT('Ctrl Pts',(4.67381354591698,0.31702878431748,-0.151620868600707));
#6530=CARTESIAN_POINT('Ctrl Pts',(4.67217935970378,0.322818649137025,-0.151205659590905));
#6531=CARTESIAN_POINT('Ctrl Pts',(4.66952958748343,0.331938800090816,-0.150554031777303));
#6532=CARTESIAN_POINT('Ctrl Pts',(4.6685435046414,0.335277442496423,-0.150315999857958));
#6533=CARTESIAN_POINT('Ctrl Pts',(4.66675225279319,0.34124467336953,-0.149891537487618));
#6534=CARTESIAN_POINT('Ctrl Pts',(4.66595268757235,0.343874804090377,-0.149704797040631));
#6535=CARTESIAN_POINT('Ctrl Pts',(4.66400429706283,0.350204220881102,-0.149256203118779));
#6536=CARTESIAN_POINT('Ctrl Pts',(4.6628464201863,0.353900674827748,-0.148994873079714));
#6537=CARTESIAN_POINT('Ctrl Pts',(4.65924128714954,0.365213878672216,-0.148196873893526));
#6538=CARTESIAN_POINT('Ctrl Pts',(4.65673458250859,0.37281165228385,-0.147663480767335));
#6539=CARTESIAN_POINT('Ctrl Pts',(4.65070235991253,0.3904877728462,-0.146427187882288));
#6540=CARTESIAN_POINT('Ctrl Pts',(4.64711678380012,0.400545036969767,-0.145727318775054));
#6541=CARTESIAN_POINT('Ctrl Pts',(4.6339872215201,0.435847231618147,-0.143278675086443));
#6542=CARTESIAN_POINT('Ctrl Pts',(4.62371233511675,0.460812876058328,-0.141561441921139));
#6543=CARTESIAN_POINT('Ctrl Pts',(4.57996758790865,0.557517959585241,-0.134886761353886));
#6544=CARTESIAN_POINT('Ctrl Pts',(4.54016092197969,0.626159728430909,-0.130084903250573));
#6545=CARTESIAN_POINT('Ctrl Pts',(4.46659256838585,0.727859655020217,-0.122197192651481));
#6546=CARTESIAN_POINT('Ctrl Pts',(4.43722437578685,0.763786207839597,-0.119234669369417));
#6547=CARTESIAN_POINT('Ctrl Pts',(4.39853048789781,0.805797813695031,-0.115480076350559));
#6548=CARTESIAN_POINT('Ctrl Pts',(4.39113543028509,0.813609424325328,-0.11476870308578));
#6549=CARTESIAN_POINT('Ctrl Pts',(4.37924973285856,0.825825029854022,-0.113634342328986));
#6550=CARTESIAN_POINT('Ctrl Pts',(4.3748289102129,0.830296353430724,-0.11321433654788));
#6551=CARTESIAN_POINT('Ctrl Pts',(4.3665082443372,0.83857835839877,-0.112427231231687));
#6552=CARTESIAN_POINT('Ctrl Pts',(4.36261731559497,0.842397788573141,-0.11206052573141));
#6553=CARTESIAN_POINT('Ctrl Pts',(4.35387656196646,0.850859551665857,-0.111239670772204));
#6554=CARTESIAN_POINT('Ctrl Pts',(4.34901331199061,0.855487679951562,-0.110784933099378));
#6555=CARTESIAN_POINT('Ctrl Pts',(4.33455613023088,0.869012250190631,-0.109438706396591));
#6556=CARTESIAN_POINT('Ctrl Pts',(4.32485347967524,0.877790441808004,-0.108542344696331));
#6557=CARTESIAN_POINT('Ctrl Pts',(4.26077881466586,0.93384736061385,-0.102666467791259));
#6558=CARTESIAN_POINT('Ctrl Pts',(4.20232102972743,0.97620529648228,-0.0974916761104508));
#6559=CARTESIAN_POINT('Ctrl Pts',(4.07211685570001,1.05343834723275,-0.0864287426029128));
#6560=CARTESIAN_POINT('Ctrl Pts',(3.99994258612451,1.08692428653761,-0.0805489349057646));
#6561=CARTESIAN_POINT('Ctrl Pts',(3.91355719641518,1.11684187728582,-0.0741140552653006));
#6562=CARTESIAN_POINT('Ctrl Pts',(3.90210839820426,1.12061113066185,-0.0732731940006031));
#6563=CARTESIAN_POINT('Ctrl Pts',(3.88615710198964,1.12559265263226,-0.0721199958198652));
#6564=CARTESIAN_POINT('Ctrl Pts',(3.88170268793243,1.12695479877715,-0.0717999317519526));
#6565=CARTESIAN_POINT('Ctrl Pts',(3.87421306498854,1.12919660102562,-0.0712652072392914));
#6566=CARTESIAN_POINT('Ctrl Pts',(3.87118223068805,1.13009051981056,-0.0710497608330243));
#6567=CARTESIAN_POINT('Ctrl Pts',(3.86502742030902,1.13187893437307,-0.0706141865561824));
#6568=CARTESIAN_POINT('Ctrl Pts',(3.86190331726675,1.13277270715122,-0.0703940957941245));
#6569=CARTESIAN_POINT('Ctrl Pts',(3.85395803619936,1.13501023579287,-0.0698368025066016));
#6570=CARTESIAN_POINT('Ctrl Pts',(3.84913186046174,1.13633622716197,-0.0695005691621308));
#6571=CARTESIAN_POINT('Ctrl Pts',(3.83011999513144,1.14142961887213,-0.0681844603270428));
#6572=CARTESIAN_POINT('Ctrl Pts',(3.81587217898588,1.14496265396246,-0.0672165297757819));
#6573=CARTESIAN_POINT('Ctrl Pts',(3.77811043176378,1.15358042621109,-0.0646904738735653));
#6574=CARTESIAN_POINT('Ctrl Pts',(3.75449964641512,1.15821290470527,-0.0631508132919473));
#6575=CARTESIAN_POINT('Ctrl Pts',(3.67970544957271,1.1705213458426,-0.0583521744794719));
#6576=CARTESIAN_POINT('Ctrl Pts',(3.62814852508006,1.17554995615846,-0.0551573055353008));
#6577=CARTESIAN_POINT('Ctrl Pts',(3.50563494505662,1.17939105836018,-0.0475283777116149));
#6578=CARTESIAN_POINT('Ctrl Pts',(3.43479699254525,1.17522033949375,-0.0430809171857789));
#6579=CARTESIAN_POINT('Ctrl Pts',(3.35444620471573,1.16316466451054,-0.0377452881286854));
#6580=CARTESIAN_POINT('Ctrl Pts',(3.34414597583988,1.16147894757009,-0.0370559974738152));
#6581=CARTESIAN_POINT('Ctrl Pts',(3.32717257087031,1.15846894566891,-0.0359106524132708));
#6582=CARTESIAN_POINT('Ctrl Pts',(3.32048590746682,1.15722331663216,-0.0354570009017416));
#6583=CARTESIAN_POINT('Ctrl Pts',(3.30838947893792,1.15486133015112,-0.034631714068847));
#6584=CARTESIAN_POINT('Ctrl Pts',(3.30297602833448,1.15376469336405,-0.0342606960157208));
#6585=CARTESIAN_POINT('Ctrl Pts',(3.29133535025683,1.15132119951867,-0.0334591600867042));
#6586=CARTESIAN_POINT('Ctrl Pts',(3.28511096165394,1.14996181464974,-0.0330282645783143));
#6587=CARTESIAN_POINT('Ctrl Pts',(3.26797624459067,1.14607372973679,-0.0318355405930534));
#6588=CARTESIAN_POINT('Ctrl Pts',(3.25709071863468,1.14343985937194,-0.0310704672878365));
#6589=CARTESIAN_POINT('Ctrl Pts',(3.18929186352776,1.12600800713029,-0.0262576732137973));
#6590=CARTESIAN_POINT('Ctrl Pts',(3.13352468638961,1.10712229042616,-0.0220817387791934));
#6591=CARTESIAN_POINT('Ctrl Pts',(3.00443184308116,1.0523357870937,-0.0119100216368716));
#6592=CARTESIAN_POINT('Ctrl Pts',(2.93297576091339,1.01283206324342,-0.00585245073367892));
#6593=CARTESIAN_POINT('Ctrl Pts',(2.86617836717395,0.966285354738297,1.30764946397119E-15));
#6594=CARTESIAN_POINT('',(4.22418347496246,0.958295198918397,0.));
#6595=CARTESIAN_POINT('Origin',(3.53951905042299,8.32667268468867E-16,0.));
#6596=CARTESIAN_POINT('Ctrl Pts',(4.22418347496246,0.958295198918393,4.44089209850063E-16));
#6597=CARTESIAN_POINT('Ctrl Pts',(4.26382260582939,0.92997459086893,-0.00329165982698132));
#6598=CARTESIAN_POINT('Ctrl Pts',(4.30173542240052,0.89916685852182,-0.00658331965396309));
#6599=CARTESIAN_POINT('Ctrl Pts',(4.33761006999466,0.86610956984613,-0.00987497948094485));
#6600=CARTESIAN_POINT('Ctrl Pts',(4.37303430005125,0.833467325876437,-0.0131253114785776));
#6601=CARTESIAN_POINT('Ctrl Pts',(4.40647088077483,0.79863207783641,-0.0163756434762103));
#6602=CARTESIAN_POINT('Ctrl Pts',(4.43765337026355,0.76187256547571,-0.019625975473843));
#6603=CARTESIAN_POINT('Ctrl Pts',(4.4688290359802,0.725121097326283,-0.022875596190079));
#6604=CARTESIAN_POINT('Ctrl Pts',(4.49775125328327,0.686446597209151,-0.0261252169063152));
#6605=CARTESIAN_POINT('Ctrl Pts',(4.52419296687062,0.646151948668183,-0.0293748376225512));
#6606=CARTESIAN_POINT('Ctrl Pts',(4.5506380448392,0.60585217313124,-0.0326248718128573));
#6607=CARTESIAN_POINT('Ctrl Pts',(4.57460170861404,0.563932275665533,-0.0358749060031633));
#6608=CARTESIAN_POINT('Ctrl Pts',(4.59590072517422,0.520723362016513,-0.0391249401934693));
#6609=CARTESIAN_POINT('Ctrl Pts',(4.61767731820734,0.476545597973794,-0.0424478481646437));
#6610=CARTESIAN_POINT('Ctrl Pts',(4.63666802073486,0.431020796741864,-0.0457707561358183));
#6611=CARTESIAN_POINT('Ctrl Pts',(4.65272839029913,0.384525718401926,-0.0490936641069927));
#6612=CARTESIAN_POINT('Ctrl Pts',(4.66846915279708,0.338955908657327,-0.05235044502772));
#6613=CARTESIAN_POINT('Ctrl Pts',(4.68139509545731,0.292454626199629,-0.0556072259484471));
#6614=CARTESIAN_POINT('Ctrl Pts',(4.69142118679469,0.245390567712603,-0.0588640068691744));
#6615=CARTESIAN_POINT('Ctrl Pts',(4.70175263909914,0.196893096549577,-0.0622199783655723));
#6616=CARTESIAN_POINT('Ctrl Pts',(4.70900458391102,0.147798590244708,-0.0655759498619703));
#6617=CARTESIAN_POINT('Ctrl Pts',(4.71314140620248,0.098517148327605,-0.0689319213583682));
#6618=CARTESIAN_POINT('Ctrl Pts',(4.71727822849394,0.0492357064105011,-0.0722878928547662));
#6619=CARTESIAN_POINT('Ctrl Pts',(4.71829998113881,-0.000232073325149317,
-0.075643864351164));
#6620=CARTESIAN_POINT('Ctrl Pts',(4.71622928026619,-0.0494782526203934,
-0.078999835847562));
#6621=CARTESIAN_POINT('Ctrl Pts',(4.71419826096718,-0.0977807099542783,
-0.0822914956745437));
#6622=CARTESIAN_POINT('Ctrl Pts',(4.70918221066814,-0.146094497186642,-0.0855831555015257));
#6623=CARTESIAN_POINT('Ctrl Pts',(4.70117871293859,-0.194015182354719,-0.0888748153285074));
#6624=CARTESIAN_POINT('Ctrl Pts',(4.69354694837555,-0.23971012714772,-0.0920135896082097));
#6625=CARTESIAN_POINT('Ctrl Pts',(4.68319921317479,-0.285047032934924,-0.095152363887912));
#6626=CARTESIAN_POINT('Ctrl Pts',(4.67018650263742,-0.329675863543162,-0.0982911381676143));
#6627=CARTESIAN_POINT('Ctrl Pts',(4.65718861687458,-0.374253850605062,-0.101426336588094));
#6628=CARTESIAN_POINT('Ctrl Pts',(4.641531917044,-0.418124812744379,-0.104561535008573));
#6629=CARTESIAN_POINT('Ctrl Pts',(4.6233183718038,-0.460949122435977,-0.107696733429053));
#6630=CARTESIAN_POINT('Ctrl Pts',(4.60511713162024,-0.503744500058096,-0.11082981371198));
#6631=CARTESIAN_POINT('Ctrl Pts',(4.5843626867868,-0.545494100397139,-0.113962893994906));
#6632=CARTESIAN_POINT('Ctrl Pts',(4.56120581261628,-0.585876456651907,-0.117095974277833));
#6633=CARTESIAN_POINT('Ctrl Pts',(4.53805384812113,-0.62625025111813,-0.120228390291179));
#6634=CARTESIAN_POINT('Ctrl Pts',(4.51250074913838,-0.665256882154561,-0.123360806304525));
#6635=CARTESIAN_POINT('Ctrl Pts',(4.4847427284623,-0.702600356514171,-0.12649322231787));
#6636=CARTESIAN_POINT('Ctrl Pts',(4.45695818213,-0.739979516421182,-0.129628631678301));
#6637=CARTESIAN_POINT('Ctrl Pts',(4.42696485136167,-0.77569188988454,-0.132764041038732));
#6638=CARTESIAN_POINT('Ctrl Pts',(4.39500041587223,-0.8094730976809,-0.135899450399163));
#6639=CARTESIAN_POINT('Ctrl Pts',(4.36301801761838,-0.843273289196747,-0.139036621737203));
#6640=CARTESIAN_POINT('Ctrl Pts',(4.32906272850112,-0.87513976659434,-0.142173793075244));
#6641=CARTESIAN_POINT('Ctrl Pts',(4.29340766366195,-0.904846407590057,-0.145310964413285));
#6642=CARTESIAN_POINT('Ctrl Pts',(4.25768672285757,-0.934607934298585,-0.148453931959828));
#6643=CARTESIAN_POINT('Ctrl Pts',(4.22026020429182,-0.962201331231541,-0.15159689950637));
#6644=CARTESIAN_POINT('Ctrl Pts',(4.18143101926719,-0.987443206850178,-0.154739867052913));
#6645=CARTESIAN_POINT('Ctrl Pts',(4.16800681048762,-0.996169947009094,-0.155826468600317));
#6646=CARTESIAN_POINT('Ctrl Pts',(4.15441516069387,-1.00461602573018,-0.15691307014772));
#6647=CARTESIAN_POINT('Ctrl Pts',(4.14066920303589,-1.01277517569966,-0.157999671695124));
#6648=CARTESIAN_POINT('Ctrl Pts',(4.12021344700688,-1.02491704208196,-0.15961667479578));
#6649=CARTESIAN_POINT('Ctrl Pts',(4.09936714904988,-1.03645230111076,-0.161233677896437));
#6650=CARTESIAN_POINT('Ctrl Pts',(4.07816926754758,-1.04735428871592,-0.162850680997093));
#6651=CARTESIAN_POINT('Origin',(3.53951905042299,8.32667268468867E-16,0.924367114736157));
#6652=CARTESIAN_POINT('',(4.07816931162903,-1.047354266045,-0.76175719316035));
#6653=CARTESIAN_POINT('',(4.0781692670594,-1.04735428896699,-0.661995228290505));
#6654=CARTESIAN_POINT('',(4.07816926754759,-1.04735428871592,0.924367114736157));
#6655=CARTESIAN_POINT('Ctrl Pts',(4.07816931162903,-1.047354266045,-0.76175719316035));
#6656=CARTESIAN_POINT('Ctrl Pts',(4.11408449771752,-1.028883224302,-0.75925178827356));
#6657=CARTESIAN_POINT('Ctrl Pts',(4.14903578684085,-1.00857194726112,-0.756728985411424));
#6658=CARTESIAN_POINT('Ctrl Pts',(4.2007960181172,-0.974815447192962,-0.752791344928083));
#6659=CARTESIAN_POINT('Ctrl Pts',(4.21838604571316,-0.962648380607407,-0.751415312608433));
#6660=CARTESIAN_POINT('Ctrl Pts',(4.24838438327225,-0.940667235500158,-0.748993071487715));
#6661=CARTESIAN_POINT('Ctrl Pts',(4.26094451012015,-0.931069372113161,-0.747954718235958));
#6662=CARTESIAN_POINT('Ctrl Pts',(4.27894960649694,-0.916727631974777,-0.746428293310126));
#6663=CARTESIAN_POINT('Ctrl Pts',(4.28455047789923,-0.912181597427246,-0.745947959461167));
#6664=CARTESIAN_POINT('Ctrl Pts',(4.29433453304305,-0.904089992843911,-0.745098905772204));
#6665=CARTESIAN_POINT('Ctrl Pts',(4.29853541639712,-0.900566089975633,-0.744731059244522));
#6666=CARTESIAN_POINT('Ctrl Pts',(4.30723995822577,-0.893160132434266,-0.743961850541347));
#6667=CARTESIAN_POINT('Ctrl Pts',(4.3117391222387,-0.889273058682218,-0.743560290905421));
#6668=CARTESIAN_POINT('Ctrl Pts',(4.32339363388339,-0.879048949164388,-0.742509544390645));
#6669=CARTESIAN_POINT('Ctrl Pts',(4.33050149084711,-0.872658688850285,-0.741858179270333));
#6670=CARTESIAN_POINT('Ctrl Pts',(4.36008715374033,-0.845401507957279,-0.739101460142049));
#6671=CARTESIAN_POINT('Ctrl Pts',(4.38182137522774,-0.823748880257132,-0.736963353839677));
#6672=CARTESIAN_POINT('Ctrl Pts',(4.47365648348548,-0.72482038699092,-0.727406996775484));
#6673=CARTESIAN_POINT('Ctrl Pts',(4.5341517001094,-0.639278883383134,-0.719627547302095));
#6674=CARTESIAN_POINT('Ctrl Pts',(4.59269268464872,-0.527630994946312,-0.710508477288347));
#6675=CARTESIAN_POINT('Ctrl Pts',(4.60226786336298,-0.508069135975042,-0.708947669468941));
#6676=CARTESIAN_POINT('Ctrl Pts',(4.61694606614582,-0.475848566393389,-0.706447942174642));
#6677=CARTESIAN_POINT('Ctrl Pts',(4.6223810304526,-0.463347390777703,-0.705495008183453));
#6678=CARTESIAN_POINT('Ctrl Pts',(4.62942754962777,-0.44633773829989,-0.704223722673499));
#6679=CARTESIAN_POINT('Ctrl Pts',(4.6312302042334,-0.441910253211254,-0.703895105860567));
#6680=CARTESIAN_POINT('Ctrl Pts',(4.63419017831379,-0.434511621910368,-0.703349915704065));
#6681=CARTESIAN_POINT('Ctrl Pts',(4.63536246155079,-0.431546575476847,-0.70313247922492));
#6682=CARTESIAN_POINT('Ctrl Pts',(4.63755726769565,-0.425928654410585,-0.702722534290551));
#6683=CARTESIAN_POINT('Ctrl Pts',(4.63858224762229,-0.42327678206877,-0.702529877765054));
#6684=CARTESIAN_POINT('Ctrl Pts',(4.64098460495769,-0.416993737098885,-0.702075375912999));
#6685=CARTESIAN_POINT('Ctrl Pts',(4.64235365513237,-0.413359383977703,-0.701814015570827));
#6686=CARTESIAN_POINT('Ctrl Pts',(4.6471143769742,-0.40052929715995,-0.700896550309365));
#6687=CARTESIAN_POINT('Ctrl Pts',(4.65040932566734,-0.391297760024812,-0.700245786661472));
#6688=CARTESIAN_POINT('Ctrl Pts',(4.67668190005899,-0.314681260081685,-0.694913501140349));
#6689=CARTESIAN_POINT('Ctrl Pts',(4.69362443346622,-0.245371636196225,-0.690520723646131));
#6690=CARTESIAN_POINT('Ctrl Pts',(4.71294218216511,-0.116767203974033,-0.682476742640783));
#6691=CARTESIAN_POINT('Ctrl Pts',(4.71730924433082,-0.0580174760102126,
-0.678840815355901));
#6692=CARTESIAN_POINT('Ctrl Pts',(4.71725417857355,0.0220216548452417,-0.673739202646583));
#6693=CARTESIAN_POINT('Ctrl Pts',(4.71666656343383,0.0432277413949803,-0.672374017768371));
#6694=CARTESIAN_POINT('Ctrl Pts',(4.7146477537229,0.0800894300116951,-0.669969176964529));
#6695=CARTESIAN_POINT('Ctrl Pts',(4.71347515043739,0.0957539741828366,-0.668937221381266));
#6696=CARTESIAN_POINT('Ctrl Pts',(4.71130920694993,0.118552336391043,-0.667418537026304));
#6697=CARTESIAN_POINT('Ctrl Pts',(4.71056312962085,0.125708345514172,-0.666939436700112));
#6698=CARTESIAN_POINT('Ctrl Pts',(4.70913342086259,0.138301527783642,-0.666091858638477));
#6699=CARTESIAN_POINT('Ctrl Pts',(4.708477314275,0.143741656343089,-0.665724245326205));
#6700=CARTESIAN_POINT('Ctrl Pts',(4.70702935797867,0.155081181386098,-0.664954826762459));
#6701=CARTESIAN_POINT('Ctrl Pts',(4.70623070192685,0.160979536189289,-0.664552819428059));
#6702=CARTESIAN_POINT('Ctrl Pts',(4.70402842114411,0.176366043482055,-0.663499339699145));
#6703=CARTESIAN_POINT('Ctrl Pts',(4.7025535646726,0.185843388415899,-0.662845666701782));
#6704=CARTESIAN_POINT('Ctrl Pts',(4.69582292627179,0.225870030830573,-0.66006400337114));
#6705=CARTESIAN_POINT('Ctrl Pts',(4.68947834026259,0.256221093285343,-0.657902500612395));
#6706=CARTESIAN_POINT('Ctrl Pts',(4.66175928895829,0.366834741893492,-0.649826221414154));
#6707=CARTESIAN_POINT('Ctrl Pts',(4.63311311665378,0.445016349434409,-0.643705355196698));
#6708=CARTESIAN_POINT('Ctrl Pts',(4.57349100981242,0.566317723505985,-0.633811177738374));
#6709=CARTESIAN_POINT('Ctrl Pts',(4.54740564813502,0.611538782282844,-0.630028315018804));
#6710=CARTESIAN_POINT('Ctrl Pts',(4.51453737800882,0.660668387759828,-0.625917024807517));
#6711=CARTESIAN_POINT('Ctrl Pts',(4.5106178609278,0.666416209135279,-0.625436051349425));
#6712=CARTESIAN_POINT('Ctrl Pts',(4.5045583301707,0.675135284761337,-0.624706877598847));
#6713=CARTESIAN_POINT('Ctrl Pts',(4.50245509286179,0.678131730030445,-0.624456364723646));
#6714=CARTESIAN_POINT('Ctrl Pts',(4.49857887217485,0.683599716204206,-0.62399943936819));
#6715=CARTESIAN_POINT('Ctrl Pts',(4.49681028021669,0.686074205534111,-0.62379275103892));
#6716=CARTESIAN_POINT('Ctrl Pts',(4.49279566884896,0.691645418160335,-0.623327583656288));
#6717=CARTESIAN_POINT('Ctrl Pts',(4.49054413556597,0.694738068743461,-0.623069482746365));
#6718=CARTESIAN_POINT('Ctrl Pts',(4.48468548333397,0.702703515435972,-0.622404869374956));
#6719=CARTESIAN_POINT('Ctrl Pts',(4.48105568348254,0.707559600974885,-0.621999840755215));
#6720=CARTESIAN_POINT('Ctrl Pts',(4.45643277879081,0.739976041151459,-0.61929548392679));
#6721=CARTESIAN_POINT('Ctrl Pts',(4.4342677094121,0.766629421105363,-0.617068717688261));
#6722=CARTESIAN_POINT('Ctrl Pts',(4.39197017125308,0.813153627948617,-0.613095667419175));
#6723=CARTESIAN_POINT('Ctrl Pts',(4.37223764639561,0.83334962476219,-0.6113381980851));
#6724=CARTESIAN_POINT('Ctrl Pts',(4.31706497679318,0.885899642417509,-0.606614124979173));
#6725=CARTESIAN_POINT('Ctrl Pts',(4.28034418190566,0.916828160617236,-0.60366447820395));
#6726=CARTESIAN_POINT('Ctrl Pts',(4.19900455947919,0.977251953123329,-0.597328175616331));
#6727=CARTESIAN_POINT('Ctrl Pts',(4.15406105479072,1.00612104417369,-0.593936107167316));
#6728=CARTESIAN_POINT('Ctrl Pts',(4.09782796236123,1.0370648888041,-0.589717631800969));
#6729=CARTESIAN_POINT('Ctrl Pts',(4.08826535138482,1.04215637460957,-0.589001273482033));
#6730=CARTESIAN_POINT('Ctrl Pts',(4.07310138206807,1.04996365813097,-0.58786618172041));
#6731=CARTESIAN_POINT('Ctrl Pts',(4.0675462465069,1.05276828681743,-0.587450538969502));
#6732=CARTESIAN_POINT('Ctrl Pts',(4.05710439987679,1.05793663952144,-0.586669477544284));
#6733=CARTESIAN_POINT('Ctrl Pts',(4.05222304822086,1.06031086770052,-0.586304432982237));
#6734=CARTESIAN_POINT('Ctrl Pts',(4.04125803340685,1.06555069180061,-0.585484530986028));
#6735=CARTESIAN_POINT('Ctrl Pts',(4.03516592921754,1.06839807756334,-0.585029065845042));
#6736=CARTESIAN_POINT('Ctrl Pts',(4.01960214284205,1.07551066388787,-0.583865473250612));
#6737=CARTESIAN_POINT('Ctrl Pts',(4.01009796859312,1.07970293764442,-0.583154916002278));
#6738=CARTESIAN_POINT('Ctrl Pts',(3.93114963436176,1.11328650496325,-0.577251064435099));
#6739=CARTESIAN_POINT('Ctrl Pts',(3.85909799301456,1.13606636397634,-0.571836493757893));
#6740=CARTESIAN_POINT('Ctrl Pts',(3.72893207294945,1.16385091630774,-0.562100384833522));
#6741=CARTESIAN_POINT('Ctrl Pts',(3.6716772924882,1.17173405437578,-0.557837701210622));
#6742=CARTESIAN_POINT('Ctrl Pts',(3.59353599937772,1.17669059596362,-0.552183027628493));
#6743=CARTESIAN_POINT('Ctrl Pts',(3.57296562531858,1.17745488945251,-0.550710203259791));
#6744=CARTESIAN_POINT('Ctrl Pts',(3.5392954801517,1.17782271969558,-0.548335318281514));
#6745=CARTESIAN_POINT('Ctrl Pts',(3.5262041532421,1.17774749339292,-0.547420816853431));
#6746=CARTESIAN_POINT('Ctrl Pts',(3.50840960648368,1.17734847331151,-0.546192189089015));
#6747=CARTESIAN_POINT('Ctrl Pts',(3.50370364540243,1.17721471438579,-0.545868637771748));
#6748=CARTESIAN_POINT('Ctrl Pts',(3.49582678100196,1.17694355000632,-0.545329512527767));
#6749=CARTESIAN_POINT('Ctrl Pts',(3.49265544192516,1.17682154012441,-0.545113114684295));
#6750=CARTESIAN_POINT('Ctrl Pts',(3.48662904248441,1.17656528860321,-0.5447032060178));
#6751=CARTESIAN_POINT('Ctrl Pts',(3.48377392680237,1.17643347152374,-0.544509559187604));
#6752=CARTESIAN_POINT('Ctrl Pts',(3.4769863838525,1.17609533379558,-0.544050456644416));
#6753=CARTESIAN_POINT('Ctrl Pts',(3.47305442450417,1.17587968056627,-0.543785508299114));
#6754=CARTESIAN_POINT('Ctrl Pts',(3.45913654671919,1.17504630268861,-0.542851002320313));
#6755=CARTESIAN_POINT('Ctrl Pts',(3.44915716117522,1.17432104025507,-0.542187009214251));
#6756=CARTESIAN_POINT('Ctrl Pts',(3.37649840170159,1.16810873799805,-0.537388895013115));
#6757=CARTESIAN_POINT('Ctrl Pts',(3.3143306057952,1.15773313196141,-0.533477738502758));
#6758=CARTESIAN_POINT('Ctrl Pts',(3.19279366532602,1.12728221874041,-0.525719715587363));
#6759=CARTESIAN_POINT('Ctrl Pts',(3.13360704270085,1.10734754524679,-0.52188301482203));
#6760=CARTESIAN_POINT('Ctrl Pts',(3.04357354125242,1.06883042761197,-0.515665273788253));
#6761=CARTESIAN_POINT('Ctrl Pts',(3.01152217534904,1.05336572442389,-0.513371551354849));
#6762=CARTESIAN_POINT('Ctrl Pts',(2.97168790094352,1.03187057455983,-0.510389305659565));
#6763=CARTESIAN_POINT('Ctrl Pts',(2.96321137931696,1.02716043340691,-0.509746887872278));
#6764=CARTESIAN_POINT('Ctrl Pts',(2.94960534160534,1.01937854118037,-0.508702506422669));
#6765=CARTESIAN_POINT('Ctrl Pts',(2.94443924513565,1.01637139726705,-0.508302837680211));
#6766=CARTESIAN_POINT('Ctrl Pts',(2.93458453332311,1.01053415729336,-0.507534306565444));
#6767=CARTESIAN_POINT('Ctrl Pts',(2.92989231613606,1.00771042276113,-0.507165679822961));
#6768=CARTESIAN_POINT('Ctrl Pts',(2.91922001133851,1.001186106108,-0.506320966044665));
#6769=CARTESIAN_POINT('Ctrl Pts',(2.91325308112705,0.997464510117761,-0.505844126681568));
#6770=CARTESIAN_POINT('Ctrl Pts',(2.89447572171364,0.985518095710768,-0.504328829548049));
#6771=CARTESIAN_POINT('Ctrl Pts',(2.88179168990913,0.977098508108748,-0.503283294007638));
#6772=CARTESIAN_POINT('Ctrl Pts',(2.79849433201982,0.919449288834153,-0.496265998921689));
#6773=CARTESIAN_POINT('Ctrl Pts',(2.73331010182913,0.862859493913574,-0.490010157572538));
#6774=CARTESIAN_POINT('Ctrl Pts',(2.64128832777086,0.763364062141092,-0.480064157035253));
#6775=CARTESIAN_POINT('Ctrl Pts',(2.61001358585827,0.724957405587742,-0.476429821568471));
#6776=CARTESIAN_POINT('Ctrl Pts',(2.57220907780569,0.672047702865381,-0.471771685140373));
#6777=CARTESIAN_POINT('Ctrl Pts',(2.56342288198954,0.659221523585968,-0.470667668710592));
#6778=CARTESIAN_POINT('Ctrl Pts',(2.54904844629212,0.637319775002072,-0.468828985805786));
#6779=CARTESIAN_POINT('Ctrl Pts',(2.54332493433572,0.62833575115913,-0.468087556264866));
#6780=CARTESIAN_POINT('Ctrl Pts',(2.53543978477891,0.615580019273414,-0.467054028632626));
#6781=CARTESIAN_POINT('Ctrl Pts',(2.53317613291337,0.611872426003054,-0.466755868346626));
#6782=CARTESIAN_POINT('Ctrl Pts',(2.52933052133893,0.605494697835627,-0.46624692796133));
#6783=CARTESIAN_POINT('Ctrl Pts',(2.52773852007144,0.602830699880699,-0.466035514820911));
#6784=CARTESIAN_POINT('Ctrl Pts',(2.52466024614019,0.597633079228416,-0.465625351499246));
#6785=CARTESIAN_POINT('Ctrl Pts',(2.52317290790217,0.595100167266194,-0.465426527806647));
#6786=CARTESIAN_POINT('Ctrl Pts',(2.51911476997904,0.588129635191564,-0.464882190848579));
#6787=CARTESIAN_POINT('Ctrl Pts',(2.51656341656705,0.583680680597963,-0.464537893310958));
#6788=CARTESIAN_POINT('Ctrl Pts',(2.50663973876124,0.566111193398668,-0.463189898050406));
#6789=CARTESIAN_POINT('Ctrl Pts',(2.49948975314791,0.552865868291557,-0.462199131912969));
#6790=CARTESIAN_POINT('Ctrl Pts',(2.48079891243461,0.516594542644462,-0.459544318379849));
#6791=CARTESIAN_POINT('Ctrl Pts',(2.46975579057744,0.493320379541933,-0.457903096754138));
#6792=CARTESIAN_POINT('Ctrl Pts',(2.43866585011557,0.421831926798036,-0.452993197536466));
#6793=CARTESIAN_POINT('Ctrl Pts',(2.42105243085542,0.37262957223303,-0.449787385593403));
#6794=CARTESIAN_POINT('Ctrl Pts',(2.38680369428382,0.252303245680422,-0.442037562267477));
#6795=CARTESIAN_POINT('Ctrl Pts',(2.37340204448034,0.180495606953495,-0.437476198545167));
#6796=CARTESIAN_POINT('Ctrl Pts',(2.36576884580909,0.0975401421354294,-0.432009429681297));
#6797=CARTESIAN_POINT('Ctrl Pts',(2.3649518993186,0.0871528450724344,-0.431321692456492));
#6798=CARTESIAN_POINT('Ctrl Pts',(2.3638342430538,0.0700399756648277,-0.430182711244844));
#6799=CARTESIAN_POINT('Ctrl Pts',(2.36345318195266,0.0633200941985408,-0.429733950973512));
#6800=CARTESIAN_POINT('Ctrl Pts',(2.36286911964247,0.0511802383485442,-0.428920356891009));
#6801=CARTESIAN_POINT('Ctrl Pts',(2.362645917926,0.045761389049225,-0.428556158269894));
#6802=CARTESIAN_POINT('Ctrl Pts',(2.36224754351222,0.0341378042762881,-0.427772631466832));
#6803=CARTESIAN_POINT('Ctrl Pts',(2.36208398072578,0.0279328617127304,-0.427352955289438));
#6804=CARTESIAN_POINT('Ctrl Pts',(2.36177063975281,0.0109505707505099,-0.426200336928075));
#6805=CARTESIAN_POINT('Ctrl Pts',(2.36171975055371,0.000172225592996742,
-0.425464370900915));
#6806=CARTESIAN_POINT('Ctrl Pts',(2.36228815092201,-0.0629495674470405,
-0.421127166975548));
#6807=CARTESIAN_POINT('Ctrl Pts',(2.36624861359716,-0.115196890798785,-0.417423970045857));
#6808=CARTESIAN_POINT('Ctrl Pts',(2.3846456014432,-0.243627653030059,-0.408053258502117));
#6809=CARTESIAN_POINT('Ctrl Pts',(2.40314844599993,-0.318979470628389,-0.402308323745594));
#6810=CARTESIAN_POINT('Ctrl Pts',(2.44041472212273,-0.424570381034427,-0.394189749252246));
#6811=CARTESIAN_POINT('Ctrl Pts',(2.45335211089965,-0.456653266429886,-0.391716164687622));
#6812=CARTESIAN_POINT('Ctrl Pts',(2.4701938787623,-0.49363490295437,-0.388891676654412));
#6813=CARTESIAN_POINT('Ctrl Pts',(2.47274644084436,-0.499127181662356,-0.388472927190597));
#6814=CARTESIAN_POINT('Ctrl Pts',(2.47697873190624,-0.508052890830636,-0.387793874028403));
#6815=CARTESIAN_POINT('Ctrl Pts',(2.47863296944214,-0.511498184330585,-0.38753212263193));
#6816=CARTESIAN_POINT('Ctrl Pts',(2.48163303910204,-0.517669286275346,-0.387064010937824));
#6817=CARTESIAN_POINT('Ctrl Pts',(2.48297267462688,-0.520397981662914,-0.386857288022044));
#6818=CARTESIAN_POINT('Ctrl Pts',(2.48594857656599,-0.526400716910466,-0.386403109047352));
#6819=CARTESIAN_POINT('Ctrl Pts',(2.48758954705423,-0.529672331729539,-0.386155944910589));
#6820=CARTESIAN_POINT('Ctrl Pts',(2.49239283842223,-0.539138319672939,-0.385441737465978));
#6821=CARTESIAN_POINT('Ctrl Pts',(2.49559487486044,-0.545312527862871,-0.384977054239299));
#6822=CARTESIAN_POINT('Ctrl Pts',(2.52321642272114,-0.597437691035325,-0.381060800405111));
#6823=CARTESIAN_POINT('Ctrl Pts',(2.55060525970189,-0.641758361821393,-0.377774770905265));
#6824=CARTESIAN_POINT('Ctrl Pts',(2.62889195496161,-0.751462911630926,-0.369379228826727));
#6825=CARTESIAN_POINT('Ctrl Pts',(2.68390195297865,-0.813546090546265,-0.364345822705794));
#6826=CARTESIAN_POINT('Ctrl Pts',(2.76821455933966,-0.890604704517804,-0.357066201713279));
#6827=CARTESIAN_POINT('Ctrl Pts',(2.79230816550589,-0.9109132663389,-0.355029515449641));
#6828=CARTESIAN_POINT('Ctrl Pts',(2.82481215057754,-0.93615295519475,-0.352317847251739));
#6829=CARTESIAN_POINT('Ctrl Pts',(2.83251147328147,-0.941981202015655,-0.351678074832365));
#6830=CARTESIAN_POINT('Ctrl Pts',(2.84508415781752,-0.951257517986378,-0.350636948144735));
#6831=CARTESIAN_POINT('Ctrl Pts',(2.84991369861984,-0.95476444327421,-0.350237862977285));
#6832=CARTESIAN_POINT('Ctrl Pts',(2.85922709550427,-0.961419749032661,-0.349469748097654));
#6833=CARTESIAN_POINT('Ctrl Pts',(2.86370668430362,-0.964573855035549,-0.349100948816312));
#6834=CARTESIAN_POINT('Ctrl Pts',(2.87409956674137,-0.971783611343328,-0.348246716411219));
#6835=CARTESIAN_POINT('Ctrl Pts',(2.88002816673208,-0.975816707652761,-0.347760455291054));
#6836=CARTESIAN_POINT('Ctrl Pts',(2.89893811511055,-0.988429690411587,-0.346212484258325));
#6837=CARTESIAN_POINT('Ctrl Pts',(2.91205239458709,-0.996806271698867,-0.345143373329822));
#6838=CARTESIAN_POINT('Ctrl Pts',(2.94320612257778,-1.01584692007562,-0.342612705836933));
#6839=CARTESIAN_POINT('Ctrl Pts',(2.96137138418869,-1.02629394234843,-0.341143986729184));
#6840=CARTESIAN_POINT('Ctrl Pts',(3.03048086246985,-1.0636223408543,-0.335581141046875));
#6841=CARTESIAN_POINT('Ctrl Pts',(3.08309130671424,-1.08723720788527,-0.331390727282636));
#6842=CARTESIAN_POINT('Ctrl Pts',(3.20572098532464,-1.13180713383808,-0.32182359724022));
#6843=CARTESIAN_POINT('Ctrl Pts',(3.2763993843832,-1.15029492596286,-0.316444645571545));
#6844=CARTESIAN_POINT('Ctrl Pts',(3.3579025579419,-1.16370290727511,-0.310657113710584));
#6845=CARTESIAN_POINT('Ctrl Pts',(3.36748593749116,-1.16515819950296,-0.309983149321902));
#6846=CARTESIAN_POINT('Ctrl Pts',(3.38093760400852,-1.1670313215176,-0.30904729256321));
#6847=CARTESIAN_POINT('Ctrl Pts',(3.38479134147459,-1.16754850764564,-0.308780344875128));
#6848=CARTESIAN_POINT('Ctrl Pts',(3.39147208344645,-1.16841142953133,-0.308319666718604));
#6849=CARTESIAN_POINT('Ctrl Pts',(3.39429788585235,-1.16876601034484,-0.308125458803245));
#6850=CARTESIAN_POINT('Ctrl Pts',(3.40030619881635,-1.1694978044744,-0.307713944444898));
#6851=CARTESIAN_POINT('Ctrl Pts',(3.40348902512183,-1.16987228600488,-0.307496792866438));
#6852=CARTESIAN_POINT('Ctrl Pts',(3.41145269819462,-1.17077632709621,-0.306955480827591));
#6853=CARTESIAN_POINT('Ctrl Pts',(3.41623538933698,-1.17128960533117,-0.30663220510854));
#6854=CARTESIAN_POINT('Ctrl Pts',(3.43470570617148,-1.17315745165342,-0.305390284421834));
#6855=CARTESIAN_POINT('Ctrl Pts',(3.44841414207368,-1.17430157085485,-0.304482392145445));
#6856=CARTESIAN_POINT('Ctrl Pts',(3.4841273431563,-1.17665302959701,-0.302145807390136));
#6857=CARTESIAN_POINT('Ctrl Pts',(3.50615217395362,-1.17748348771582,-0.300732997229318));
#6858=CARTESIAN_POINT('Ctrl Pts',(3.63732332438298,-1.17874546582077,-0.292419217168538));
#6859=CARTESIAN_POINT('Ctrl Pts',(3.74607357239828,-1.16462181751565,-0.285887590347448));
#6860=CARTESIAN_POINT('Ctrl Pts',(3.87625889933871,-1.12887984453467,-0.277223401480889));
#6861=CARTESIAN_POINT('Ctrl Pts',(3.90095545211669,-1.12121675006157,-0.275543252923995));
#6862=CARTESIAN_POINT('Ctrl Pts',(3.93388533123544,-1.10979789439828,-0.273242994905945));
#6863=CARTESIAN_POINT('Ctrl Pts',(3.94235783155502,-1.10675066698364,-0.272645730522776));
#6864=CARTESIAN_POINT('Ctrl Pts',(3.95626348543776,-1.10156851971587,-0.271656069168298));
#6865=CARTESIAN_POINT('Ctrl Pts',(3.96171728815671,-1.09948977881939,-0.27126552021832));
#6866=CARTESIAN_POINT('Ctrl Pts',(3.97232662818089,-1.09535540648099,-0.270500969158009));
#6867=CARTESIAN_POINT('Ctrl Pts',(3.97748353676146,-1.09330369649639,-0.270127105007017));
#6868=CARTESIAN_POINT('Ctrl Pts',(3.98963103553707,-1.08837099851889,-0.269241040224813));
#6869=CARTESIAN_POINT('Ctrl Pts',(3.99660869424102,-1.08545901924974,-0.26872782021178));
#6870=CARTESIAN_POINT('Ctrl Pts',(4.01986012249731,-1.07549157406541,-0.267003046112239));
#6871=CARTESIAN_POINT('Ctrl Pts',(4.03600178336608,-1.06813599704391,-0.265781531605415));
#6872=CARTESIAN_POINT('Ctrl Pts',(4.060759723617,-1.05617163136073,-0.263869136273379));
#6873=CARTESIAN_POINT('Ctrl Pts',(4.06949331464938,-1.05181629783442,-0.263186859774962));
#6874=CARTESIAN_POINT('Ctrl Pts',(4.07816931076926,-1.04735426648718,-0.262501355395651));
#6875=CARTESIAN_POINT('',(2.36176935163321,-0.000842318577373219,-0.325632885263839));
#6876=CARTESIAN_POINT('Ctrl Pts',(4.07816926754758,-1.04735428871592,-0.162850680997093));
#6877=CARTESIAN_POINT('Ctrl Pts',(4.03648879475578,-1.0687903929655,-0.166030123892547));
#6878=CARTESIAN_POINT('Ctrl Pts',(3.99344742609404,-1.08777537239131,-0.169209566788002));
#6879=CARTESIAN_POINT('Ctrl Pts',(3.9493633730446,-1.10413889240205,-0.172389009683457));
#6880=CARTESIAN_POINT('Ctrl Pts',(3.90533328117549,-1.12048238261079,-0.175564560774969));
#6881=CARTESIAN_POINT('Ctrl Pts',(3.86026354815364,-1.13421057160714,-0.178740111866482));
#6882=CARTESIAN_POINT('Ctrl Pts',(3.81449436851147,-1.14520026062787,-0.181915662957994));
#6883=CARTESIAN_POINT('Ctrl Pts',(3.76876124798889,-1.15618129145297,-0.1850887122005));
#6884=CARTESIAN_POINT('Ctrl Pts',(3.72233031060124,-1.16442796521287,-0.188261761443006));
#6885=CARTESIAN_POINT('Ctrl Pts',(3.6755564187704,-1.16986704240829,-0.191434810685512));
#6886=CARTESIAN_POINT('Ctrl Pts',(3.62879897667555,-1.17530420675488,-0.194606744010136));
#6887=CARTESIAN_POINT('Ctrl Pts',(3.58169937055643,-1.17793566842164,-0.19777867733476));
#6888=CARTESIAN_POINT('Ctrl Pts',(3.53461946523157,-1.1777398085167,-0.200950610659384));
#6889=CARTESIAN_POINT('Ctrl Pts',(3.48750099629399,-1.17754378818098,-0.204125142145739));
#6890=CARTESIAN_POINT('Ctrl Pts',(3.44040281706057,-1.17451581787525,-0.207299673632094));
#6891=CARTESIAN_POINT('Ctrl Pts',(3.3936867592207,-1.16868644440786,-0.210474205118449));
#6892=CARTESIAN_POINT('Ctrl Pts',(3.34695251665996,-1.16285480179504,-0.213649972324846));
#6893=CARTESIAN_POINT('Ctrl Pts',(3.3006012400234,-1.15421967962168,-0.216825739531243));
#6894=CARTESIAN_POINT('Ctrl Pts',(3.25498596040136,-1.14286306405568,-0.220001506737639));
#6895=CARTESIAN_POINT('Ctrl Pts',(3.2092830980799,-1.13148464344857,-0.223183371511935));
#6896=CARTESIAN_POINT('Ctrl Pts',(3.16431958840069,-1.11737445457709,-0.22636523628623));
#6897=CARTESIAN_POINT('Ctrl Pts',(3.12043315625231,-1.10066437927606,-0.229547101060525));
#6898=CARTESIAN_POINT('Ctrl Pts',(3.08617027849336,-1.08761854165941,-0.232031236554579));
#6899=CARTESIAN_POINT('Ctrl Pts',(3.05256362255288,-1.07298905960761,-0.234515372048633));
#6900=CARTESIAN_POINT('Ctrl Pts',(3.01976355863634,-1.05685821719737,-0.236999507542687));
#6901=CARTESIAN_POINT('Ctrl Pts',(2.97630109333403,-1.03548368023501,-0.240291167369668));
#6902=CARTESIAN_POINT('Ctrl Pts',(2.93406351792174,-1.0113765558278,-0.24358282719665));
#6903=CARTESIAN_POINT('Ctrl Pts',(2.89341309480587,-0.984704095967967,-0.246874487023632));
#6904=CARTESIAN_POINT('Ctrl Pts',(2.85416982043374,-0.958954925843083,-0.250052203264414));
#6905=CARTESIAN_POINT('Ctrl Pts',(2.81640611387305,-0.930815467375344,-0.253229919505196));
#6906=CARTESIAN_POINT('Ctrl Pts',(2.78042461561076,-0.900483593152643,-0.256407635745978));
#6907=CARTESIAN_POINT('Ctrl Pts',(2.74447761515567,-0.870180800074408,-0.259582305303117));
#6908=CARTESIAN_POINT('Ctrl Pts',(2.71030986328289,-0.837690108820577,-0.262756974860256));
#6909=CARTESIAN_POINT('Ctrl Pts',(2.67819299342287,-0.803251197342788,-0.265931644417395));
#6910=CARTESIAN_POINT('Ctrl Pts',(2.64609291826073,-0.768830294815317,-0.269104653862066));
#6911=CARTESIAN_POINT('Ctrl Pts',(2.61604197842615,-0.732463596067216,-0.272277663306736));
#6912=CARTESIAN_POINT('Ctrl Pts',(2.58827484689098,-0.694427481992727,-0.275450672751407));
#6913=CARTESIAN_POINT('Ctrl Pts',(2.56051013444798,-0.656394681651432,-0.278623405761248));
#6914=CARTESIAN_POINT('Ctrl Pts',(2.53502916050988,-0.616693204514807,-0.281796138771089));
#6915=CARTESIAN_POINT('Ctrl Pts',(2.51202454191676,-0.575630174234756,-0.28496887178093));
#6916=CARTESIAN_POINT('Ctrl Pts',(2.48899611590444,-0.534524647932812,-0.288144888243807));
#6917=CARTESIAN_POINT('Ctrl Pts',(2.46844942873736,-0.492055243244083,-0.291320904706685));
#6918=CARTESIAN_POINT('Ctrl Pts',(2.45053121156843,-0.448553842171557,-0.294496921169562));
#6919=CARTESIAN_POINT('Ctrl Pts',(2.4326018017593,-0.405025267886123,-0.297674921535702));
#6920=CARTESIAN_POINT('Ctrl Pts',(2.41730430957338,-0.36046393975318,-0.300852921901843));
#6921=CARTESIAN_POINT('Ctrl Pts',(2.40473608172682,-0.315218458306463,-0.304030922267983));
#6922=CARTESIAN_POINT('Ctrl Pts',(2.39214524396919,-0.269891581429597,-0.307214639773129));
#6923=CARTESIAN_POINT('Ctrl Pts',(2.38229357788065,-0.223878639106408,-0.310398357278275));
#6924=CARTESIAN_POINT('Ctrl Pts',(2.37522729932057,-0.177538110880048,-0.313582074783422));
#6925=CARTESIAN_POINT('Ctrl Pts',(2.37343891898607,-0.165809944679764,-0.314387830985697));
#6926=CARTESIAN_POINT('Ctrl Pts',(2.37182869035538,-0.154060812079169,-0.315193587187973));
#6927=CARTESIAN_POINT('Ctrl Pts',(2.37039683387009,-0.142296539882158,-0.315999343390248));
#6928=CARTESIAN_POINT('Ctrl Pts',(2.3646904554523,-0.095412379593892,-0.319210524014779));
#6929=CARTESIAN_POINT('Ctrl Pts',(2.3618032037766,-0.0481751837724696,-0.322421704639309));
#6930=CARTESIAN_POINT('Ctrl Pts',(2.36176935163321,-0.000842318577373219,
-0.325632885263839));
#6931=CARTESIAN_POINT('Ctrl Pts',(2.3617693838383,-0.00088620519429726,
-0.326328626527825));
#6932=CARTESIAN_POINT('Ctrl Pts',(2.36168697442929,0.108634315111176,-0.333237160701623));
#6933=CARTESIAN_POINT('Ctrl Pts',(2.37688011695775,0.217634663538543,-0.339791136799143));
#6934=CARTESIAN_POINT('Ctrl Pts',(2.4112740138359,0.338245985790649,-0.347863569349079));
#6935=CARTESIAN_POINT('Ctrl Pts',(2.41593677931753,0.353426163559503,-0.348893890434319));
#6936=CARTESIAN_POINT('Ctrl Pts',(2.42482307569376,0.380400793188009,-0.350753733509043));
#6937=CARTESIAN_POINT('Ctrl Pts',(2.42893061655525,0.392231042178549,-0.351579547541527));
#6938=CARTESIAN_POINT('Ctrl Pts',(2.43547263533047,0.410145677589036,-0.352846697530529));
#6939=CARTESIAN_POINT('Ctrl Pts',(2.43777063119874,0.416279210781812,-0.353283537891786));
#6940=CARTESIAN_POINT('Ctrl Pts',(2.44186223727288,0.426928789990344,-0.354047405745229));
#6941=CARTESIAN_POINT('Ctrl Pts',(2.4436328733024,0.431453539511446,-0.354373662110115));
#6942=CARTESIAN_POINT('Ctrl Pts',(2.44768333197325,0.44161842628527,-0.355110521967119));
#6943=CARTESIAN_POINT('Ctrl Pts',(2.44997894358078,0.447252080696719,-0.35552164685082));
#6944=CARTESIAN_POINT('Ctrl Pts',(2.45628724947051,0.462396454681113,-0.356634375052862));
#6945=CARTESIAN_POINT('Ctrl Pts',(2.46038142670843,0.471872433114153,-0.357338703637262));
#6946=CARTESIAN_POINT('Ctrl Pts',(2.4805796305919,0.516983080198633,-0.360731520999217));
#6947=CARTESIAN_POINT('Ctrl Pts',(2.49832550390408,0.551851057964409,-0.363475290433457));
#6948=CARTESIAN_POINT('Ctrl Pts',(2.56016817984527,0.659722375024465,-0.372360792069148));
#6949=CARTESIAN_POINT('Ctrl Pts',(2.61046752690619,0.728849965862253,-0.378685905895085));
#6950=CARTESIAN_POINT('Ctrl Pts',(2.68673643930151,0.812804987824375,-0.386952545903791));
#6951=CARTESIAN_POINT('Ctrl Pts',(2.70644115942162,0.83298953900932,-0.388990140799229));
#6952=CARTESIAN_POINT('Ctrl Pts',(2.73478813095285,0.860013611376803,-0.391768860120055));
#6953=CARTESIAN_POINT('Ctrl Pts',(2.74282914441637,0.86746785395331,-0.392541027153686));
#6954=CARTESIAN_POINT('Ctrl Pts',(2.7569223959563,0.880171395036631,-0.393865226461982));
#6955=CARTESIAN_POINT('Ctrl Pts',(2.76292614743906,0.885473139109411,-0.394420460966358));
#6956=CARTESIAN_POINT('Ctrl Pts',(2.77192101918803,0.893254392263535,-0.395238654559867));
#6957=CARTESIAN_POINT('Ctrl Pts',(2.77487092324347,0.895780882552836,-0.395504839933977));
#6958=CARTESIAN_POINT('Ctrl Pts',(2.78012179328468,0.900233231331982,-0.395974785218987));
#6959=CARTESIAN_POINT('Ctrl Pts',(2.78241766033256,0.902164924318805,-0.396178959411012));
#6960=CARTESIAN_POINT('Ctrl Pts',(2.78742245995206,0.906343293668238,-0.396621220804574));
#6961=CARTESIAN_POINT('Ctrl Pts',(2.79013408968879,0.908586610518872,-0.396859069664233));
#6962=CARTESIAN_POINT('Ctrl Pts',(2.79759042463452,0.914699108094887,-0.397508392747629));
#6963=CARTESIAN_POINT('Ctrl Pts',(2.80235538891057,0.918543566875013,-0.397918164604192));
#6964=CARTESIAN_POINT('Ctrl Pts',(2.82725885899987,0.93831752361345,-0.40003435273515));
#6965=CARTESIAN_POINT('Ctrl Pts',(2.84788600843057,0.953623781698629,-0.401701615324763));
#6966=CARTESIAN_POINT('Ctrl Pts',(2.87836036939974,0.974727617884295,-0.404070550069948));
#6967=CARTESIAN_POINT('Ctrl Pts',(2.88781570976759,0.981074665709309,-0.404793012887576));
#6968=CARTESIAN_POINT('Ctrl Pts',(2.95939898335455,1.02763444647273,-0.410180820038382));
#6969=CARTESIAN_POINT('Ctrl Pts',(3.02510285903924,1.0620493044245,-0.414680448546493));
#6970=CARTESIAN_POINT('Ctrl Pts',(3.14374750320947,1.11058319039115,-0.422692628063581));
#6971=CARTESIAN_POINT('Ctrl Pts',(3.19524009606638,1.12760853877295,-0.426134584669825));
#6972=CARTESIAN_POINT('Ctrl Pts',(3.25826790389293,1.14372700071162,-0.430410126093525));
#6973=CARTESIAN_POINT('Ctrl Pts',(3.26885520119699,1.14627864297862,-0.431130221486981));
#6974=CARTESIAN_POINT('Ctrl Pts',(3.28556747898213,1.15006202817494,-0.432270585095368));
#6975=CARTESIAN_POINT('Ctrl Pts',(3.29166965160461,1.15139252310599,-0.432687732009335));
#6976=CARTESIAN_POINT('Ctrl Pts',(3.30310835136465,1.15379142891049,-0.433471246938598));
#6977=CARTESIAN_POINT('Ctrl Pts',(3.30844228287727,1.15487151054093,-0.433837236617798));
#6978=CARTESIAN_POINT('Ctrl Pts',(3.32039375465797,1.15720548307719,-0.434658794946688));
#6979=CARTESIAN_POINT('Ctrl Pts',(3.32701490686117,1.15843964496585,-0.435114969099434));
#6980=CARTESIAN_POINT('Ctrl Pts',(3.34387792244817,1.16143342473726,-0.436279548035995));
#6981=CARTESIAN_POINT('Ctrl Pts',(3.35413298064496,1.16311437280737,-0.436990372905088));
#6982=CARTESIAN_POINT('Ctrl Pts',(3.43846878062212,1.17579453943486,-0.4428588030807));
#6983=CARTESIAN_POINT('Ctrl Pts',(3.51340844765557,1.17983830107933,-0.448233681952999));
#6984=CARTESIAN_POINT('Ctrl Pts',(3.64542038779149,1.17437574872178,-0.45789229303986));
#6985=CARTESIAN_POINT('Ctrl Pts',(3.70238080571172,1.16783978823402,-0.46211810922811));
#6986=CARTESIAN_POINT('Ctrl Pts',(3.77902224233109,1.15332718177776,-0.467750668621716));
#6987=CARTESIAN_POINT('Ctrl Pts',(3.7992995701186,1.14892974135766,-0.469235134233333));
#6988=CARTESIAN_POINT('Ctrl Pts',(3.83224627818835,1.1408678044226,-0.471627283023445));
#6989=CARTESIAN_POINT('Ctrl Pts',(3.84498853188288,1.13752231144036,-0.472547521418659));
#6990=CARTESIAN_POINT('Ctrl Pts',(3.86222793237053,1.13268549227179,-0.473783423714395));
#6991=CARTESIAN_POINT('Ctrl Pts',(3.86677560466676,1.13137995231716,-0.474108578871976));
#6992=CARTESIAN_POINT('Ctrl Pts',(3.87437398894227,1.12914896900803,-0.474650258735744));
#6993=CARTESIAN_POINT('Ctrl Pts',(3.87742898614855,1.12823849431332,-0.474867611476438));
#6994=CARTESIAN_POINT('Ctrl Pts',(3.88321838829966,1.12648746580278,-0.475278633550124));
#6995=CARTESIAN_POINT('Ctrl Pts',(3.88595348981981,1.12564933487802,-0.475472442611575));
#6996=CARTESIAN_POINT('Ctrl Pts',(3.89244917617556,1.12363291101652,-0.475931903337706));
#6997=CARTESIAN_POINT('Ctrl Pts',(3.89620698414545,1.12244568306195,-0.476197047470731));
#6998=CARTESIAN_POINT('Ctrl Pts',(3.90948562860962,1.11817705779161,-0.477131867958273));
#6999=CARTESIAN_POINT('Ctrl Pts',(3.91897339704649,1.11499310160126,-0.477795984292783));
#7000=CARTESIAN_POINT('Ctrl Pts',(3.98514384102471,1.091844767732,-0.482408409744347));
#7001=CARTESIAN_POINT('Ctrl Pts',(4.04027356919942,1.06768592028281,-0.486153969788257));
#7002=CARTESIAN_POINT('Ctrl Pts',(4.15217776266215,1.00806321493159,-0.494010707439357));
#7003=CARTESIAN_POINT('Ctrl Pts',(4.20825882092962,0.97176574458282,-0.498106439889093));
#7004=CARTESIAN_POINT('Ctrl Pts',(4.28805197415633,0.909927378667701,-0.504525166683664));
#7005=CARTESIAN_POINT('Ctrl Pts',(4.31420696825961,0.887765542050408,-0.506737278164688));
#7006=CARTESIAN_POINT('Ctrl Pts',(4.34639021875562,0.857989388569559,-0.509626861940493));
#7007=CARTESIAN_POINT('Ctrl Pts',(4.35334363115579,0.851396744220246,-0.510261778919031));
#7008=CARTESIAN_POINT('Ctrl Pts',(4.36448437209197,0.840572841911628,-0.511296905029968));
#7009=CARTESIAN_POINT('Ctrl Pts',(4.36872151338084,0.836393303262204,-0.511694893988918));
#7010=CARTESIAN_POINT('Ctrl Pts',(4.37680070983434,0.828302206327701,-0.512462202262385));
#7011=CARTESIAN_POINT('Ctrl Pts',(4.38064749464227,0.824395572996321,-0.512831300815088));
#7012=CARTESIAN_POINT('Ctrl Pts',(4.38940075071394,0.81538108900083,-0.513679938728911));
#7013=CARTESIAN_POINT('Ctrl Pts',(4.39428866383154,0.810255594853679,-0.514160255500975));
#7014=CARTESIAN_POINT('Ctrl Pts',(4.40972840918327,0.793770192559621,-0.51569838948932));
#7015=CARTESIAN_POINT('Ctrl Pts',(4.42010190722888,0.78224627789502,-0.51676359295647));
#7016=CARTESIAN_POINT('Ctrl Pts',(4.48166067154539,0.711084131588965,-0.523284831203735));
#7017=CARTESIAN_POINT('Ctrl Pts',(4.52698958881951,0.646660128206376,-0.528972840683664));
#7018=CARTESIAN_POINT('Ctrl Pts',(4.58063723111642,0.55146263956364,-0.536986904800494));
#7019=CARTESIAN_POINT('Ctrl Pts',(4.59466180221519,0.524129670224106,-0.539244801603902));
#7020=CARTESIAN_POINT('Ctrl Pts',(4.62582731742985,0.457055876131071,-0.544648874078153));
#7021=CARTESIAN_POINT('Ctrl Pts',(4.64187994411099,0.41685364128635,-0.547777892581808));
#7022=CARTESIAN_POINT('Ctrl Pts',(4.65870084738575,0.366901133812908,-0.551467533879394));
#7023=CARTESIAN_POINT('Ctrl Pts',(4.66160840478246,0.357910368093936,-0.552123953663679));
#7024=CARTESIAN_POINT('Ctrl Pts',(4.66563373195058,0.344931761392496,-0.553059604024824));
#7025=CARTESIAN_POINT('Ctrl Pts',(4.66683907897295,0.340971773765715,-0.553343501177967));
#7026=CARTESIAN_POINT('Ctrl Pts',(4.66890202637153,0.334063738627193,-0.553835893272591));
#7027=CARTESIAN_POINT('Ctrl Pts',(4.6697690136202,0.331118573035162,-0.554044916310924));
#7028=CARTESIAN_POINT('Ctrl Pts',(4.67158485287182,0.324859908421564,-0.55448715960361));
#7029=CARTESIAN_POINT('Ctrl Pts',(4.6725306843868,0.321545609897299,-0.554720208152433));
#7030=CARTESIAN_POINT('Ctrl Pts',(4.67507453731076,0.312481065988549,-0.55535459459021));
#7031=CARTESIAN_POINT('Ctrl Pts',(4.67664344889033,0.306722654088504,-0.555754314351022));
#7032=CARTESIAN_POINT('Ctrl Pts',(4.6840146438666,0.278833834727577,-0.557675483197943));
#7033=CARTESIAN_POINT('Ctrl Pts',(4.68921546584654,0.256547829257607,-0.559166021673699));
#7034=CARTESIAN_POINT('Ctrl Pts',(4.69810206960813,0.212736119415637,-0.562034746814394));
#7035=CARTESIAN_POINT('Ctrl Pts',(4.70184502825559,0.191232006465518,-0.563414369590088));
#7036=CARTESIAN_POINT('Ctrl Pts',(4.70752387192921,0.152215855588442,-0.565885781010491));
#7037=CARTESIAN_POINT('Ctrl Pts',(4.7096684962859,0.134741342067537,-0.56698129657522));
#7038=CARTESIAN_POINT('Ctrl Pts',(4.71594649039535,0.0719800575475563,-0.570894290312237));
#7039=CARTESIAN_POINT('Ctrl Pts',(4.71784827121885,0.0265114797234634,-0.573690378143538));
#7040=CARTESIAN_POINT('Ctrl Pts',(4.71650227169159,-0.0571191282781658,
-0.578906926547529));
#7041=CARTESIAN_POINT('Ctrl Pts',(4.71403297465736,-0.0952302136696254,
-0.581312175056079));
#7042=CARTESIAN_POINT('Ctrl Pts',(4.70788339535222,-0.149275404393393,-0.584811784472708));
#7043=CARTESIAN_POINT('Ctrl Pts',(4.70571583456706,-0.165358431795092,-0.58586437571251));
#7044=CARTESIAN_POINT('Ctrl Pts',(4.70125253548774,-0.193992331123487,-0.587761823873281));
#7045=CARTESIAN_POINT('Ctrl Pts',(4.6990838141625,-0.20656053091543,-0.588602789459792));
#7046=CARTESIAN_POINT('Ctrl Pts',(4.69547962840132,-0.225597110364337,-0.589890082476426));
#7047=CARTESIAN_POINT('Ctrl Pts',(4.69419293172453,-0.232092953088178,-0.590331747844263));
#7048=CARTESIAN_POINT('Ctrl Pts',(4.6918603532172,-0.243369115781755,-0.591102773523019));
#7049=CARTESIAN_POINT('Ctrl Pts',(4.69083932284629,-0.248154455357563,-0.591431342633003));
#7050=CARTESIAN_POINT('Ctrl Pts',(4.68847809289501,-0.258892667519622,-0.592171783331215));
#7051=CARTESIAN_POINT('Ctrl Pts',(4.68712139893248,-0.264841729811598,-0.592584168749194));
#7052=CARTESIAN_POINT('Ctrl Pts',(4.68335143216703,-0.280799835578068,-0.593696368411557));
#7053=CARTESIAN_POINT('Ctrl Pts',(4.68085308396306,-0.290788028271361,-0.594398860754467));
#7054=CARTESIAN_POINT('Ctrl Pts',(4.66840246174506,-0.337930068216015,-0.597745607004141));
#7055=CARTESIAN_POINT('Ctrl Pts',(4.65676599167903,-0.374610709816397,-0.600442869794084));
#7056=CARTESIAN_POINT('Ctrl Pts',(4.61362254365121,-0.49058057471665,-0.609277032799512));
#7057=CARTESIAN_POINT('Ctrl Pts',(4.57529581940955,-0.567037343307796,-0.615598918979071));
#7058=CARTESIAN_POINT('Ctrl Pts',(4.51376099914961,-0.6623771644089,-0.623864569175167));
#7059=CARTESIAN_POINT('Ctrl Pts',(4.49761528903258,-0.685523662817829,-0.625902280730524));
#7060=CARTESIAN_POINT('Ctrl Pts',(4.47084046085439,-0.721111555270641,-0.629061290942799));
#7061=CARTESIAN_POINT('Ctrl Pts',(4.46075738582872,-0.733949208377229,-0.63020645131707));
#7062=CARTESIAN_POINT('Ctrl Pts',(4.44717374462461,-0.750522540988549,-0.631687978243776));
#7063=CARTESIAN_POINT('Ctrl Pts',(4.44391167162935,-0.754450208788329,-0.632039316911165));
#7064=CARTESIAN_POINT('Ctrl Pts',(4.43852762352065,-0.760847717138629,-0.632611804106465));
#7065=CARTESIAN_POINT('Ctrl Pts',(4.43642080713561,-0.763330140005019,-0.632833999941227));
#7066=CARTESIAN_POINT('Ctrl Pts',(4.43227345035486,-0.768176016964517,-0.633267794733483));
#7067=CARTESIAN_POINT('Ctrl Pts',(4.43023376428372,-0.770540142079035,-0.633479448804152));
#7068=CARTESIAN_POINT('Ctrl Pts',(4.42564335643877,-0.775818131432801,-0.63395209499033));
#7069=CARTESIAN_POINT('Ctrl Pts',(4.42308759398128,-0.778727608768272,-0.634212723749121));
#7070=CARTESIAN_POINT('Ctrl Pts',(4.41412724539791,-0.788827155643087,-0.635117946746003));
#7071=CARTESIAN_POINT('Ctrl Pts',(4.40764866721918,-0.795951480441159,-0.6357574148211));
#7072=CARTESIAN_POINT('Ctrl Pts',(4.35039150495479,-0.857384823221027,-0.641288075319325));
#7073=CARTESIAN_POINT('Ctrl Pts',(4.29465593472954,-0.906859588682673,-0.645863027935886));
#7074=CARTESIAN_POINT('Ctrl Pts',(4.18883333671004,-0.984227075975733,-0.653971699055674));
#7075=CARTESIAN_POINT('Ctrl Pts',(4.1406921550285,-1.01434818011597,-0.657483292085759));
#7076=CARTESIAN_POINT('Ctrl Pts',(4.08644946351141,-1.04306468112501,-0.661398375850873));
#7077=CARTESIAN_POINT('Ctrl Pts',(4.08231563063612,-1.0452218303879,-0.661696462973669));
#7078=CARTESIAN_POINT('Ctrl Pts',(4.0781692670594,-1.04735428896699,-0.661995228290505));
#7079=CARTESIAN_POINT('Origin',(3.53951905042299,8.32667268468867E-16,0.924367114736157));
#7080=CARTESIAN_POINT('',(4.07816926864924,-1.04735428814934,-1.26060176719249));
#7081=CARTESIAN_POINT('',(4.07816919733398,-1.04735432482649,-1.16244574507018));
#7082=CARTESIAN_POINT('',(4.07816926754759,-1.04735428871592,0.924367114736157));
#7083=CARTESIAN_POINT('',(2.36176946686129,0.00104026961872179,-0.924219816937961));
#7084=CARTESIAN_POINT('Ctrl Pts',(4.07816926864928,-1.04735428814932,-1.26060176719248));
#7085=CARTESIAN_POINT('Ctrl Pts',(4.08884795112987,-1.04186228347275,-1.25975288411232));
#7086=CARTESIAN_POINT('Ctrl Pts',(4.09944307827394,-1.03620673564027,-1.25891107276242));
#7087=CARTESIAN_POINT('Ctrl Pts',(4.11519672246416,-1.02748539330295,-1.25766203314466));
#7088=CARTESIAN_POINT('Ctrl Pts',(4.12042046061093,-1.02454115143288,-1.2572483069518));
#7089=CARTESIAN_POINT('Ctrl Pts',(4.12864847716065,-1.01982045416298,-1.2565976088512));
#7090=CARTESIAN_POINT('Ctrl Pts',(4.13166764964849,-1.01807036957726,-1.25635905167481));
#7091=CARTESIAN_POINT('Ctrl Pts',(4.13705697346545,-1.01491432481657,-1.25593365434014));
#7092=CARTESIAN_POINT('Ctrl Pts',(4.13942996186064,-1.01351347043171,-1.2557465043161));
#7093=CARTESIAN_POINT('Ctrl Pts',(4.14514400029037,-1.01011318281524,-1.25529620888823));
#7094=CARTESIAN_POINT('Ctrl Pts',(4.14848007859398,-1.00810549510168,-1.25503359514105));
#7095=CARTESIAN_POINT('Ctrl Pts',(4.15873503059597,-1.00186447308904,-1.25422702027125));
#7096=CARTESIAN_POINT('Ctrl Pts',(4.16562035291837,-0.997576072549032,-1.25368644513071));
#7097=CARTESIAN_POINT('Ctrl Pts',(4.18163001027191,-0.987373682438825,-1.25243043940545));
#7098=CARTESIAN_POINT('Ctrl Pts',(4.19071797727802,-0.981403713912158,-1.25171818050059));
#7099=CARTESIAN_POINT('Ctrl Pts',(4.22271767898707,-0.959742560384,-1.24920789715573));
#7100=CARTESIAN_POINT('Ctrl Pts',(4.24515696836875,-0.943367102041331,-1.24744316341442));
#7101=CARTESIAN_POINT('Ctrl Pts',(4.33212015627507,-0.875063270520032,-1.24049681309479));
#7102=CARTESIAN_POINT('Ctrl Pts',(4.39166649172802,-0.817188843989751,-1.23547825870419));
#7103=CARTESIAN_POINT('Ctrl Pts',(4.47095738287137,-0.721947483790242,-1.22765703468779));
#7104=CARTESIAN_POINT('Ctrl Pts',(4.49558851591988,-0.688996484404309,-1.22501989220541));
#7105=CARTESIAN_POINT('Ctrl Pts',(4.52428438311081,-0.646097988347847,-1.22162545445284));
#7106=CARTESIAN_POINT('Ctrl Pts',(4.53000672564423,-0.637290769255301,-1.22093059921813));
#7107=CARTESIAN_POINT('Ctrl Pts',(4.5388925251133,-0.62320587264089,-1.21982192172754));
#7108=CARTESIAN_POINT('Ctrl Pts',(4.54213381874223,-0.61797777106771,-1.21941094922122));
#7109=CARTESIAN_POINT('Ctrl Pts',(4.54787951211164,-0.608545957762582,-1.21867039410471));
#7110=CARTESIAN_POINT('Ctrl Pts',(4.55039896882165,-0.604351547319281,-1.21834136603355));
#7111=CARTESIAN_POINT('Ctrl Pts',(4.55624022542853,-0.594488254417214,-1.21756828356612));
#7112=CARTESIAN_POINT('Ctrl Pts',(4.55954084055412,-0.588807079593249,-1.21712348310464));
#7113=CARTESIAN_POINT('Ctrl Pts',(4.56897167690826,-0.572256989612077,-1.21582894457913));
#7114=CARTESIAN_POINT('Ctrl Pts',(4.57497675539408,-0.56131817429893,-1.21497483021721));
#7115=CARTESIAN_POINT('Ctrl Pts',(4.58817918015679,-0.536335687474715,-1.21302688024825));
#7116=CARTESIAN_POINT('Ctrl Pts',(4.595270236266,-0.522238863020427,-1.21192959816084));
#7117=CARTESIAN_POINT('Ctrl Pts',(4.61784886756158,-0.475012747859351,-1.20825892419414));
#7118=CARTESIAN_POINT('Ctrl Pts',(4.63207555035815,-0.441307335297537,-1.20564695497923));
#7119=CARTESIAN_POINT('Ctrl Pts',(4.6710422019801,-0.335494373439686,-1.19748686334835));
#7120=CARTESIAN_POINT('Ctrl Pts',(4.69037134943595,-0.261609072522471,-1.19183179675652));
#7121=CARTESIAN_POINT('Ctrl Pts',(4.70764347429664,-0.153838635619794,-1.18392967186133));
#7122=CARTESIAN_POINT('Ctrl Pts',(4.71149091838431,-0.121092414616739,-1.18157556512381));
#7123=CARTESIAN_POINT('Ctrl Pts',(4.71445082571294,-0.0816904289252436,
-1.178829954803));
#7124=CARTESIAN_POINT('Ctrl Pts',(4.71488717004093,-0.075151786817161,-1.1783771993553));
#7125=CARTESIAN_POINT('Ctrl Pts',(4.71547957795118,-0.0649998120297619,
-1.17767904085047));
#7126=CARTESIAN_POINT('Ctrl Pts',(4.71567360456513,-0.0613889527771861,
-1.17743165989542));
#7127=CARTESIAN_POINT('Ctrl Pts',(4.7160003789219,-0.0547358934510776,-1.17697765833948));
#7128=CARTESIAN_POINT('Ctrl Pts',(4.71613795973825,-0.0516940709573712,
-1.17677078665699));
#7129=CARTESIAN_POINT('Ctrl Pts',(4.71642409023076,-0.0447733882341851,
-1.17630168584423));
#7130=CARTESIAN_POINT('Ctrl Pts',(4.71656526284452,-0.0408943018009075,
-1.1760398637126));
#7131=CARTESIAN_POINT('Ctrl Pts',(4.71694023791755,-0.0289690156196302,
-1.1752381786659));
#7132=CARTESIAN_POINT('Ctrl Pts',(4.71711073820966,-0.0209208570094207,
-1.17470164276538));
#7133=CARTESIAN_POINT('Ctrl Pts',(4.71731637295538,-0.00210600396640012,
-1.17345654817815));
#7134=CARTESIAN_POINT('Ctrl Pts',(4.71728641972372,0.00866083266957495,
-1.17275108609864));
#7135=CARTESIAN_POINT('Ctrl Pts',(4.7166575927894,0.0467795522435654,-1.17027366716793));
#7136=CARTESIAN_POINT('Ctrl Pts',(4.7152534000642,0.0741108505661698,-1.16853406868859));
#7137=CARTESIAN_POINT('Ctrl Pts',(4.70594799466925,0.181822718668806,-1.16173907383884));
#7138=CARTESIAN_POINT('Ctrl Pts',(4.69074196946906,0.261347363644654,-1.15684181768749));
#7139=CARTESIAN_POINT('Ctrl Pts',(4.65501277556173,0.380341783272286,-1.14901710279447));
#7140=CARTESIAN_POINT('Ctrl Pts',(4.64021134439091,0.42126233038003,-1.14623314512473));
#7141=CARTESIAN_POINT('Ctrl Pts',(4.61905567945612,0.470963661633562,-1.14268171743881));
#7142=CARTESIAN_POINT('Ctrl Pts',(4.61479877438006,0.480603378558655,-1.14198478224458));
#7143=CARTESIAN_POINT('Ctrl Pts',(4.60782483745484,0.495839171159651,-1.14086962188246));
#7144=CARTESIAN_POINT('Ctrl Pts',(4.60519176510714,0.501473230529509,-1.14045424125655));
#7145=CARTESIAN_POINT('Ctrl Pts',(4.60017698667964,0.51198561790892,-1.139673418825));
#7146=CARTESIAN_POINT('Ctrl Pts',(4.59780592380346,0.516868864056127,-1.13930834903681));
#7147=CARTESIAN_POINT('Ctrl Pts',(4.59241986697501,0.527769103055894,-1.13848805697374));
#7148=CARTESIAN_POINT('Ctrl Pts',(4.58938690629979,0.533776954900184,-1.13803222430838));
#7149=CARTESIAN_POINT('Ctrl Pts',(4.58022320932044,0.551548625258632,-1.13667255906125));
#7150=CARTESIAN_POINT('Ctrl Pts',(4.57394520746903,0.563234882683309,-1.13576364649318));
#7151=CARTESIAN_POINT('Ctrl Pts',(4.5591461509936,0.589700438411027,-1.13367026644052));
#7152=CARTESIAN_POINT('Ctrl Pts',(4.55049884911401,0.604405349571571,-1.13248156382093));
#7153=CARTESIAN_POINT('Ctrl Pts',(4.51988697862427,0.653965498300141,-1.12838601100008));
#7154=CARTESIAN_POINT('Ctrl Pts',(4.49641641669209,0.687850989738129,-1.12543000807355));
#7155=CARTESIAN_POINT('Ctrl Pts',(4.43458296076068,0.767817114527967,-1.11808284254597));
#7156=CARTESIAN_POINT('Ctrl Pts',(4.39438497274184,0.812333959056298,-1.11365697335322));
#7157=CARTESIAN_POINT('Ctrl Pts',(4.32095919913548,0.882134712442782,-1.10627655920687));
#7158=CARTESIAN_POINT('Ctrl Pts',(4.28945415198576,0.909070111109058,-1.10329597032964));
#7159=CARTESIAN_POINT('Ctrl Pts',(4.25158784824816,0.938132657152573,-1.09997561112915));
#7160=CARTESIAN_POINT('Ctrl Pts',(4.24655277121828,0.94193321273168,-1.09953918000978));
#7161=CARTESIAN_POINT('Ctrl Pts',(4.23835632942023,0.948017259257392,-1.09883721114766));
#7162=CARTESIAN_POINT('Ctrl Pts',(4.23521381459628,0.950325766548631,-1.09857006738864));
#7163=CARTESIAN_POINT('Ctrl Pts',(4.22959599088233,0.954409847819512,-1.09809611642698));
#7164=CARTESIAN_POINT('Ctrl Pts',(4.22712520172596,0.956191467632653,-1.09788890691474));
#7165=CARTESIAN_POINT('Ctrl Pts',(4.22171725593542,0.960059190142491,-1.09743808436597));
#7166=CARTESIAN_POINT('Ctrl Pts',(4.21877742632116,0.962141413630804,-1.09719473082735));
#7167=CARTESIAN_POINT('Ctrl Pts',(4.21036072166443,0.968044994940203,-1.09650275833733));
#7168=CARTESIAN_POINT('Ctrl Pts',(4.20486072817006,0.971833379282359,-1.09605627763682));
#7169=CARTESIAN_POINT('Ctrl Pts',(4.16532450987109,0.99857287087287,-1.09288495886974));
#7170=CARTESIAN_POINT('Ctrl Pts',(4.13013703862062,1.01978009316341,-1.0902627021538));
#7171=CARTESIAN_POINT('Ctrl Pts',(4.02059690305597,1.07822255841859,-1.08246415829892));
#7172=CARTESIAN_POINT('Ctrl Pts',(3.94335074039314,1.10946850957014,-1.07742869781916));
#7173=CARTESIAN_POINT('Ctrl Pts',(3.82424205071352,1.14354343260029,-1.06960771180223));
#7174=CARTESIAN_POINT('Ctrl Pts',(3.7844741733988,1.15271644836675,-1.06699085748781));
#7175=CARTESIAN_POINT('Ctrl Pts',(3.73399183295129,1.16163043172554,-1.06361916061123));
#7176=CARTESIAN_POINT('Ctrl Pts',(3.72364648431919,1.16331509039633,-1.06292569422328));
#7177=CARTESIAN_POINT('Ctrl Pts',(3.70720086146154,1.16576826799626,-1.06181872387096));
#7178=CARTESIAN_POINT('Ctrl Pts',(3.701114520593,1.16662750954324,-1.06140805440622));
#7179=CARTESIAN_POINT('Ctrl Pts',(3.6901711465152,1.16808516599541,-1.06066776050874));
#7180=CARTESIAN_POINT('Ctrl Pts',(3.6853165484873,1.16870102994563,-1.06033868814949));
#7181=CARTESIAN_POINT('Ctrl Pts',(3.6739289004707,1.17007363331048,-1.05956512901717));
#7182=CARTESIAN_POINT('Ctrl Pts',(3.66739312512786,1.17080593316937,-1.05911989315564));
#7183=CARTESIAN_POINT('Ctrl Pts',(3.64840915902149,1.17277213627095,-1.05782280963187));
#7184=CARTESIAN_POINT('Ctrl Pts',(3.63594733911074,1.17386247218179,-1.05696655910112));
#7185=CARTESIAN_POINT('Ctrl Pts',(3.60768287382204,1.17588234578086,-1.05501297730987));
#7186=CARTESIAN_POINT('Ctrl Pts',(3.59187437200674,1.17669217596267,-1.05391217068112));
#7187=CARTESIAN_POINT('Ctrl Pts',(3.53933115594105,1.1783229462667,-1.05022550907506));
#7188=CARTESIAN_POINT('Ctrl Pts',(3.50257740621707,1.17774355232101,-1.04760070287487));
#7189=CARTESIAN_POINT('Ctrl Pts',(3.37890368063003,1.1699992292326,-1.03863167166116));
#7190=CARTESIAN_POINT('Ctrl Pts',(3.29277243021401,1.15490730394646,-1.03213444644967));
#7191=CARTESIAN_POINT('Ctrl Pts',(3.18712775935599,1.12402817327558,-1.02424957913164));
#7192=CARTESIAN_POINT('Ctrl Pts',(3.16534833255063,1.11696705293612,-1.02263048379369));
#7193=CARTESIAN_POINT('Ctrl Pts',(3.13816112675581,1.10726806026736,-1.02062881852968));
#7194=CARTESIAN_POINT('Ctrl Pts',(3.13255052480449,1.10521824229417,-1.02021680184776));
#7195=CARTESIAN_POINT('Ctrl Pts',(3.12372418742472,1.10191723695001,-1.01957058667346));
#7196=CARTESIAN_POINT('Ctrl Pts',(3.12049803361439,1.10069448687127,-1.0193347992979));
#7197=CARTESIAN_POINT('Ctrl Pts',(3.11440902885289,1.09835603157603,-1.01889062221534));
#7198=CARTESIAN_POINT('Ctrl Pts',(3.11154519187073,1.09724330900908,-1.01868207578175));
#7199=CARTESIAN_POINT('Ctrl Pts',(3.10497402927931,1.09466049142576,-1.01820434534152));
#7200=CARTESIAN_POINT('Ctrl Pts',(3.10126977782375,1.09318275833218,-1.01793561444452));
#7201=CARTESIAN_POINT('Ctrl Pts',(3.08937698475657,1.08836821324169,-1.01707445538923));
#7202=CARTESIAN_POINT('Ctrl Pts',(3.08121825743751,1.08495789848586,-1.01648616504898));
#7203=CARTESIAN_POINT('Ctrl Pts',(3.06177900535324,1.07657395207362,-1.01508866675573));
#7204=CARTESIAN_POINT('Ctrl Pts',(3.05053645061148,1.07151438070504,-1.01428384251026));
#7205=CARTESIAN_POINT('Ctrl Pts',(3.00885761720949,1.0519646915953,-1.01130546228494));
#7206=CARTESIAN_POINT('Ctrl Pts',(2.97896655476766,1.03634574503722,-1.00917987662706));
#7207=CARTESIAN_POINT('Ctrl Pts',(2.87534315230949,0.976402263300304,-1.00170891578259));
#7208=CARTESIAN_POINT('Ctrl Pts',(2.80584508500041,0.925317956202571,-0.996486589639262));
#7209=CARTESIAN_POINT('Ctrl Pts',(2.71968922318595,0.846130254695397,-0.989024600020789));
#7210=CARTESIAN_POINT('Ctrl Pts',(2.69769006547169,0.824245747744154,-0.987018124268657));
#7211=CARTESIAN_POINT('Ctrl Pts',(2.67005203494809,0.794489916749034,-0.984341848377458));
#7212=CARTESIAN_POINT('Ctrl Pts',(2.66360872696786,0.787380603729084,-0.983706120536616));
#7213=CARTESIAN_POINT('Ctrl Pts',(2.65330930448196,0.775733712432191,-0.982670069010851));
#7214=CARTESIAN_POINT('Ctrl Pts',(2.64939939348282,0.771244125119865,-0.982271975383961));
#7215=CARTESIAN_POINT('Ctrl Pts',(2.64195605353233,0.762565251221382,-0.98150473875416));
#7216=CARTESIAN_POINT('Ctrl Pts',(2.63841748898215,0.758380557494087,-0.981135818492017));
#7217=CARTESIAN_POINT('Ctrl Pts',(2.63030099649412,0.748645016636396,-0.98027978480689));
#7218=CARTESIAN_POINT('Ctrl Pts',(2.62574451257208,0.743076658578565,-0.979791829861827));
#7219=CARTESIAN_POINT('Ctrl Pts',(2.6120440622931,0.726017123307341,-0.978301688268817));
#7220=CARTESIAN_POINT('Ctrl Pts',(2.60306403609447,0.71439673105362,-0.977293140060038));
#7221=CARTESIAN_POINT('Ctrl Pts',(2.56154769446888,0.658545312257499,-0.972473957855018));
#7222=CARTESIAN_POINT('Ctrl Pts',(2.53191772962496,0.612248279629675,-0.968556722359695));
#7223=CARTESIAN_POINT('Ctrl Pts',(2.48286177121569,0.522331306975943,-0.961114368891997));
#7224=CARTESIAN_POINT('Ctrl Pts',(2.46264374027178,0.479263915643639,-0.957614792665407));
#7225=CARTESIAN_POINT('Ctrl Pts',(2.42508185818727,0.384780924418095,-0.950166755605304));
#7226=CARTESIAN_POINT('Ctrl Pts',(2.40857045909484,0.33314154948456,-0.946231809080753));
#7227=CARTESIAN_POINT('Ctrl Pts',(2.39413750361668,0.274294685758456,-0.942015416507684));
#7228=CARTESIAN_POINT('Ctrl Pts',(2.39265603166628,0.26803298901159,-0.941570121254137));
#7229=CARTESIAN_POINT('Ctrl Pts',(2.39035096761227,0.257921068263755,-0.940856757402183));
#7230=CARTESIAN_POINT('Ctrl Pts',(2.38949525802527,0.254078409262238,-0.940586999788746));
#7231=CARTESIAN_POINT('Ctrl Pts',(2.38801100115816,0.247252040633597,-0.940110226733926));
#7232=CARTESIAN_POINT('Ctrl Pts',(2.38737475537814,0.244270103091031,-0.939902789439959));
#7233=CARTESIAN_POINT('Ctrl Pts',(2.38601765345072,0.237786397172968,-0.93945356644503));
#7234=CARTESIAN_POINT('Ctrl Pts',(2.38530115700255,0.234283799817053,-0.939212025082583));
#7235=CARTESIAN_POINT('Ctrl Pts',(2.38385275711833,0.227035343721708,-0.938714410592869));
#7236=CARTESIAN_POINT('Ctrl Pts',(2.38312308943164,0.223289075332115,-0.938458460700184));
#7237=CARTESIAN_POINT('Ctrl Pts',(2.38129150428539,0.213635491159728,-0.937801938042549));
#7238=CARTESIAN_POINT('Ctrl Pts',(2.380216547132,0.207723087605955,-0.93740275386749));
#7239=CARTESIAN_POINT('Ctrl Pts',(2.36765734034256,0.135509677322557,-0.932559713736292));
#7240=CARTESIAN_POINT('Ctrl Pts',(2.3618289331582,0.0683427960735498,-0.928385095283674));
#7241=CARTESIAN_POINT('Ctrl Pts',(2.36176950948769,0.00103986859528879,
-0.924219717613382));
#7242=CARTESIAN_POINT('Ctrl Pts',(2.36176950984586,0.00104027417416537,
-0.924219742714656));
#7243=CARTESIAN_POINT('Ctrl Pts',(2.36169137254877,-0.087423102145968,-0.918744744905834));
#7244=CARTESIAN_POINT('Ctrl Pts',(2.37157967282482,-0.17560646492569,-0.913299058918513));
#7245=CARTESIAN_POINT('Ctrl Pts',(2.39344558752727,-0.271493055808622,-0.906875336705913));
#7246=CARTESIAN_POINT('Ctrl Pts',(2.39576560230082,-0.281106567316079,-0.906225880030156));
#7247=CARTESIAN_POINT('Ctrl Pts',(2.39980837696625,-0.2969794148988,-0.905143944706169));
#7248=CARTESIAN_POINT('Ctrl Pts',(2.40146234587091,-0.303255876299024,-0.904713615876211));
#7249=CARTESIAN_POINT('Ctrl Pts',(2.40480158054008,-0.315515388049364,-0.903867975787011));
#7250=CARTESIAN_POINT('Ctrl Pts',(2.40648249996904,-0.321499408072078,-0.903452814162152));
#7251=CARTESIAN_POINT('Ctrl Pts',(2.40972011665561,-0.332684388942151,-0.902672191964999));
#7252=CARTESIAN_POINT('Ctrl Pts',(2.41126556692301,-0.337888455955341,-0.902307101669647));
#7253=CARTESIAN_POINT('Ctrl Pts',(2.41480867964136,-0.349523957849553,-0.901486485428806));
#7254=CARTESIAN_POINT('Ctrl Pts',(2.41682562540537,-0.355949273660984,-0.901030346854788));
#7255=CARTESIAN_POINT('Ctrl Pts',(2.42210345141635,-0.372271431842001,-0.899863843113399));
#7256=CARTESIAN_POINT('Ctrl Pts',(2.425440717664,-0.382142769464095,-0.899151026909326));
#7257=CARTESIAN_POINT('Ctrl Pts',(2.45164623153488,-0.456393990929186,-0.893732255140715));
#7258=CARTESIAN_POINT('Ctrl Pts',(2.47994267163356,-0.518707723639068,-0.888847096663249));
#7259=CARTESIAN_POINT('Ctrl Pts',(2.54222202032079,-0.629223862472239,-0.879593136506329));
#7260=CARTESIAN_POINT('Ctrl Pts',(2.57473462638666,-0.678022877352781,-0.875265519245851));
#7261=CARTESIAN_POINT('Ctrl Pts',(2.62583047348316,-0.743552549334317,-0.869234744829148));
#7262=CARTESIAN_POINT('Ctrl Pts',(2.64152146788556,-0.762428819681802,-0.867469653372397));
#7263=CARTESIAN_POINT('Ctrl Pts',(2.66753834476747,-0.791808594105275,-0.864693078972203));
#7264=CARTESIAN_POINT('Ctrl Pts',(2.6774907588001,-0.802632216237684,-0.863663450222892));
#7265=CARTESIAN_POINT('Ctrl Pts',(2.69098264653742,-0.816764600931235,-0.862313199688891));
#7266=CARTESIAN_POINT('Ctrl Pts',(2.69434308600831,-0.820241448150295,-0.861980526507242));
#7267=CARTESIAN_POINT('Ctrl Pts',(2.70000965555534,-0.826032511704268,-0.861425756116281));
#7268=CARTESIAN_POINT('Ctrl Pts',(2.70230413634507,-0.828357967771663,-0.861202799993461));
#7269=CARTESIAN_POINT('Ctrl Pts',(2.7068073998265,-0.832884200240964,-0.860768537181673));
#7270=CARTESIAN_POINT('Ctrl Pts',(2.70901528694292,-0.835085793942235,-0.86055716984257));
#7271=CARTESIAN_POINT('Ctrl Pts',(2.713972488068,-0.839989760020111,-0.860085974574311));
#7272=CARTESIAN_POINT('Ctrl Pts',(2.71672640565149,-0.842687479616945,-0.859826502416486));
#7273=CARTESIAN_POINT('Ctrl Pts',(2.72633031888285,-0.852003445377359,-0.858929340455391));
#7274=CARTESIAN_POINT('Ctrl Pts',(2.73324753516953,-0.858552294193845,-0.858296658317883));
#7275=CARTESIAN_POINT('Ctrl Pts',(2.79581566704745,-0.916365238048771,-0.852684840706295));
#7276=CARTESIAN_POINT('Ctrl Pts',(2.85621489284541,-0.962246694790298,-0.848034235487393));
#7277=CARTESIAN_POINT('Ctrl Pts',(2.96814548089873,-1.03138227272268,-0.839896008093139));
#7278=CARTESIAN_POINT('Ctrl Pts',(3.01771085143064,-1.05732337115805,-0.836434060030371));
#7279=CARTESIAN_POINT('Ctrl Pts',(3.09725924760648,-1.09199659070477,-0.830896957977463));
#7280=CARTESIAN_POINT('Ctrl Pts',(3.12606448304018,-1.10322497634146,-0.828896451215516));
#7281=CARTESIAN_POINT('Ctrl Pts',(3.16380653281279,-1.11625113796333,-0.826263534660623));
#7282=CARTESIAN_POINT('Ctrl Pts',(3.1723703205623,-1.11909709212268,-0.825665389514593));
#7283=CARTESIAN_POINT('Ctrl Pts',(3.18663476751442,-1.12365615991865,-0.8246674655009));
#7284=CARTESIAN_POINT('Ctrl Pts',(3.19231732233661,-1.12542500445896,-0.824269500666078));
#7285=CARTESIAN_POINT('Ctrl Pts',(3.20325824027774,-1.12873990305329,-0.823502357645262));
#7286=CARTESIAN_POINT('Ctrl Pts',(3.20851447989547,-1.13029247265128,-0.823133401064346));
#7287=CARTESIAN_POINT('Ctrl Pts',(3.22058276062506,-1.13376575945037,-0.822285258784228));
#7288=CARTESIAN_POINT('Ctrl Pts',(3.22740160672693,-1.13566185627967,-0.821805297339097));
#7289=CARTESIAN_POINT('Ctrl Pts',(3.24919100749393,-1.14150971059971,-0.820269000508651));
#7290=CARTESIAN_POINT('Ctrl Pts',(3.26422205020613,-1.14522762542965,-0.819205299990023));
#7291=CARTESIAN_POINT('Ctrl Pts',(3.3561913221848,-1.16606097629717,-0.812670164013497));
#7292=CARTESIAN_POINT('Ctrl Pts',(3.43460161754377,-1.17571062278816,-0.806965241552146));
#7293=CARTESIAN_POINT('Ctrl Pts',(3.56029260173218,-1.17850159385758,-0.797745596129126));
#7294=CARTESIAN_POINT('Ctrl Pts',(3.60723329068936,-1.17673811478744,-0.794290943156639));
#7295=CARTESIAN_POINT('Ctrl Pts',(3.67508306737412,-1.17011475892615,-0.789363078053028));
#7296=CARTESIAN_POINT('Ctrl Pts',(3.69616308634227,-1.16747972427549,-0.787841711444709));
#7297=CARTESIAN_POINT('Ctrl Pts',(3.73039764636079,-1.16225629632423,-0.785397829837855));
#7298=CARTESIAN_POINT('Ctrl Pts',(3.74359911152947,-1.16001107900636,-0.784462014455471));
#7299=CARTESIAN_POINT('Ctrl Pts',(3.76142666009417,-1.15666530125683,-0.783209718614093));
#7300=CARTESIAN_POINT('Ctrl Pts',(3.76608798882877,-1.1557612748534,-0.782883350487185));
#7301=CARTESIAN_POINT('Ctrl Pts',(3.77386345352732,-1.15420443834303,-0.782340868071289));
#7302=CARTESIAN_POINT('Ctrl Pts',(3.77698059779126,-1.15356716277065,-0.782123907956946));
#7303=CARTESIAN_POINT('Ctrl Pts',(3.78288418319024,-1.15233527755197,-0.781714037158621));
#7304=CARTESIAN_POINT('Ctrl Pts',(3.78567110409258,-1.15174317738436,-0.781520983596849));
#7305=CARTESIAN_POINT('Ctrl Pts',(3.7922739125673,-1.15031530512018,-0.781064571896277));
#7306=CARTESIAN_POINT('Ctrl Pts',(3.79608787463899,-1.14947064384012,-0.780801708240299));
#7307=CARTESIAN_POINT('Ctrl Pts',(3.80947836718751,-1.14643514308341,-0.779881306358804));
#7308=CARTESIAN_POINT('Ctrl Pts',(3.81903193905991,-1.14414340470369,-0.779229121568934));
#7309=CARTESIAN_POINT('Ctrl Pts',(3.89633653720258,-1.12457323711456,-0.773980012266576));
#7310=CARTESIAN_POINT('Ctrl Pts',(3.96246415574902,-1.10140992798168,-0.769661003282745));
#7311=CARTESIAN_POINT('Ctrl Pts',(4.04370070732135,-1.06455025202621,-0.764142660288055));
#7312=CARTESIAN_POINT('Ctrl Pts',(4.06104457509595,-1.05616145202369,-0.762951796426201));
#7313=CARTESIAN_POINT('Ctrl Pts',(4.07816931162903,-1.047354266045,-0.76175719316035));
#7314=CARTESIAN_POINT('Ctrl Pts',(4.0781692670594,-1.04735428896699,-0.661995228290505));
#7315=CARTESIAN_POINT('Ctrl Pts',(4.06384449805672,-1.05472146166857,-0.663027396374779));
#7316=CARTESIAN_POINT('Ctrl Pts',(4.04937017112961,-1.06179393871798,-0.66406769041727));
#7317=CARTESIAN_POINT('Ctrl Pts',(4.02072968252284,-1.07506760891601,-0.666124908225273));
#7318=CARTESIAN_POINT('Ctrl Pts',(4.00657794537862,-1.08129088998704,-0.66714084293908));
#7319=CARTESIAN_POINT('Ctrl Pts',(3.98570657165901,-1.08998298186393,-0.668640397941914));
#7320=CARTESIAN_POINT('Ctrl Pts',(3.97908002581738,-1.09267211458824,-0.669116671298086));
#7321=CARTESIAN_POINT('Ctrl Pts',(3.96733728565307,-1.09731335625582,-0.669961166861675));
#7322=CARTESIAN_POINT('Ctrl Pts',(3.96223115113726,-1.09929046316112,-0.670328547794272));
#7323=CARTESIAN_POINT('Ctrl Pts',(3.95152332944664,-1.10335092082469,-0.671099402510311));
#7324=CARTESIAN_POINT('Ctrl Pts',(3.94591921285633,-1.10542737713696,-0.671503091308947));
#7325=CARTESIAN_POINT('Ctrl Pts',(3.93118353984429,-1.11076008967085,-0.672565346118283));
#7326=CARTESIAN_POINT('Ctrl Pts',(3.92202731489475,-1.11394634832691,-0.673226177654392));
#7327=CARTESIAN_POINT('Ctrl Pts',(3.88255610967042,-1.12713784375608,-0.676078982549639));
#7328=CARTESIAN_POINT('Ctrl Pts',(3.85188305553649,-1.13602048252598,-0.678306606130048));
#7329=CARTESIAN_POINT('Ctrl Pts',(3.72102999211968,-1.16821417866578,-0.687860298912885));
#7330=CARTESIAN_POINT('Ctrl Pts',(3.6183872022316,-1.17959531671325,-0.695527868963861));
#7331=CARTESIAN_POINT('Ctrl Pts',(3.49392431925198,-1.17706672365769,-0.704531277533278));
#7332=CARTESIAN_POINT('Ctrl Pts',(3.47226679019333,-1.17602814559389,-0.706084856838454));
#7333=CARTESIAN_POINT('Ctrl Pts',(3.43710060542435,-1.17336700816546,-0.708574448685394));
#7334=CARTESIAN_POINT('Ctrl Pts',(3.42357018593278,-1.17210732194144,-0.709524329552045));
#7335=CARTESIAN_POINT('Ctrl Pts',(3.40531674095537,-1.17008872043968,-0.710792343683378));
#7336=CARTESIAN_POINT('Ctrl Pts',(3.40057272145931,-1.16953486190257,-0.711120665498905));
#7337=CARTESIAN_POINT('Ctrl Pts',(3.3926673450815,-1.16856313742453,-0.711665577916761));
#7338=CARTESIAN_POINT('Ctrl Pts',(3.38950412782377,-1.16816127020335,-0.711883028231694));
#7339=CARTESIAN_POINT('Ctrl Pts',(3.38352194456256,-1.16737657079426,-0.712293101373884));
#7340=CARTESIAN_POINT('Ctrl Pts',(3.38070267321607,-1.16699636410948,-0.712485871540047));
#7341=CARTESIAN_POINT('Ctrl Pts',(3.37403250525875,-1.16607220646012,-0.712940852852626));
#7342=CARTESIAN_POINT('Ctrl Pts',(3.37018284094189,-1.16551938488063,-0.713202576963058));
#7343=CARTESIAN_POINT('Ctrl Pts',(3.35671972761983,-1.16351793490379,-0.714115070709402));
#7344=CARTESIAN_POINT('Ctrl Pts',(3.34712122419081,-1.16196930626575,-0.714760606893146));
#7345=CARTESIAN_POINT('Ctrl Pts',(3.26616547397237,-1.14787715250985,-0.720171052553844));
#7346=CARTESIAN_POINT('Ctrl Pts',(3.19607657484216,-1.12889076427616,-0.724636543500754));
#7347=CARTESIAN_POINT('Ctrl Pts',(3.07386342586199,-1.08333688949993,-0.732704191285957));
#7348=CARTESIAN_POINT('Ctrl Pts',(3.02112909993145,-1.05911528271416,-0.736288666416117));
#7349=CARTESIAN_POINT('Ctrl Pts',(2.95198291393492,-1.02094984151499,-0.741324442554763));
#7350=CARTESIAN_POINT('Ctrl Pts',(2.93384833753817,-1.01029708484264,-0.742678289251088));
#7351=CARTESIAN_POINT('Ctrl Pts',(2.90277187442234,-0.990904418547217,-0.745064937001914));
#7352=CARTESIAN_POINT('Ctrl Pts',(2.88970034193191,-0.982381871717211,-0.746090202802747));
#7353=CARTESIAN_POINT('Ctrl Pts',(2.87087042769946,-0.969564631657674,-0.747600847997373));
#7354=CARTESIAN_POINT('Ctrl Pts',(2.86497553909145,-0.965472735576419,-0.748078716623134));
#7355=CARTESIAN_POINT('Ctrl Pts',(2.85464807912376,-0.958163248733963,-0.74892488830745));
#7356=CARTESIAN_POINT('Ctrl Pts',(2.85019983029513,-0.954968098727821,-0.749292336592187));
#7357=CARTESIAN_POINT('Ctrl Pts',(2.84095722713426,-0.948230969574695,-0.750062179205172));
#7358=CARTESIAN_POINT('Ctrl Pts',(2.83616716465693,-0.944683394135114,-0.750464780728388));
#7359=CARTESIAN_POINT('Ctrl Pts',(2.82370884923174,-0.935309342610655,-0.751521552431347));
#7360=CARTESIAN_POINT('Ctrl Pts',(2.81608490217181,-0.929425001867218,-0.752177948352769));
#7361=CARTESIAN_POINT('Ctrl Pts',(2.78395797130701,-0.903993898601079,-0.754986295823248));
#7362=CARTESIAN_POINT('Ctrl Pts',(2.76017036639493,-0.88356823413951,-0.757172557513027));
#7363=CARTESIAN_POINT('Ctrl Pts',(2.67663884575618,-0.805842534028724,-0.765256783314842));
#7364=CARTESIAN_POINT('Ctrl Pts',(2.622167641112,-0.743241240029211,-0.771357615567682));
#7365=CARTESIAN_POINT('Ctrl Pts',(2.5448706598329,-0.63283282106341,-0.781223346798208));
#7366=CARTESIAN_POINT('Ctrl Pts',(2.51788128990069,-0.588268969840252,-0.784998270719495));
#7367=CARTESIAN_POINT('Ctrl Pts',(2.49072523848536,-0.535887082058305,-0.789102041887998));
#7368=CARTESIAN_POINT('Ctrl Pts',(2.48757916464597,-0.529684724369334,-0.78958284895361));
#7369=CARTESIAN_POINT('Ctrl Pts',(2.48286139513809,-0.520175987604878,-0.790311804809278));
#7370=CARTESIAN_POINT('Ctrl Pts',(2.48124993374357,-0.516889675028393,-0.790562264501288));
#7371=CARTESIAN_POINT('Ctrl Pts',(2.47832762263425,-0.5108591433676,-0.7910191040279));
#7372=CARTESIAN_POINT('Ctrl Pts',(2.4770120760809,-0.508117349335524,-0.791225759551085));
#7373=CARTESIAN_POINT('Ctrl Pts',(2.4740658509911,-0.501915503143293,-0.791690865530397));
#7374=CARTESIAN_POINT('Ctrl Pts',(2.47244139802913,-0.49845258276926,-0.791948937846555));
#7375=CARTESIAN_POINT('Ctrl Pts',(2.46828594927651,-0.489480804043665,-0.792613511583998));
#7376=CARTESIAN_POINT('Ctrl Pts',(2.46578052779981,-0.483960125807008,-0.793018528990502));
#7377=CARTESIAN_POINT('Ctrl Pts',(2.44923762748605,-0.446747043867711,-0.795723999814623));
#7378=CARTESIAN_POINT('Ctrl Pts',(2.43656104881631,-0.414464298927704,-0.797951814353656));
#7379=CARTESIAN_POINT('Ctrl Pts',(2.4161611494687,-0.354911134495222,-0.801929390635964));
#7380=CARTESIAN_POINT('Ctrl Pts',(2.40796255807533,-0.327833667094271,-0.803690262866974));
#7381=CARTESIAN_POINT('Ctrl Pts',(2.38846646301464,-0.253948059909044,-0.808427916813069));
#7382=CARTESIAN_POINT('Ctrl Pts',(2.37905102809295,-0.206701595100035,-0.811387699066481));
#7383=CARTESIAN_POINT('Ctrl Pts',(2.36538172610949,-0.106384593528173,-0.817719861059856));
#7384=CARTESIAN_POINT('Ctrl Pts',(2.36177966651481,-0.0533386013821922,
-0.821096818502703));
#7385=CARTESIAN_POINT('Ctrl Pts',(2.36176694100396,0.0104570720174762,-0.825289805850122));
#7386=CARTESIAN_POINT('Ctrl Pts',(2.36191040660988,0.0211482986329484,-0.825996773691546));
#7387=CARTESIAN_POINT('Ctrl Pts',(2.36236843029258,0.0380864760305374,-0.827124289206556));
#7388=CARTESIAN_POINT('Ctrl Pts',(2.36258722863895,0.044335611637442,-0.827541881960423));
#7389=CARTESIAN_POINT('Ctrl Pts',(2.3630887104801,0.0560011876736822,-0.828324563396148));
#7390=CARTESIAN_POINT('Ctrl Pts',(2.36335906826686,0.0614180140389397,-0.828689261279015));
#7391=CARTESIAN_POINT('Ctrl Pts',(2.36404586874551,0.0735015574446161,-0.82950572380842));
#7392=CARTESIAN_POINT('Ctrl Pts',(2.36448163076826,0.0801669447027157,-0.82995807455009));
#7393=CARTESIAN_POINT('Ctrl Pts',(2.36593395798388,0.0998129201257336,-0.831297402075247));
#7394=CARTESIAN_POINT('Ctrl Pts',(2.36710907778127,0.11278040919832,-0.832189235740729));
#7395=CARTESIAN_POINT('Ctrl Pts',(2.37541138509143,0.190109062418618,-0.837556130536567));
#7396=CARTESIAN_POINT('Ctrl Pts',(2.38762062974279,0.253802398273469,-0.842187646192627));
#7397=CARTESIAN_POINT('Ctrl Pts',(2.42266464211315,0.379555326406646,-0.851705799239318));
#7398=CARTESIAN_POINT('Ctrl Pts',(2.44561310265269,0.441356814852639,-0.856578300359325));
#7399=CARTESIAN_POINT('Ctrl Pts',(2.48649342933691,0.52834705120888,-0.863520453701498));
#7400=CARTESIAN_POINT('Ctrl Pts',(2.50043868614386,0.555271027494385,-0.865680197679378));
#7401=CARTESIAN_POINT('Ctrl Pts',(2.51857463403817,0.587204107457938,-0.868230899362441));
#7402=CARTESIAN_POINT('Ctrl Pts',(2.52178631641377,0.592753112095173,-0.868673714375721));
#7403=CARTESIAN_POINT('Ctrl Pts',(2.52686360051482,0.601362489549847,-0.86935976903767));
#7404=CARTESIAN_POINT('Ctrl Pts',(2.52869806961092,0.604440939776594,-0.869604883707214));
#7405=CARTESIAN_POINT('Ctrl Pts',(2.53211852103611,0.610121727728589,-0.870056769296397));
#7406=CARTESIAN_POINT('Ctrl Pts',(2.53370054920967,0.612726278385516,-0.870263773621644));
#7407=CARTESIAN_POINT('Ctrl Pts',(2.53734226971226,0.618669662859677,-0.870735763561398));
#7408=CARTESIAN_POINT('Ctrl Pts',(2.53940854878389,0.62200437069181,-0.87100032067971));
#7409=CARTESIAN_POINT('Ctrl Pts',(2.54587990940005,0.632332691975721,-0.87181908509676));
#7410=CARTESIAN_POINT('Ctrl Pts',(2.55034208928388,0.639290485563246,-0.872369756808881));
#7411=CARTESIAN_POINT('Ctrl Pts',(2.58460283914147,0.691494933514421,-0.876499249117139));
#7412=CARTESIAN_POINT('Ctrl Pts',(2.6174223945559,0.734690077843528,-0.879904942180072));
#7413=CARTESIAN_POINT('Ctrl Pts',(2.71491064449213,0.846124888822076,-0.88910799612077));
#7414=CARTESIAN_POINT('Ctrl Pts',(2.78493554889033,0.909125306547553,-0.894823258260179));
#7415=CARTESIAN_POINT('Ctrl Pts',(2.8775610485378,0.974311611141803,-0.902155332392961));
#7416=CARTESIAN_POINT('Ctrl Pts',(2.89370066749655,0.985083782634484,-0.903424134577679));
#7417=CARTESIAN_POINT('Ctrl Pts',(2.91688801648414,0.999745062323917,-0.905238981568036));
#7418=CARTESIAN_POINT('Ctrl Pts',(2.92372136057425,1.00396852238058,-0.905772853492476));
#7419=CARTESIAN_POINT('Ctrl Pts',(2.93493052200697,1.01073903744508,-0.906647302712863));
#7420=CARTESIAN_POINT('Ctrl Pts',(2.93928057915808,1.01332841012302,-0.906986345512928));
#7421=CARTESIAN_POINT('Ctrl Pts',(2.94846594288752,1.01871610198089,-0.907701669480715));
#7422=CARTESIAN_POINT('Ctrl Pts',(2.95330472474207,1.02150821576772,-0.908078161347059));
#7423=CARTESIAN_POINT('Ctrl Pts',(2.96497572562905,1.02813247862298,-0.908985548101728));
#7424=CARTESIAN_POINT('Ctrl Pts',(2.97182659520497,1.03193105235669,-0.909517613333797));
#7425=CARTESIAN_POINT('Ctrl Pts',(2.99587441125569,1.04495280433512,-0.911383616481748));
#7426=CARTESIAN_POINT('Ctrl Pts',(3.01326144961529,1.05381626288246,-0.912729933013163));
#7427=CARTESIAN_POINT('Ctrl Pts',(3.13103882273909,1.11021440999413,-0.92183642553937));
#7428=CARTESIAN_POINT('Ctrl Pts',(3.23748899173449,1.14376595067545,-0.930080065714455));
#7429=CARTESIAN_POINT('Ctrl Pts',(3.38604342108829,1.16837684160571,-0.941036663651135));
#7430=CARTESIAN_POINT('Ctrl Pts',(3.42536628638138,1.17287213541808,-0.943878359376383));
#7431=CARTESIAN_POINT('Ctrl Pts',(3.47106996531247,1.17577578450086,-0.947063210496579));
#7432=CARTESIAN_POINT('Ctrl Pts',(3.47729842939213,1.17612183518022,-0.947494697698407));
#7433=CARTESIAN_POINT('Ctrl Pts',(3.48740325408992,1.17660275629466,-0.94819029693238));
#7434=CARTESIAN_POINT('Ctrl Pts',(3.49127795050671,1.17676798890331,-0.948455969309928));
#7435=CARTESIAN_POINT('Ctrl Pts',(3.49819577274479,1.17702876686691,-0.948928330433654));
#7436=CARTESIAN_POINT('Ctrl Pts',(3.50123851863152,1.1771316548678,-0.949135410562213));
#7437=CARTESIAN_POINT('Ctrl Pts',(3.50789813417171,1.17733099431107,-0.949587140659578));
#7438=CARTESIAN_POINT('Ctrl Pts',(3.51151506676149,1.1774225793188,-0.94983152249864));
#7439=CARTESIAN_POINT('Ctrl Pts',(3.52188386560435,1.17763732288972,-0.950529499150087));
#7440=CARTESIAN_POINT('Ctrl Pts',(3.52863658062403,1.17771908414366,-0.950980896930664));
#7441=CARTESIAN_POINT('Ctrl Pts',(3.57886639929658,1.17789519262264,-0.954317570891468));
#7442=CARTESIAN_POINT('Ctrl Pts',(3.62232359078915,1.1756400930449,-0.957087661581744));
#7443=CARTESIAN_POINT('Ctrl Pts',(3.76508129985068,1.16027398363143,-0.966087390269286));
#7444=CARTESIAN_POINT('Ctrl Pts',(3.86282527951115,1.13692011861388,-0.972124422177075));
#7445=CARTESIAN_POINT('Ctrl Pts',(3.97941906442402,1.09278851738949,-0.980136753882568));
#7446=CARTESIAN_POINT('Ctrl Pts',(4.00211919111816,1.08337423817266,-0.981735261993988));
#7447=CARTESIAN_POINT('Ctrl Pts',(4.0325424193974,1.06962646314573,-0.983939374560743));
#7448=CARTESIAN_POINT('Ctrl Pts',(4.04053650888214,1.0659053955915,-0.984524447672939));
#7449=CARTESIAN_POINT('Ctrl Pts',(4.05318350688247,1.05984480038945,-0.985459871686834));
#7450=CARTESIAN_POINT('Ctrl Pts',(4.05786408793479,1.0575635183545,-0.985808229099558));
#7451=CARTESIAN_POINT('Ctrl Pts',(4.06744428067452,1.05281532310324,-0.986525782149849));
#7452=CARTESIAN_POINT('Ctrl Pts',(4.07234208507604,1.05034506962875,-0.986895086106371));
#7453=CARTESIAN_POINT('Ctrl Pts',(4.08366100012913,1.04453672662344,-0.987754374924724));
#7454=CARTESIAN_POINT('Ctrl Pts',(4.09006889919248,1.04117351804064,-0.988245222697718));
#7455=CARTESIAN_POINT('Ctrl Pts',(4.110491710607,1.03021328440735,-0.989823979759671));
#7456=CARTESIAN_POINT('Ctrl Pts',(4.12438301856667,1.02239096518677,-0.990919722137352));
#7457=CARTESIAN_POINT('Ctrl Pts',(4.15673407479203,1.00329871014212,-0.993524983590162));
#7458=CARTESIAN_POINT('Ctrl Pts',(4.17505011055746,0.99179779083554,-0.995042261847771));
#7459=CARTESIAN_POINT('Ctrl Pts',(4.27861351475689,0.922721771705734,-1.00386920464853));
#7460=CARTESIAN_POINT('Ctrl Pts',(4.35633757632152,0.854680234069028,-1.01153988794234));
#7461=CARTESIAN_POINT('Ctrl Pts',(4.4452055493561,0.753550022877049,-1.02127693373014));
#7462=CARTESIAN_POINT('Ctrl Pts',(4.46521679582857,0.728827657199198,-1.02354550196838));
#7463=CARTESIAN_POINT('Ctrl Pts',(4.4880811283507,0.698116882350186,-1.02620546000706));
#7464=CARTESIAN_POINT('Ctrl Pts',(4.49191446541519,0.69287818221052,-1.02665388379206));
#7465=CARTESIAN_POINT('Ctrl Pts',(4.49780721547107,0.684683742913695,-1.02734676236659));
#7466=CARTESIAN_POINT('Ctrl Pts',(4.49989664059119,0.681749895679036,-1.02759314994675));
#7467=CARTESIAN_POINT('Ctrl Pts',(4.50372797841694,0.676317589212855,-1.02804619575482));
#7468=CARTESIAN_POINT('Ctrl Pts',(4.50547365837579,0.673821960203314,-1.02825309748472));
#7469=CARTESIAN_POINT('Ctrl Pts',(4.50943187583426,0.668116286440486,-1.02872336065821));
#7470=CARTESIAN_POINT('Ctrl Pts',(4.51163817097607,0.664902006050303,-1.0289863061358));
#7471=CARTESIAN_POINT('Ctrl Pts',(4.51840122727407,0.654943503701617,-1.0297950818896));
#7472=CARTESIAN_POINT('Ctrl Pts',(4.5229041855042,0.648162783841992,-1.03033749881339));
#7473=CARTESIAN_POINT('Ctrl Pts',(4.56423244342651,0.584506916468017,-1.03535839404319));
#7474=CARTESIAN_POINT('Ctrl Pts',(4.59616106901539,0.524591459829858,-1.03956300181563));
#7475=CARTESIAN_POINT('Ctrl Pts',(4.656945925136,0.382148819435706,-1.04914823735399));
#7476=CARTESIAN_POINT('Ctrl Pts',(4.68213495463694,0.298508486263926,-1.05450828908948));
#7477=CARTESIAN_POINT('Ctrl Pts',(4.70061440431197,0.197945915105545,-1.06117487516569));
#7478=CARTESIAN_POINT('Ctrl Pts',(4.70306664402943,0.182980789793019,-1.06217176787215));
#7479=CARTESIAN_POINT('Ctrl Pts',(4.70623022961427,0.161025932881263,-1.06364321981611));
#7480=CARTESIAN_POINT('Ctrl Pts',(4.70716913059963,0.154070157414272,-1.06411070918958));
#7481=CARTESIAN_POINT('Ctrl Pts',(4.70872920702809,0.141677838557073,-1.0649460845104));
#7482=CARTESIAN_POINT('Ctrl Pts',(4.70937477926404,0.136244530979993,-1.06531320107108));
#7483=CARTESIAN_POINT('Ctrl Pts',(4.71064641320417,0.124865927367903,-1.06608390385087));
#7484=CARTESIAN_POINT('Ctrl Pts',(4.71126511297489,0.1189199827392,-1.06648770768215));
#7485=CARTESIAN_POINT('Ctrl Pts',(4.71276995507573,0.103303795312426,-1.06755117485564));
#7486=CARTESIAN_POINT('Ctrl Pts',(4.71358179594345,0.0936270216496876,-1.06821311621246));
#7487=CARTESIAN_POINT('Ctrl Pts',(4.71682358635542,0.0482584481335576,-1.07133113253047));
#7488=CARTESIAN_POINT('Ctrl Pts',(4.71774593736107,0.0124813294471392,-1.07383297825155));
#7489=CARTESIAN_POINT('Ctrl Pts',(4.71579391959372,-0.0862564181600668,
-1.08085981367337));
#7490=CARTESIAN_POINT('Ctrl Pts',(4.70949870385573,-0.14902627573032,-1.08546978685763));
#7491=CARTESIAN_POINT('Ctrl Pts',(4.69610124916665,-0.222603093001959,-1.09095850334604));
#7492=CARTESIAN_POINT('Ctrl Pts',(4.69381109208111,-0.234188822147068,-1.0918250568462));
#7493=CARTESIAN_POINT('Ctrl Pts',(4.67986476110268,-0.299558289735975,-1.09672251319418));
#7494=CARTESIAN_POINT('Ctrl Pts',(4.66462292232887,-0.35251414974623,-1.10072455182986));
#7495=CARTESIAN_POINT('Ctrl Pts',(4.64352304476232,-0.410258011082909,-1.10500267434292));
#7496=CARTESIAN_POINT('Ctrl Pts',(4.6412653916238,-0.416282907906336,-1.10544793027893));
#7497=CARTESIAN_POINT('Ctrl Pts',(4.63754708349992,-0.425963606964508,-1.10616121899824));
#7498=CARTESIAN_POINT('Ctrl Pts',(4.63611731159667,-0.42963101680436,-1.1064309406418));
#7499=CARTESIAN_POINT('Ctrl Pts',(4.63354759941266,-0.436126002630176,-1.10690764507312));
#7500=CARTESIAN_POINT('Ctrl Pts',(4.6324150383126,-0.43895639484777,-1.10711504962679));
#7501=CARTESIAN_POINT('Ctrl Pts',(4.62993067814571,-0.445095855863185,-1.10756419563971));
#7502=CARTESIAN_POINT('Ctrl Pts',(4.6285747987739,-0.448403185329899,-1.10780569288453));
#7503=CARTESIAN_POINT('Ctrl Pts',(4.62469250867243,-0.457751574411895,-1.10848714239649));
#7504=CARTESIAN_POINT('Ctrl Pts',(4.62213069776714,-0.46377792557394,-1.10892505686748));
#7505=CARTESIAN_POINT('Ctrl Pts',(4.60458118792502,-0.504123092750719,-1.11184957465907));
#7506=CARTESIAN_POINT('Ctrl Pts',(4.58801259693433,-0.537735397952453,-1.11425097635191));
#7507=CARTESIAN_POINT('Ctrl Pts',(4.54437384162106,-0.616548411627288,-1.11992937868765));
#7508=CARTESIAN_POINT('Ctrl Pts',(4.51582050306904,-0.660833584906177,-1.12316207461071));
#7509=CARTESIAN_POINT('Ctrl Pts',(4.44079596979284,-0.761662882574636,-1.13094811027053));
#7510=CARTESIAN_POINT('Ctrl Pts',(4.39184172443522,-0.816072549531273,-1.13551806672366));
#7511=CARTESIAN_POINT('Ctrl Pts',(4.33048488492769,-0.872684022937023,-1.14099635606994));
#7512=CARTESIAN_POINT('Ctrl Pts',(4.3227075763017,-0.879670436455903,-1.14168640103472));
#7513=CARTESIAN_POINT('Ctrl Pts',(4.30976164617698,-0.890992083576647,-1.14282862402646));
#7514=CARTESIAN_POINT('Ctrl Pts',(4.3046468478007,-0.895388183870356,-1.14327829969705));
#7515=CARTESIAN_POINT('Ctrl Pts',(4.29534731872871,-0.903243136425282,-1.1440931759109));
#7516=CARTESIAN_POINT('Ctrl Pts',(4.29117586424519,-0.906717468243931,-1.14445773693941));
#7517=CARTESIAN_POINT('Ctrl Pts',(4.28218373983157,-0.914102155161602,-1.14524163084726));
#7518=CARTESIAN_POINT('Ctrl Pts',(4.27735589570603,-0.918003473938131,-1.14566130903841));
#7519=CARTESIAN_POINT('Ctrl Pts',(4.26407308871906,-0.928564669859278,-1.14681287562956));
#7520=CARTESIAN_POINT('Ctrl Pts',(4.25555749051845,-0.935146961443839,-1.14754777160343));
#7521=CARTESIAN_POINT('Ctrl Pts',(4.20545732399026,-0.972787290712016,-1.15185322582288));
#7522=CARTESIAN_POINT('Ctrl Pts',(4.1619520991648,-1.00118161930328,-1.15552381851881));
#7523=CARTESIAN_POINT('Ctrl Pts',(4.10399612704973,-1.0337668160214,-1.16032415327027));
#7524=CARTESIAN_POINT('Ctrl Pts',(4.09114291367256,-1.04068199432085,-1.16138314355777));
#7525=CARTESIAN_POINT('Ctrl Pts',(4.07816919733399,-1.04735432482649,-1.16244574507018));
#7526=CARTESIAN_POINT('Origin',(3.53951905042299,8.32667268468867E-16,0.924367114736157));
#7527=CARTESIAN_POINT('',(4.07816941925732,-1.04735421069218,-1.7624800269618));
#7528=CARTESIAN_POINT('',(4.07816926735968,-1.04735428881255,-1.66387346933803));
#7529=CARTESIAN_POINT('',(4.07816926754759,-1.04735428871592,0.924367114736157));
#7530=CARTESIAN_POINT('Ctrl Pts',(4.07816941925732,-1.04735421069218,-1.7624800269618));
#7531=CARTESIAN_POINT('Ctrl Pts',(4.12402156783836,-1.02377262149066,-1.75884119833188));
#7532=CARTESIAN_POINT('Ctrl Pts',(4.16829267925419,-0.997196752434242,-1.75510908299161));
#7533=CARTESIAN_POINT('Ctrl Pts',(4.25805127955991,-0.93494805305265,-1.74711882129328));
#7534=CARTESIAN_POINT('Ctrl Pts',(4.30293455233965,-0.898673155174069,-1.74286238740916));
#7535=CARTESIAN_POINT('Ctrl Pts',(4.36006044211788,-0.845123661458328,-1.73720682626097));
#7536=CARTESIAN_POINT('Ctrl Pts',(4.37476471387704,-0.830594342664483,-1.73572758190825));
#7537=CARTESIAN_POINT('Ctrl Pts',(4.39817290656924,-0.806213989927964,-1.73334358094016));
#7538=CARTESIAN_POINT('Ctrl Pts',(4.40710749433009,-0.796591344546048,-1.7324262688827));
#7539=CARTESIAN_POINT('Ctrl Pts',(4.41902811922707,-0.783314157455995,-1.73119454737553));
#7540=CARTESIAN_POINT('Ctrl Pts',(4.42215548339693,-0.779788561383607,-1.73087065096255));
#7541=CARTESIAN_POINT('Ctrl Pts',(4.42735371647312,-0.773857056213299,-1.73033114347868));
#7542=CARTESIAN_POINT('Ctrl Pts',(4.42943614610039,-0.771461406217131,-1.73011470556488));
#7543=CARTESIAN_POINT('Ctrl Pts',(4.43337316642583,-0.766895059733491,-1.72970496766419));
#7544=CARTESIAN_POINT('Ctrl Pts',(4.43522958442939,-0.764725998675945,-1.72951153029195));
#7545=CARTESIAN_POINT('Ctrl Pts',(4.43962293930561,-0.759554803873737,-1.72905312696225));
#7546=CARTESIAN_POINT('Ctrl Pts',(4.44215279157775,-0.756546655069034,-1.72878866605188));
#7547=CARTESIAN_POINT('Ctrl Pts',(4.45104599166755,-0.745863986304985,-1.72785700877703));
#7548=CARTESIAN_POINT('Ctrl Pts',(4.45732711979027,-0.738121138150766,-1.72719533937084));
#7549=CARTESIAN_POINT('Ctrl Pts',(4.50346225542457,-0.679749961319573,-1.7222996377087));
#7550=CARTESIAN_POINT('Ctrl Pts',(4.53920515782283,-0.626000329528692,-1.71830009188633));
#7551=CARTESIAN_POINT('Ctrl Pts',(4.60005295353438,-0.515876746269686,-1.71051268168533));
#7552=CARTESIAN_POINT('Ctrl Pts',(4.62548652708865,-0.459929402292148,-1.7067343796029));
#7553=CARTESIAN_POINT('Ctrl Pts',(4.65848727668399,-0.369118359268179,-1.70059779161538));
#7554=CARTESIAN_POINT('Ctrl Pts',(4.66903463489072,-0.335458531143566,-1.69832372923198));
#7555=CARTESIAN_POINT('Ctrl Pts',(4.68052969360066,-0.292032938681058,-1.69536391229397));
#7556=CARTESIAN_POINT('Ctrl Pts',(4.68288834355618,-0.282657346423455,-1.69472342820524));
#7557=CARTESIAN_POINT('Ctrl Pts',(4.68651621840781,-0.267447550340622,-1.69368154173606));
#7558=CARTESIAN_POINT('Ctrl Pts',(4.6878570005195,-0.261630743028786,-1.69328241702915));
#7559=CARTESIAN_POINT('Ctrl Pts',(4.69034271350128,-0.250459454456107,-1.69251449611081));
#7560=CARTESIAN_POINT('Ctrl Pts',(4.6914946393424,-0.245106676009676,-1.69214593219876));
#7561=CARTESIAN_POINT('Ctrl Pts',(4.69404228381504,-0.232853449555932,-1.69130075239853));
#7562=CARTESIAN_POINT('Ctrl Pts',(4.69541352643238,-0.225948184367437,-1.69082337912172));
#7563=CARTESIAN_POINT('Ctrl Pts',(4.69956377094064,-0.20402126705809,-1.68930389967736));
#7564=CARTESIAN_POINT('Ctrl Pts',(4.70211236211434,-0.188958155811475,-1.68825465413436));
#7565=CARTESIAN_POINT('Ctrl Pts',(4.71689230484864,-0.0899282119012987,
-1.68131804608723));
#7566=CARTESIAN_POINT('Ctrl Pts',(4.72030932577333,-0.00491321944165487,
-1.67515549505037));
#7567=CARTESIAN_POINT('Ctrl Pts',(4.7130039623824,0.10277357668324,-1.66723486479033));
#7568=CARTESIAN_POINT('Ctrl Pts',(4.71076117480938,0.125782162099334,-1.66553769817192));
#7569=CARTESIAN_POINT('Ctrl Pts',(4.70221944697553,0.1928892962147,-1.66059222937456));
#7570=CARTESIAN_POINT('Ctrl Pts',(4.69409407948227,0.236718854694833,-1.65736698810654));
#7571=CARTESIAN_POINT('Ctrl Pts',(4.68122622746271,0.289295037690181,-1.65357697072449));
#7572=CARTESIAN_POINT('Ctrl Pts',(4.67883443609033,0.298575557605083,-1.65291107454052));
#7573=CARTESIAN_POINT('Ctrl Pts',(4.67524119513117,0.311845493205629,-1.6519643741052));
#7574=CARTESIAN_POINT('Ctrl Pts',(4.674131522781,0.315859051651586,-1.65167875891447));
#7575=CARTESIAN_POINT('Ctrl Pts',(4.67216533547617,0.322826444166616,-1.6511842930227));
#7576=CARTESIAN_POINT('Ctrl Pts',(4.67131850366377,0.3257829317743,-1.65097490277886));
#7577=CARTESIAN_POINT('Ctrl Pts',(4.66950011637425,0.332038674213376,-1.65053278261153));
#7578=CARTESIAN_POINT('Ctrl Pts',(4.66852568337388,0.335337015697624,-1.65030021836079));
#7579=CARTESIAN_POINT('Ctrl Pts',(4.66583356646529,0.344304755837359,-1.64966926988815));
#7580=CARTESIAN_POINT('Ctrl Pts',(4.66408750682879,0.349965633216039,-1.64927247032405));
#7581=CARTESIAN_POINT('Ctrl Pts',(4.6555581270602,0.37689549259379,-1.64739084734756));
#7582=CARTESIAN_POINT('Ctrl Pts',(4.6482132141992,0.397983465379435,-1.64593537569598));
#7583=CARTESIAN_POINT('Ctrl Pts',(4.63384364665159,0.435747100932546,-1.64334016055827));
#7584=CARTESIAN_POINT('Ctrl Pts',(4.62702620250074,0.452493211383162,-1.64219341864626));
#7585=CARTESIAN_POINT('Ctrl Pts',(4.61084911706903,0.489749855802069,-1.63963765582858));
#7586=CARTESIAN_POINT('Ctrl Pts',(4.60128071766576,0.510161986485313,-1.63823422661368));
#7587=CARTESIAN_POINT('Ctrl Pts',(4.55972093587499,0.592579193203745,-1.63250863585511));
#7588=CARTESIAN_POINT('Ctrl Pts',(4.52283891071328,0.651953610970371,-1.62823474923878));
#7589=CARTESIAN_POINT('Ctrl Pts',(4.46693956838103,0.726310918199653,-1.62232560530166));
#7590=CARTESIAN_POINT('Ctrl Pts',(4.45241171692637,0.744488578574955,-1.62083258294982));
#7591=CARTESIAN_POINT('Ctrl Pts',(4.42644659176075,0.775073373047359,-1.61822390401277));
#7592=CARTESIAN_POINT('Ctrl Pts',(4.41526329492532,0.78768722793614,-1.61711792090836));
#7593=CARTESIAN_POINT('Ctrl Pts',(4.39878757302733,0.805485822167764,-1.61551053875043));
#7594=CARTESIAN_POINT('Ctrl Pts',(4.39371059757371,0.810867806894958,-1.61501810984387));
#7595=CARTESIAN_POINT('Ctrl Pts',(4.38476409958284,0.820174518560993,-1.61415512696631));
#7596=CARTESIAN_POINT('Ctrl Pts',(4.38091707111418,0.824120624086463,-1.61378554052036));
#7597=CARTESIAN_POINT('Ctrl Pts',(4.37341422834849,0.831709400796884,-1.61306753254382));
#7598=CARTESIAN_POINT('Ctrl Pts',(4.36976188139756,0.835355334750929,-1.61271926654244));
#7599=CARTESIAN_POINT('Ctrl Pts',(4.35998035578412,0.844992169020553,-1.61178979408735));
#7600=CARTESIAN_POINT('Ctrl Pts',(4.35380963872326,0.85094027427078,-1.61120676282103));
#7601=CARTESIAN_POINT('Ctrl Pts',(4.33098266892604,0.872468079164142,-1.60906161114945));
#7602=CARTESIAN_POINT('Ctrl Pts',(4.31394070545571,0.887629530893936,-1.60748222245532));
#7603=CARTESIAN_POINT('Ctrl Pts',(4.21861436543652,0.967601300261546,-1.59875946098973));
#7604=CARTESIAN_POINT('Ctrl Pts',(4.13264048326198,1.02255700607095,-1.5912367982865));
#7605=CARTESIAN_POINT('Ctrl Pts',(4.01347828389879,1.0785930862681,-1.58163105591438));
#7606=CARTESIAN_POINT('Ctrl Pts',(3.98576720456792,1.09035004892502,-1.57945356177546));
#7607=CARTESIAN_POINT('Ctrl Pts',(3.9469219627294,1.10510146032129,-1.57650283524124));
#7608=CARTESIAN_POINT('Ctrl Pts',(3.93615015565345,1.10901314629823,-1.57569515093149));
#7609=CARTESIAN_POINT('Ctrl Pts',(3.91734150566344,1.11553422557838,-1.57430505373057));
#7610=CARTESIAN_POINT('Ctrl Pts',(3.90933064357695,1.11821545862779,-1.57371927910735));
#7611=CARTESIAN_POINT('Ctrl Pts',(3.89752491896508,1.12202608014478,-1.57286590499044));
#7612=CARTESIAN_POINT('Ctrl Pts',(3.89375231934396,1.12322282685655,-1.57259467676492));
#7613=CARTESIAN_POINT('Ctrl Pts',(3.88706100180845,1.12530838548232,-1.5721163017335));
#7614=CARTESIAN_POINT('Ctrl Pts',(3.8841447825356,1.12620489962643,-1.5719087221209));
#7615=CARTESIAN_POINT('Ctrl Pts',(3.87781775476554,1.12812309859558,-1.57146033365875));
#7616=CARTESIAN_POINT('Ctrl Pts',(3.87440577955913,1.12914065484973,-1.57121976095565));
#7617=CARTESIAN_POINT('Ctrl Pts',(3.86493792443298,1.13191757064232,-1.57055546566782));
#7618=CARTESIAN_POINT('Ctrl Pts',(3.85887234041032,1.13364382008187,-1.57013357843805));
#7619=CARTESIAN_POINT('Ctrl Pts',(3.82530460332513,1.14290630646632,-1.56781764691092));
#7620=CARTESIAN_POINT('Ctrl Pts',(3.79754718027202,1.14949118857355,-1.56597214837872));
#7621=CARTESIAN_POINT('Ctrl Pts',(3.66562919439549,1.17576561400528,-1.55740952463851));
#7622=CARTESIAN_POINT('Ctrl Pts',(3.5593615929637,1.18234417043931,-1.55107273857339));
#7623=CARTESIAN_POINT('Ctrl Pts',(3.43182088613601,1.17301955158421,-1.54293092883299));
#7624=CARTESIAN_POINT('Ctrl Pts',(3.41004967818746,1.17081653444504,-1.54152412013656));
#7625=CARTESIAN_POINT('Ctrl Pts',(3.37240117774762,1.16594400163605,-1.5390526761519));
#7626=CARTESIAN_POINT('Ctrl Pts',(3.35649358778646,1.16355293728631,-1.53799635541198));
#7627=CARTESIAN_POINT('Ctrl Pts',(3.33348154668428,1.15961043684511,-1.53644839662488));
#7628=CARTESIAN_POINT('Ctrl Pts',(3.32633417709084,1.1583177560671,-1.53596481569026));
#7629=CARTESIAN_POINT('Ctrl Pts',(3.31380615043783,1.15593204415302,-1.53511206084683));
#7630=CARTESIAN_POINT('Ctrl Pts',(3.30842027446222,1.15486733347588,-1.53474378558529));
#7631=CARTESIAN_POINT('Ctrl Pts',(3.29723925725165,1.15257566002025,-1.5339756800357));
#7632=CARTESIAN_POINT('Ctrl Pts',(3.29144554702594,1.15134255760537,-1.53357566561486));
#7633=CARTESIAN_POINT('Ctrl Pts',(3.27642675662717,1.14802741368854,-1.53253339315456));
#7634=CARTESIAN_POINT('Ctrl Pts',(3.26721716635233,1.14587790471841,-1.53188902120037));
#7635=CARTESIAN_POINT('Ctrl Pts',(3.2291991765614,1.13652034676396,-1.52920658546107));
#7636=CARTESIAN_POINT('Ctrl Pts',(3.20064485018686,1.12833546793783,-1.5271379560596));
#7637=CARTESIAN_POINT('Ctrl Pts',(3.09246082757994,1.09284839070095,-1.51908642499023));
#7638=CARTESIAN_POINT('Ctrl Pts',(3.01554006419951,1.05812149385582,-1.5128848914851));
#7639=CARTESIAN_POINT('Ctrl Pts',(2.897657373682,0.988874448589901,-1.50287557155424));
#7640=CARTESIAN_POINT('Ctrl Pts',(2.8541541765315,0.959236883287899,-1.4990600860629));
#7641=CARTESIAN_POINT('Ctrl Pts',(2.80729209670304,0.922489709671055,-1.49491802572919));
#7642=CARTESIAN_POINT('Ctrl Pts',(2.80184916997425,0.918143087732133,-1.49443645754283));
#7643=CARTESIAN_POINT('Ctrl Pts',(2.79360311053011,0.911437266156045,-1.49370655079394));
#7644=CARTESIAN_POINT('Ctrl Pts',(2.79077200578922,0.909112943255084,-1.49345589333044));
#7645=CARTESIAN_POINT('Ctrl Pts',(2.78560971517004,0.904834255483009,-1.49299880131462));
#7646=CARTESIAN_POINT('Ctrl Pts',(2.78327524734904,0.902884060352113,-1.49279208999418));
#7647=CARTESIAN_POINT('Ctrl Pts',(2.77802305366047,0.898461759202,-1.49232698616727));
#7648=CARTESIAN_POINT('Ctrl Pts',(2.77510979467302,0.89598447340852,-1.49206897092791));
#7649=CARTESIAN_POINT('Ctrl Pts',(2.76761311634263,0.889546505097599,-1.49140477643663));
#7650=CARTESIAN_POINT('Ctrl Pts',(2.76304802651306,0.885564514101435,-1.4910000775387));
#7651=CARTESIAN_POINT('Ctrl Pts',(2.73268080120068,0.858660725688144,-1.48830477319058));
#7652=CARTESIAN_POINT('Ctrl Pts',(2.70786355695607,0.834647136575428,-1.4860861621365));
#7653=CARTESIAN_POINT('Ctrl Pts',(2.6784630992231,0.803583093869982,-1.48338316824471));
#7654=CARTESIAN_POINT('Ctrl Pts',(2.6728545413076,0.797531048034353,-1.48286394456196));
#7655=CARTESIAN_POINT('Ctrl Pts',(2.65501060289876,0.777865591166287,-1.48119848872164));
#7656=CARTESIAN_POINT('Ctrl Pts',(2.64302862673834,0.76402553655045,-1.48005922381001));
#7657=CARTESIAN_POINT('Ctrl Pts',(2.60226028051457,0.714654945089442,-1.47608688593562));
#7658=CARTESIAN_POINT('Ctrl Pts',(2.5752248577766,0.677733251261796,-1.47327506229901));
#7659=CARTESIAN_POINT('Ctrl Pts',(2.52980832401545,0.607469216965361,-1.46805562199051));
#7660=CARTESIAN_POINT('Ctrl Pts',(2.51076539235449,0.574630464091372,-1.46566410296407));
#7661=CARTESIAN_POINT('Ctrl Pts',(2.48591578247145,0.52657060258171,-1.46218251098858));
#7662=CARTESIAN_POINT('Ctrl Pts',(2.47878702403522,0.512058566787382,-1.46113365207363));
#7663=CARTESIAN_POINT('Ctrl Pts',(2.46658769965374,0.485875661607356,-1.45924216773586));
#7664=CARTESIAN_POINT('Ctrl Pts',(2.46140321089575,0.474260538236342,-1.45840339004994));
#7665=CARTESIAN_POINT('Ctrl Pts',(2.45380809366998,0.45647628822524,-1.4571184532792));
#7666=CARTESIAN_POINT('Ctrl Pts',(2.45125959713045,0.450366786784851,-1.45667691925175));
#7667=CARTESIAN_POINT('Ctrl Pts',(2.44671774834194,0.439214949747966,-1.45587061022657));
#7668=CARTESIAN_POINT('Ctrl Pts',(2.44470744109183,0.434179682051117,-1.45550641231937));
#7669=CARTESIAN_POINT('Ctrl Pts',(2.44043520358832,0.423260552178374,-1.45471625919872));
#7670=CARTESIAN_POINT('Ctrl Pts',(2.43818561094402,0.417372075996157,-1.45428990838787));
#7671=CARTESIAN_POINT('Ctrl Pts',(2.43217166334469,0.401242902198157,-1.45312129086021));
#7672=CARTESIAN_POINT('Ctrl Pts',(2.42850224960028,0.39096771815302,-1.4523759398954));
#7673=CARTESIAN_POINT('Ctrl Pts',(2.4087606355546,0.333163278708378,-1.4481767701443));
#7674=CARTESIAN_POINT('Ctrl Pts',(2.39559781285615,0.284702182677126,-1.44463012504818));
#7675=CARTESIAN_POINT('Ctrl Pts',(2.36969404711082,0.157803112612822,-1.43528740164707));
#7676=CARTESIAN_POINT('Ctrl Pts',(2.3617224083408,0.0786523203925032,-1.42939606451052));
#7677=CARTESIAN_POINT('Ctrl Pts',(2.36178952604145,-0.0350283978066116,
-1.42115590347207));
#7678=CARTESIAN_POINT('Ctrl Pts',(2.3633110826812,-0.0693478293372115,-1.41870012363523));
#7679=CARTESIAN_POINT('Ctrl Pts',(2.36686244336644,-0.109581702054972,-1.41589288626285));
#7680=CARTESIAN_POINT('Ctrl Pts',(2.36744086055434,-0.11560444705143,-1.41547457393234));
#7681=CARTESIAN_POINT('Ctrl Pts',(2.36846034979838,-0.125424035540343,-1.41479595687285));
#7682=CARTESIAN_POINT('Ctrl Pts',(2.36887352829259,-0.129223571969174,-1.41453421033222));
#7683=CARTESIAN_POINT('Ctrl Pts',(2.36964875792967,-0.136043425957578,-1.41406597486874));
#7684=CARTESIAN_POINT('Ctrl Pts',(2.37000401958411,-0.139064403360385,-1.41385912422629));
#7685=CARTESIAN_POINT('Ctrl Pts',(2.37081311940635,-0.14572213348381,-1.41340450178702));
#7686=CARTESIAN_POINT('Ctrl Pts',(2.37127222982741,-0.149358161686565,-1.41315702336807));
#7687=CARTESIAN_POINT('Ctrl Pts',(2.37265428016482,-0.159907193152545,-1.41244121659493));
#7688=CARTESIAN_POINT('Ctrl Pts',(2.3736216803609,-0.166814360255853,-1.41197526313782));
#7689=CARTESIAN_POINT('Ctrl Pts',(2.38248084560995,-0.226221426809344,-1.40798810158194));
#7690=CARTESIAN_POINT('Ctrl Pts',(2.39385386137737,-0.278148061494531,-1.40463917024175));
#7691=CARTESIAN_POINT('Ctrl Pts',(2.4325892371466,-0.411232633154748,-1.39600968930499));
#7692=CARTESIAN_POINT('Ctrl Pts',(2.46535135532612,-0.490478444462737,-1.3908067015251));
#7693=CARTESIAN_POINT('Ctrl Pts',(2.51993512987423,-0.590201690231243,-1.38353327947164));
#7694=CARTESIAN_POINT('Ctrl Pts',(2.5343494264082,-0.614429193001555,-1.38170574176274));
#7695=CARTESIAN_POINT('Ctrl Pts',(2.55464441715308,-0.645912600656586,-1.37923546857936));
#7696=CARTESIAN_POINT('Ctrl Pts',(2.55976277795992,-0.653650341853781,-1.37862041904227));
#7697=CARTESIAN_POINT('Ctrl Pts',(2.56827614390267,-0.66619584683815,-1.37760972910029));
#7698=CARTESIAN_POINT('Ctrl Pts',(2.57161678364344,-0.671040155017402,-1.37721611655494));
#7699=CARTESIAN_POINT('Ctrl Pts',(2.57815249271537,-0.68036733234645,-1.37645163859999));
#7700=CARTESIAN_POINT('Ctrl Pts',(2.58134297108685,-0.68485324298345,-1.37608095323778));
#7701=CARTESIAN_POINT('Ctrl Pts',(2.58887202258151,-0.695283719576946,-1.37521188563698));
#7702=CARTESIAN_POINT('Ctrl Pts',(2.59323505916464,-0.701210257971917,-1.37471257891483));
#7703=CARTESIAN_POINT('Ctrl Pts',(2.60763724410199,-0.720394267844292,-1.37307799826549));
#7704=CARTESIAN_POINT('Ctrl Pts',(2.61790129612382,-0.733479562192908,-1.37193409363574));
#7705=CARTESIAN_POINT('Ctrl Pts',(2.6429217282258,-0.764022678330969,-1.36919276209822));
#7706=CARTESIAN_POINT('Ctrl Pts',(2.65791563419098,-0.781276332993568,-1.36758643508937));
#7707=CARTESIAN_POINT('Ctrl Pts',(2.71908167880184,-0.847656742967956,-1.36117275183795));
#7708=CARTESIAN_POINT('Ctrl Pts',(2.76892974071437,-0.893213128249696,-1.35623315699841));
#7709=CARTESIAN_POINT('Ctrl Pts',(2.82843086820848,-0.938885822236372,-1.3507288973519));
#7710=CARTESIAN_POINT('Ctrl Pts',(2.83451311610812,-0.943461511344577,-1.35017056792598));
#7711=CARTESIAN_POINT('Ctrl Pts',(2.88597945750959,-0.981404149145852,-1.34548407050552));
#7712=CARTESIAN_POINT('Ctrl Pts',(2.93366494064733,-1.01153863413426,-1.34138373138775));
#7713=CARTESIAN_POINT('Ctrl Pts',(2.98900271913295,-1.0411859849375,-1.3370150329672));
#7714=CARTESIAN_POINT('Ctrl Pts',(2.99470092534498,-1.04417896044123,-1.33656960734444));
#7715=CARTESIAN_POINT('Ctrl Pts',(3.00392407904516,-1.0489273525122,-1.33585607701315));
#7716=CARTESIAN_POINT('Ctrl Pts',(3.00743370054857,-1.05071201848643,-1.3355862820396));
#7717=CARTESIAN_POINT('Ctrl Pts',(3.01367704136102,-1.05384749415545,-1.33510946794191));
#7718=CARTESIAN_POINT('Ctrl Pts',(3.0164071275492,-1.05520532425152,-1.33490202669739));
#7719=CARTESIAN_POINT('Ctrl Pts',(3.02234940572972,-1.05813203318312,-1.33445282254889));
#7720=CARTESIAN_POINT('Ctrl Pts',(3.02556348326635,-1.05969689858941,-1.33421130378618));
#7721=CARTESIAN_POINT('Ctrl Pts',(3.03468490867483,-1.06408666346032,-1.33352983452817));
#7722=CARTESIAN_POINT('Ctrl Pts',(3.04060887289725,-1.06687702086005,-1.33309192167412));
#7723=CARTESIAN_POINT('Ctrl Pts',(3.08055007866884,-1.08528503352303,-1.33016858421557));
#7724=CARTESIAN_POINT('Ctrl Pts',(3.11527568093058,-1.09932447875169,-1.32776827851351));
#7725=CARTESIAN_POINT('Ctrl Pts',(3.20030478962864,-1.12907042679265,-1.32209015321045));
#7726=CARTESIAN_POINT('Ctrl Pts',(3.25110641094363,-1.14310321123864,-1.3188567341802));
#7727=CARTESIAN_POINT('Ctrl Pts',(3.37423656052095,-1.16838057105099,-1.31106954470835));
#7728=CARTESIAN_POINT('Ctrl Pts',(3.44699631956718,-1.17637958108633,-1.30649917109925));
#7729=CARTESIAN_POINT('Ctrl Pts',(3.53047489557254,-1.17776166705568,-1.30102045863125));
#7730=CARTESIAN_POINT('Ctrl Pts',(3.54092866205826,-1.17779554368283,-1.30033045772814));
#7731=CARTESIAN_POINT('Ctrl Pts',(3.55812558122246,-1.177622329282,-1.29918825891853));
#7732=CARTESIAN_POINT('Ctrl Pts',(3.56486910554612,-1.17749646493795,-1.29873856268896));
#7733=CARTESIAN_POINT('Ctrl Pts',(3.57703860877626,-1.17716474013002,-1.29792361613158));
#7734=CARTESIAN_POINT('Ctrl Pts',(3.58246498948656,-1.17697926374947,-1.29755900517698));
#7735=CARTESIAN_POINT('Ctrl Pts',(3.59409309806293,-1.1765012883705,-1.29677496667228));
#7736=CARTESIAN_POINT('Ctrl Pts',(3.60029416096478,-1.1761972587982,-1.29635519344792));
#7737=CARTESIAN_POINT('Ctrl Pts',(3.61724166762075,-1.17523196784924,-1.29520326709841));
#7738=CARTESIAN_POINT('Ctrl Pts',(3.62798168351054,-1.17447236352397,-1.29446810381238));
#7739=CARTESIAN_POINT('Ctrl Pts',(3.6904854325951,-1.16918951173482,-1.29015833817254));
#7740=CARTESIAN_POINT('Ctrl Pts',(3.74190759125941,-1.16139247237629,-1.28648346484916));
#7741=CARTESIAN_POINT('Ctrl Pts',(3.86495100312061,-1.13431523204402,-1.27738696469821));
#7742=CARTESIAN_POINT('Ctrl Pts',(3.93559803864069,-1.11161926810425,-1.27189983064239));
#7743=CARTESIAN_POINT('Ctrl Pts',(4.01785602921749,-1.07634940325568,-1.26539391958374));
#7744=CARTESIAN_POINT('Ctrl Pts',(4.03195083345737,-1.06997442715185,-1.26427535331562));
#7745=CARTESIAN_POINT('Ctrl Pts',(4.05674825621073,-1.05816489756866,-1.26230502090634));
#7746=CARTESIAN_POINT('Ctrl Pts',(4.06750046289602,-1.05284121326361,-1.26144986513958));
#7747=CARTESIAN_POINT('Ctrl Pts',(4.07816926864928,-1.04735428814932,-1.26060176719248));
#7748=CARTESIAN_POINT('',(2.36176947928705,0.00103427561139527,-1.32571981376975));
#7749=CARTESIAN_POINT('Ctrl Pts',(4.07816919733399,-1.04735432482649,-1.16244574507018));
#7750=CARTESIAN_POINT('Ctrl Pts',(4.02576993936297,-1.07430305395767,-1.16673746298016));
#7751=CARTESIAN_POINT('Ctrl Pts',(3.97140528621463,-1.09729006594874,-1.17109351575135));
#7752=CARTESIAN_POINT('Ctrl Pts',(3.89907451381304,-1.12165793381364,-1.17664363878772));
#7753=CARTESIAN_POINT('Ctrl Pts',(3.88249576664682,-1.12683790775929,-1.17789930736607));
#7754=CARTESIAN_POINT('Ctrl Pts',(3.84387492467964,-1.13797346763657,-1.18077851439586));
#7755=CARTESIAN_POINT('Ctrl Pts',(3.82176090442941,-1.14365895833256,-1.18239309715367));
#7756=CARTESIAN_POINT('Ctrl Pts',(3.793673930072,-1.1500156377344,-1.18438999917358));
#7757=CARTESIAN_POINT('Ctrl Pts',(3.78784384947714,-1.15128861186597,-1.18480160366909));
#7758=CARTESIAN_POINT('Ctrl Pts',(3.77862964379605,-1.15322724487107,-1.1854472995747));
#7759=CARTESIAN_POINT('Ctrl Pts',(3.7752519368968,-1.15392242424811,-1.18568297599713));
#7760=CARTESIAN_POINT('Ctrl Pts',(3.76885930787444,-1.15520887613308,-1.18612702649756));
#7761=CARTESIAN_POINT('Ctrl Pts',(3.765845148203,-1.15580318345222,-1.18633555663617));
#7762=CARTESIAN_POINT('Ctrl Pts',(3.75875951634206,-1.15717148922491,-1.18682383983025));
#7763=CARTESIAN_POINT('Ctrl Pts',(3.75468623909621,-1.15793580115188,-1.18710305112941));
#7764=CARTESIAN_POINT('Ctrl Pts',(3.74129006564816,-1.16037633702375,-1.1880166981226));
#7765=CARTESIAN_POINT('Ctrl Pts',(3.73195068943448,-1.16196164497823,-1.18864632247463));
#7766=CARTESIAN_POINT('Ctrl Pts',(3.67964637132004,-1.17019206334374,-1.1921366771471));
#7767=CARTESIAN_POINT('Ctrl Pts',(3.63635363864641,-1.17456759652873,-1.19489161152607));
#7768=CARTESIAN_POINT('Ctrl Pts',(3.53214613350913,-1.17929682718839,-1.20140941104788));
#7769=CARTESIAN_POINT('Ctrl Pts',(3.47125600694485,-1.1773426556639,-1.20512927121521));
#7770=CARTESIAN_POINT('Ctrl Pts',(3.35627386626345,-1.16469912933824,-1.21235313707226));
#7771=CARTESIAN_POINT('Ctrl Pts',(3.30225094683362,-1.15490499974966,-1.21583311105905));
#7772=CARTESIAN_POINT('Ctrl Pts',(3.23833792391426,-1.13864330090122,-1.22016387706283));
#7773=CARTESIAN_POINT('Ctrl Pts',(3.22760439318307,-1.13574991546692,-1.22089843078489));
#7774=CARTESIAN_POINT('Ctrl Pts',(3.21080718470864,-1.13096590859511,-1.22206013816313));
#7775=CARTESIAN_POINT('Ctrl Pts',(3.20471491851737,-1.12917738538525,-1.22248402212577));
#7776=CARTESIAN_POINT('Ctrl Pts',(3.19350052604868,-1.12578641165289,-1.22326912406143));
#7777=CARTESIAN_POINT('Ctrl Pts',(3.18837429237067,-1.12419803466002,-1.22362987959535));
#7778=CARTESIAN_POINT('Ctrl Pts',(3.17702541379756,-1.1205963588183,-1.22443280884789));
#7779=CARTESIAN_POINT('Ctrl Pts',(3.1708083605516,-1.11856616263138,-1.22487552068921));
#7780=CARTESIAN_POINT('Ctrl Pts',(3.1535420490446,-1.11276821304423,-1.22611319130398));
#7781=CARTESIAN_POINT('Ctrl Pts',(3.14253167525274,-1.10888788815956,-1.22691178483548));
#7782=CARTESIAN_POINT('Ctrl Pts',(3.11757796039311,-1.09967431559004,-1.22874370656214));
#7783=CARTESIAN_POINT('Ctrl Pts',(3.10367492285101,-1.09423843175196,-1.22978025392077));
#7784=CARTESIAN_POINT('Ctrl Pts',(3.05877932407595,-1.07569355690775,-1.2331803089629));
#7785=CARTESIAN_POINT('Ctrl Pts',(3.02824662366678,-1.06152129972799,-1.23557635164609));
#7786=CARTESIAN_POINT('Ctrl Pts',(2.9131747192986,-1.00199172343757,-1.24492209171011));
#7787=CARTESIAN_POINT('Ctrl Pts',(2.83369371688641,-0.947683414927965,-1.2520923931899));
#7788=CARTESIAN_POINT('Ctrl Pts',(2.74689536955338,-0.87133829678888,-1.26033802760937));
#7789=CARTESIAN_POINT('Ctrl Pts',(2.73243858553963,-0.857965011503711,-1.2617258781076));
#7790=CARTESIAN_POINT('Ctrl Pts',(2.71425643410172,-0.84027903678785,-1.2634830616131));
#7791=CARTESIAN_POINT('Ctrl Pts',(2.71021843622915,-0.836294051219419,-1.26387407605042));
#7792=CARTESIAN_POINT('Ctrl Pts',(2.70381824152164,-0.829885937273577,-1.2644948373947));
#7793=CARTESIAN_POINT('Ctrl Pts',(2.70143748236444,-0.827481599127388,-1.2647259754607));
#7794=CARTESIAN_POINT('Ctrl Pts',(2.6969002902336,-0.82285980225104,-1.26516684766887));
#7795=CARTESIAN_POINT('Ctrl Pts',(2.69474220501672,-0.820644082938962,-1.26537670272643));
#7796=CARTESIAN_POINT('Ctrl Pts',(2.69044817453351,-0.816200487295676,-1.26579462694863));
#7797=CARTESIAN_POINT('Ctrl Pts',(2.68831220304368,-0.813972660019503,-1.26600269974507));
#7798=CARTESIAN_POINT('Ctrl Pts',(2.68106270562862,-0.806351660297764,-1.26670964350527));
#7799=CARTESIAN_POINT('Ctrl Pts',(2.67599135001877,-0.80091835637258,-1.26720545364832));
#7800=CARTESIAN_POINT('Ctrl Pts',(2.63739458012216,-0.758774081422109,-1.27099222967911));
#7801=CARTESIAN_POINT('Ctrl Pts',(2.60616818009097,-0.720016726888708,-1.27413501527477));
#7802=CARTESIAN_POINT('Ctrl Pts',(2.54881866819172,-0.63880887967056,-1.28033320769855));
#7803=CARTESIAN_POINT('Ctrl Pts',(2.5227523346648,-0.596447477207469,-1.2833831006497));
#7804=CARTESIAN_POINT('Ctrl Pts',(2.47025513500272,-0.497633438810671,-1.29034240035067));
#7805=CARTESIAN_POINT('Ctrl Pts',(2.44547241356908,-0.440482454989256,-1.29426688321092));
#7806=CARTESIAN_POINT('Ctrl Pts',(2.42196509377384,-0.371853960864225,-1.29902829462145));
#7807=CARTESIAN_POINT('Ctrl Pts',(2.41874008757761,-0.362017568081936,-1.29971166474106));
#7808=CARTESIAN_POINT('Ctrl Pts',(2.41363805670928,-0.345734170114021,-1.30084510270445));
#7809=CARTESIAN_POINT('Ctrl Pts',(2.41168571945516,-0.33931121822877,-1.30129273502597));
#7810=CARTESIAN_POINT('Ctrl Pts',(2.40825472622772,-0.327666809348538,-1.30210542151025));
#7811=CARTESIAN_POINT('Ctrl Pts',(2.40675703548107,-0.322451120275434,-1.30246985168342));
#7812=CARTESIAN_POINT('Ctrl Pts',(2.40361755479659,-0.31122606167101,-1.30325515167251));
#7813=CARTESIAN_POINT('Ctrl Pts',(2.40198729933713,-0.305213666023405,-1.30367637871168));
#7814=CARTESIAN_POINT('Ctrl Pts',(2.39875087720502,-0.292891495436641,-1.30454100787296));
#7815=CARTESIAN_POINT('Ctrl Pts',(2.39714918565918,-0.286580777885108,-1.30498453668737));
#7816=CARTESIAN_POINT('Ctrl Pts',(2.39323485901956,-0.270603765024212,-1.30610936019814));
#7817=CARTESIAN_POINT('Ctrl Pts',(2.39099214593264,-0.260921030801323,-1.30679282937921));
#7818=CARTESIAN_POINT('Ctrl Pts',(2.3707780866703,-0.168332682349826,-1.31334643242981));
#7819=CARTESIAN_POINT('Ctrl Pts',(2.3616950574931,-0.0837599189378531,-1.31949818309692));
#7820=CARTESIAN_POINT('Ctrl Pts',(2.36176950434981,0.00103403308384097,
-1.32571983981107));
#7821=CARTESIAN_POINT('Ctrl Pts',(2.36176950455994,0.00103427238999479,
-1.32571985736988));
#7822=CARTESIAN_POINT('Ctrl Pts',(2.3618316127191,0.0717582489250692,-1.33090914618683));
#7823=CARTESIAN_POINT('Ctrl Pts',(2.36826403998405,0.142341883379032,-1.33611673408395));
#7824=CARTESIAN_POINT('Ctrl Pts',(2.38208108694226,0.217873682753449,-1.34148119336579));
#7825=CARTESIAN_POINT('Ctrl Pts',(2.38321426120892,0.223809783178999,-1.3419013035356));
#7826=CARTESIAN_POINT('Ctrl Pts',(2.38514025103522,0.233493727788146,-1.34258394379339));
#7827=CARTESIAN_POINT('Ctrl Pts',(2.38590573275984,0.2372468075739,-1.34284783772917));
#7828=CARTESIAN_POINT('Ctrl Pts',(2.38742299982363,0.244504808475719,-1.3433567962311));
#7829=CARTESIAN_POINT('Ctrl Pts',(2.3881725027798,0.248010159603775,-1.34360197964144));
#7830=CARTESIAN_POINT('Ctrl Pts',(2.38958880490685,0.254489253143669,-1.34405393722106));
#7831=CARTESIAN_POINT('Ctrl Pts',(2.39025114042218,0.257463824480693,-1.34426094528302));
#7832=CARTESIAN_POINT('Ctrl Pts',(2.39179232886378,0.264260889756969,-1.34473288535538));
#7833=CARTESIAN_POINT('Ctrl Pts',(2.3926787361519,0.268081591885901,-1.34499738933919));
#7834=CARTESIAN_POINT('Ctrl Pts',(2.39505853483023,0.278111439636333,-1.34568987077724));
#7835=CARTESIAN_POINT('Ctrl Pts',(2.39658339373676,0.284313090999179,-1.34611615072583));
#7836=CARTESIAN_POINT('Ctrl Pts',(2.41268497981492,0.347574961479989,-1.3504480310999));
#7837=CARTESIAN_POINT('Ctrl Pts',(2.43147386657798,0.403486333356421,-1.35414095607788));
#7838=CARTESIAN_POINT('Ctrl Pts',(2.47755504684468,0.512723754702348,-1.36150106191048));
#7839=CARTESIAN_POINT('Ctrl Pts',(2.50488077695117,0.565841544095042,-1.36515841169202));
#7840=CARTESIAN_POINT('Ctrl Pts',(2.56007294218793,0.655648196048438,-1.37178776666442));
#7841=CARTESIAN_POINT('Ctrl Pts',(2.58628298184903,0.693202345147572,-1.37471422240762));
#7842=CARTESIAN_POINT('Ctrl Pts',(2.6208166189692,0.73700844625919,-1.37838340892835));
#7843=CARTESIAN_POINT('Ctrl Pts',(2.62712451764267,0.744803204757438,-1.37904671598808));
#7844=CARTESIAN_POINT('Ctrl Pts',(2.6375206158764,0.757319532767677,-1.38012945697073));
#7845=CARTESIAN_POINT('Ctrl Pts',(2.64154828137164,0.762090904048538,-1.38054647071218));
#7846=CARTESIAN_POINT('Ctrl Pts',(2.64914594847734,0.770947621003043,-1.38132868766261));
#7847=CARTESIAN_POINT('Ctrl Pts',(2.65270662183671,0.775040779454269,-1.38169350517736));
#7848=CARTESIAN_POINT('Ctrl Pts',(2.66072333381586,0.784128786946163,-1.3825110434537));
#7849=CARTESIAN_POINT('Ctrl Pts',(2.66519390126566,0.789110509623414,-1.38296435684436));
#7850=CARTESIAN_POINT('Ctrl Pts',(2.67664225488379,0.801651121854137,-1.38411886726971));
#7851=CARTESIAN_POINT('Ctrl Pts',(2.68367694056488,0.80915706559828,-1.38482242984881));
#7852=CARTESIAN_POINT('Ctrl Pts',(2.73192855647619,0.859307883708574,-1.38961039835936));
#7853=CARTESIAN_POINT('Ctrl Pts',(2.77621110070649,0.898872316516266,-1.39382768074379));
#7854=CARTESIAN_POINT('Ctrl Pts',(2.88362765269659,0.981163177718446,-1.40365131255873));
#7855=CARTESIAN_POINT('Ctrl Pts',(2.94830986454206,1.02144312229219,-1.40929631897689));
#7856=CARTESIAN_POINT('Ctrl Pts',(3.03375213589413,1.06379934451007,-1.41617130460775));
#7857=CARTESIAN_POINT('Ctrl Pts',(3.0512926690889,1.07196282772527,-1.41755323438093));
#7858=CARTESIAN_POINT('Ctrl Pts',(3.08043278222723,1.084661075202,-1.4197926946376));
#7859=CARTESIAN_POINT('Ctrl Pts',(3.09191688692745,1.0894504044617,-1.4206612258589));
#7860=CARTESIAN_POINT('Ctrl Pts',(3.10766940087072,1.09572867422096,-1.42183154352114));
#7861=CARTESIAN_POINT('Ctrl Pts',(3.11187318018332,1.09737617008166,-1.42214183994511));
#7862=CARTESIAN_POINT('Ctrl Pts',(3.11906077122121,1.10014547130468,-1.42266882088822));
#7863=CARTESIAN_POINT('Ctrl Pts',(3.12203981937891,1.10127939912676,-1.42288620101202));
#7864=CARTESIAN_POINT('Ctrl Pts',(3.12768468402624,1.10340183084448,-1.42329609474297));
#7865=CARTESIAN_POINT('Ctrl Pts',(3.13034953167384,1.10439279743214,-1.42348875607539));
#7866=CARTESIAN_POINT('Ctrl Pts',(3.13666344259839,1.10671473669516,-1.42394330240407));
#7867=CARTESIAN_POINT('Ctrl Pts',(3.14031558131096,1.10803733713445,-1.42420470220452));
#7868=CARTESIAN_POINT('Ctrl Pts',(3.15320797390597,1.11263422369046,-1.42512233746239));
#7869=CARTESIAN_POINT('Ctrl Pts',(3.16248280395331,1.11581129577218,-1.42577323030606));
#7870=CARTESIAN_POINT('Ctrl Pts',(3.23929691575225,1.14105660205805,-1.43109631842507));
#7871=CARTESIAN_POINT('Ctrl Pts',(3.3086761641128,1.15709026437917,-1.43548099024168));
#7872=CARTESIAN_POINT('Ctrl Pts',(3.43746624218953,1.17479912980643,-1.44352234568844));
#7873=CARTESIAN_POINT('Ctrl Pts',(3.4963627932792,1.17843313375853,-1.4471639933981));
#7874=CARTESIAN_POINT('Ctrl Pts',(3.57651064851413,1.17736036807189,-1.45227287948557));
#7875=CARTESIAN_POINT('Ctrl Pts',(3.59772707650814,1.17650225660571,-1.45363929630321));
#7876=CARTESIAN_POINT('Ctrl Pts',(3.63459052712418,1.17401173194954,-1.45604610339223));
#7877=CARTESIAN_POINT('Ctrl Pts',(3.65024981481946,1.17263838944303,-1.45707877662303));
#7878=CARTESIAN_POINT('Ctrl Pts',(3.67303150385934,1.17018002019119,-1.45859831690869));
#7879=CARTESIAN_POINT('Ctrl Pts',(3.68017929364281,1.16934235663094,-1.4590775441531));
#7880=CARTESIAN_POINT('Ctrl Pts',(3.69275525302512,1.16775158160077,-1.45992526208627));
#7881=CARTESIAN_POINT('Ctrl Pts',(3.69818673352052,1.16702598716979,-1.46029288747278));
#7882=CARTESIAN_POINT('Ctrl Pts',(3.70950597616199,1.16543336305644,-1.46106224750131));
#7883=CARTESIAN_POINT('Ctrl Pts',(3.71539261237314,1.16455955906661,-1.46146418363111));
#7884=CARTESIAN_POINT('Ctrl Pts',(3.73074431239596,1.16216172277481,-1.46251728885668));
#7885=CARTESIAN_POINT('Ctrl Pts',(3.74019767451009,1.16056669395232,-1.46317065540774));
#7886=CARTESIAN_POINT('Ctrl Pts',(3.7800905088818,1.15333376009729,-1.46594918382699));
#7887=CARTESIAN_POINT('Ctrl Pts',(3.8103184753016,1.14661273075189,-1.46810775892774));
#7888=CARTESIAN_POINT('Ctrl Pts',(3.92056556168208,1.11749723599098,-1.47618312755397));
#7889=CARTESIAN_POINT('Ctrl Pts',(3.99840889809731,1.08784799929712,-1.48230636237904));
#7890=CARTESIAN_POINT('Ctrl Pts',(4.1189822626446,1.02666329477687,-1.49220390399194));
#7891=CARTESIAN_POINT('Ctrl Pts',(4.16387793549038,0.999996208824154,-1.49598770743971));
#7892=CARTESIAN_POINT('Ctrl Pts',(4.21259434248166,0.966495272226091,-1.50009989169716));
#7893=CARTESIAN_POINT('Ctrl Pts',(4.21829173769634,0.962502522009824,-1.50058087412274));
#7894=CARTESIAN_POINT('Ctrl Pts',(4.22693279799507,0.956331952767353,-1.5013100564271));
#7895=CARTESIAN_POINT('Ctrl Pts',(4.22990212372354,0.954190587488126,-1.50156056874576));
#7896=CARTESIAN_POINT('Ctrl Pts',(4.23532005820118,0.950244847781599,-1.50201748694578));
#7897=CARTESIAN_POINT('Ctrl Pts',(4.23777167179021,0.948444827262517,-1.502224168693));
#7898=CARTESIAN_POINT('Ctrl Pts',(4.24329089556351,0.944359510039678,-1.50268931573189));
#7899=CARTESIAN_POINT('Ctrl Pts',(4.24635436362051,0.942068752939169,-1.50294740299022));
#7900=CARTESIAN_POINT('Ctrl Pts',(4.25424385238277,0.936109112073236,-1.50361197863511));
#7901=CARTESIAN_POINT('Ctrl Pts',(4.25905287615919,0.93241776563965,-1.50401698352366));
#7902=CARTESIAN_POINT('Ctrl Pts',(4.29115064480108,0.907383698772624,-1.50672122581093));
#7903=CARTESIAN_POINT('Ctrl Pts',(4.31751758579733,0.884880791182493,-1.50894791567869));
#7904=CARTESIAN_POINT('Ctrl Pts',(4.36349461672023,0.841995159055702,-1.51292074942563));
#7905=CARTESIAN_POINT('Ctrl Pts',(4.38343501338009,0.822008242197079,-1.51467807736372));
#7906=CARTESIAN_POINT('Ctrl Pts',(4.43527920891394,0.766165946216926,-1.51940251074137));
#7907=CARTESIAN_POINT('Ctrl Pts',(4.46574048346297,0.729047517585867,-1.52235266101881));
#7908=CARTESIAN_POINT('Ctrl Pts',(4.52510298521389,0.646964528934716,-1.52868743618457));
#7909=CARTESIAN_POINT('Ctrl Pts',(4.55337853077468,0.601686516700835,-1.53207738809864));
#7910=CARTESIAN_POINT('Ctrl Pts',(4.58358801708743,0.545098479382363,-1.53629338947441));
#7911=CARTESIAN_POINT('Ctrl Pts',(4.58855632442101,0.535474690689785,-1.53700954969279));
#7912=CARTESIAN_POINT('Ctrl Pts',(4.59616862370413,0.520216734750667,-1.53814435401415));
#7913=CARTESIAN_POINT('Ctrl Pts',(4.59890197018941,0.514627631041915,-1.53855990943113));
#7914=CARTESIAN_POINT('Ctrl Pts',(4.60393648862499,0.50412303536163,-1.53934082251706));
#7915=CARTESIAN_POINT('Ctrl Pts',(4.60624822441958,0.499212765448509,-1.53970580633719));
#7916=CARTESIAN_POINT('Ctrl Pts',(4.61134783473277,0.488183705389914,-1.54052559207426));
#7917=CARTESIAN_POINT('Ctrl Pts',(4.61411739477131,0.482056706379556,-1.54098100166922));
#7918=CARTESIAN_POINT('Ctrl Pts',(4.62103141966154,0.466405343395531,-1.54214448823909));
#7919=CARTESIAN_POINT('Ctrl Pts',(4.62510255603357,0.456849416693217,-1.54285499495748));
#7920=CARTESIAN_POINT('Ctrl Pts',(4.657696268072,0.377447624340864,-1.54876135210881));
#7921=CARTESIAN_POINT('Ctrl Pts',(4.67956810737112,0.305075840223965,-1.55417873270455));
#7922=CARTESIAN_POINT('Ctrl Pts',(4.70570496835024,0.17447817038836,-1.56392160117353));
#7923=CARTESIAN_POINT('Ctrl Pts',(4.71285866530789,0.117075292893958,-1.56818821438827));
#7924=CARTESIAN_POINT('Ctrl Pts',(4.71680672146982,0.038866566434532,-1.57384334564509));
#7925=CARTESIAN_POINT('Ctrl Pts',(4.71730552758499,0.0183298876278521,-1.57531310782353));
#7926=CARTESIAN_POINT('Ctrl Pts',(4.7172424454715,-0.015280427074099,-1.57768356586059));
#7927=CARTESIAN_POINT('Ctrl Pts',(4.71700035115201,-0.0283497556969264,
-1.57859665273772));
#7928=CARTESIAN_POINT('Ctrl Pts',(4.71637531937082,-0.0461141263351836,
-1.57982363920567));
#7929=CARTESIAN_POINT('Ctrl Pts',(4.71618174531947,-0.0508143162551278,
-1.58014693564405));
#7930=CARTESIAN_POINT('Ctrl Pts',(4.71581049738897,-0.0586818204140145,
-1.58068569924795));
#7931=CARTESIAN_POINT('Ctrl Pts',(4.71564818095615,-0.0618497642636594,
-1.58090198879334));
#7932=CARTESIAN_POINT('Ctrl Pts',(4.71531540461906,-0.0678686395293367,
-1.58131164072307));
#7933=CARTESIAN_POINT('Ctrl Pts',(4.71514737138161,-0.0707196590406,-1.58150513920623));
#7934=CARTESIAN_POINT('Ctrl Pts',(4.71472313943746,-0.0774977326646866,
-1.58196392950753));
#7935=CARTESIAN_POINT('Ctrl Pts',(4.71445762330664,-0.0814242006804311,
-1.5822287140472));
#7936=CARTESIAN_POINT('Ctrl Pts',(4.71344767563238,-0.0953239980667431,
-1.58316279244578));
#7937=CARTESIAN_POINT('Ctrl Pts',(4.7125958736893,-0.105289432774669,-1.58382652127418));
#7938=CARTESIAN_POINT('Ctrl Pts',(4.70563587225787,-0.176077160377908,-1.58850649901327));
#7939=CARTESIAN_POINT('Ctrl Pts',(4.69492668981321,-0.236361462750202,-1.59231237929681));
#7940=CARTESIAN_POINT('Ctrl Pts',(4.66588685364125,-0.348381352898507,-1.59947994226449));
#7941=CARTESIAN_POINT('Ctrl Pts',(4.6485350061951,-0.400196614390326,-1.6028371824813));
#7942=CARTESIAN_POINT('Ctrl Pts',(4.61080228182311,-0.491311488272371,-1.60904849008933));
#7943=CARTESIAN_POINT('Ctrl Pts',(4.59168402756789,-0.531020647848604,-1.6118688383184));
#7944=CARTESIAN_POINT('Ctrl Pts',(4.56539714877969,-0.578598079656185,-1.61544518159952));
#7945=CARTESIAN_POINT('Ctrl Pts',(4.56028687385215,-0.587566719640654,-1.61612828721391));
#7946=CARTESIAN_POINT('Ctrl Pts',(4.55196436989243,-0.601736560116374,-1.61722248861349));
#7947=CARTESIAN_POINT('Ctrl Pts',(4.54882831401767,-0.606982059653343,-1.61763086245697));
#7948=CARTESIAN_POINT('Ctrl Pts',(4.542822908943,-0.61685171943176,-1.61840565615444));
#7949=CARTESIAN_POINT('Ctrl Pts',(4.53996204877292,-0.621480877932946,-1.61877176183307));
#7950=CARTESIAN_POINT('Ctrl Pts',(4.53340646425925,-0.631925901611348,-1.61960407368689));
#7951=CARTESIAN_POINT('Ctrl Pts',(4.5296926049546,-0.637729460607134,-1.62007096988646));
#7952=CARTESIAN_POINT('Ctrl Pts',(4.51823383336954,-0.655294396340474,-1.62149786795583));
#7953=CARTESIAN_POINT('Ctrl Pts',(4.51032894919217,-0.666949385558651,-1.6224637313036));
#7954=CARTESIAN_POINT('Ctrl Pts',(4.44531516409617,-0.759200527579021,-1.63026651294974));
#7955=CARTESIAN_POINT('Ctrl Pts',(4.37849165128539,-0.832447743524141,-1.63749260957849));
#7956=CARTESIAN_POINT('Ctrl Pts',(4.271917002868,-0.923250686143749,-1.64776100941429));
#7957=CARTESIAN_POINT('Ctrl Pts',(4.23911262651118,-0.948350069162419,-1.65077662203512));
#7958=CARTESIAN_POINT('Ctrl Pts',(4.19352502348027,-0.979574703247726,-1.6547226198031));
#7959=CARTESIAN_POINT('Ctrl Pts',(4.18185357360667,-0.987267344477696,-1.65571257675743));
#7960=CARTESIAN_POINT('Ctrl Pts',(4.16174350135364,-1.00001422710019,-1.65738065995565));
#7961=CARTESIAN_POINT('Ctrl Pts',(4.15337366153134,-1.00517374316936,-1.65806411209736));
#7962=CARTESIAN_POINT('Ctrl Pts',(4.14133160563545,-1.0123904416387,-1.65903105884131));
#7963=CARTESIAN_POINT('Ctrl Pts',(4.13771172393355,-1.01453353057352,-1.65931964380046));
#7964=CARTESIAN_POINT('Ctrl Pts',(4.13142065082237,-1.01821267497635,-1.65981748317565));
#7965=CARTESIAN_POINT('Ctrl Pts',(4.128754797754,-1.01975771191621,-1.66002729929873));
#7966=CARTESIAN_POINT('Ctrl Pts',(4.12311931540191,-1.02299436586058,-1.66046839975546));
#7967=CARTESIAN_POINT('Ctrl Pts',(4.12014836235405,-1.02468353394657,-1.66069953141028));
#7968=CARTESIAN_POINT('Ctrl Pts',(4.11209225081034,-1.029217636917,-1.66132258419626));
#7969=CARTESIAN_POINT('Ctrl Pts',(4.10699318220491,-1.03203785161569,-1.66171298662176));
#7970=CARTESIAN_POINT('Ctrl Pts',(4.09401964825911,-1.03908808278284,-1.66269684771795));
#7971=CARTESIAN_POINT('Ctrl Pts',(4.08611780186023,-1.04326638858741,-1.66328736455055));
#7972=CARTESIAN_POINT('Ctrl Pts',(4.07816926735968,-1.04735428881255,-1.66387346933803));
#7973=CARTESIAN_POINT('Origin',(3.53951905042299,8.32667268468867E-16,0.924367114736157));
#7974=CARTESIAN_POINT('',(4.07816947157496,-1.04735418378541,-2.2618380236781));
#7975=CARTESIAN_POINT('',(4.07816926754606,-1.0473542887167,-2.1620461556085));
#7976=CARTESIAN_POINT('',(4.07816926754759,-1.04735428871592,0.924367114736157));
#7977=CARTESIAN_POINT('',(2.36176911741392,-0.000397236870587705,-1.92540593443103));
#7978=CARTESIAN_POINT('Ctrl Pts',(4.07816947157471,-1.04735418378554,-2.26183802367812));
#7979=CARTESIAN_POINT('Ctrl Pts',(4.11215758083515,-1.02987422366249,-2.25946260336971));
#7980=CARTESIAN_POINT('Ctrl Pts',(4.14531453423107,-1.01072974373671,-2.25706537766911));
#7981=CARTESIAN_POINT('Ctrl Pts',(4.20217770663557,-0.974083814098255,-2.2527434404038));
#7982=CARTESIAN_POINT('Ctrl Pts',(4.22623386750672,-0.957276505535751,-2.25084314837658));
#7983=CARTESIAN_POINT('Ctrl Pts',(4.25716496907334,-0.93389959830894,-2.2482872055146));
#7984=CARTESIAN_POINT('Ctrl Pts',(4.26462500625597,-0.928119318065563,-2.24766173080797));
#7985=CARTESIAN_POINT('Ctrl Pts',(4.27664969228473,-0.918568732447784,-2.24663826132436));
#7986=CARTESIAN_POINT('Ctrl Pts',(4.28125689308624,-0.914852485376131,-2.24624239545728));
#7987=CARTESIAN_POINT('Ctrl Pts',(4.29008411770402,-0.907621782651955,-2.24547658656779));
#7988=CARTESIAN_POINT('Ctrl Pts',(4.29430796646247,-0.904112222590754,-2.24510684538091));
#7989=CARTESIAN_POINT('Ctrl Pts',(4.30406877140576,-0.895885980637119,-2.24424460835135));
#7990=CARTESIAN_POINT('Ctrl Pts',(4.309586835554,-0.891147332573264,-2.243751231464));
#7991=CARTESIAN_POINT('Ctrl Pts',(4.32720909635388,-0.875728286276171,-2.24215610848428));
#7992=CARTESIAN_POINT('Ctrl Pts',(4.33913727081319,-0.864850447594686,-2.24104630044757));
#7993=CARTESIAN_POINT('Ctrl Pts',(4.3667713270253,-0.838589231985334,-2.23840152057983));
#7994=CARTESIAN_POINT('Ctrl Pts',(4.38227705102541,-0.823004905773187,-2.23685846807011));
#7995=CARTESIAN_POINT('Ctrl Pts',(4.47088258983569,-0.728819380887682,-2.22768368720859));
#7996=CARTESIAN_POINT('Ctrl Pts',(4.53338307284256,-0.640971426619844,-2.21965793610917));
#7997=CARTESIAN_POINT('Ctrl Pts',(4.59571007065897,-0.521817399269699,-2.20997664042911));
#7998=CARTESIAN_POINT('Ctrl Pts',(4.60746466445453,-0.497318106622457,-2.2080468105851));
#7999=CARTESIAN_POINT('Ctrl Pts',(4.62085781807206,-0.466733578152843,-2.205729139911));
#8000=CARTESIAN_POINT('Ctrl Pts',(4.6233081351772,-0.461015170455292,-2.20529965444803));
#8001=CARTESIAN_POINT('Ctrl Pts',(4.62708194335128,-0.452011676322391,-2.2046297597358));
#8002=CARTESIAN_POINT('Ctrl Pts',(4.62843608217146,-0.44873968000058,-2.20438761100135));
#8003=CARTESIAN_POINT('Ctrl Pts',(4.63091947955316,-0.442661625021243,-2.20394026837235));
#8004=CARTESIAN_POINT('Ctrl Pts',(4.63205268204052,-0.439857334893244,-2.20373485236454));
#8005=CARTESIAN_POINT('Ctrl Pts',(4.63464831004131,-0.433362120813096,-2.20326129897013));
#8006=CARTESIAN_POINT('Ctrl Pts',(4.63610288887783,-0.42966813870244,-2.20299362569074));
#8007=CARTESIAN_POINT('Ctrl Pts',(4.64061729671911,-0.418031295518201,-2.20215535390965));
#8008=CARTESIAN_POINT('Ctrl Pts',(4.64360979867758,-0.410062363483671,-2.2015885365557));
#8009=CARTESIAN_POINT('Ctrl Pts',(4.66813750629124,-0.34253016373789,-2.19684023918535));
#8010=CARTESIAN_POINT('Ctrl Pts',(4.68492505219069,-0.281342976766287,-2.19289530235418));
#8011=CARTESIAN_POINT('Ctrl Pts',(4.71371485167868,-0.129284182677625,-2.18330913748751));
#8012=CARTESIAN_POINT('Ctrl Pts',(4.72020462868668,-0.0378102537561371,
-2.17770182371934));
#8013=CARTESIAN_POINT('Ctrl Pts',(4.71544570556673,0.0668640017647441,-2.17086642501106));
#8014=CARTESIAN_POINT('Ctrl Pts',(4.71460970412638,0.080226087733796,-2.16998668468026));
#8015=CARTESIAN_POINT('Ctrl Pts',(4.71300288566029,0.100386784409726,-2.16864710546221));
#8016=CARTESIAN_POINT('Ctrl Pts',(4.71240029154313,0.10719798969088,-2.1681924230823));
#8017=CARTESIAN_POINT('Ctrl Pts',(4.7112466021464,0.119060588088743,-2.16739667559879));
#8018=CARTESIAN_POINT('Ctrl Pts',(4.71072205864656,0.124114428083257,-2.16705643887368));
#8019=CARTESIAN_POINT('Ctrl Pts',(4.70955401554414,0.134700642993628,-2.1663411069894));
#8020=CARTESIAN_POINT('Ctrl Pts',(4.7089039420901,0.140232150874098,-2.16596581598723));
#8021=CARTESIAN_POINT('Ctrl Pts',(4.70725682905048,0.153438724543941,-2.16506607621159));
#8022=CARTESIAN_POINT('Ctrl Pts',(4.7062233315853,0.161108898539571,-2.16454050676996));
#8023=CARTESIAN_POINT('Ctrl Pts',(4.70240423910555,0.187485413052257,-2.1627224427146));
#8024=CARTESIAN_POINT('Ctrl Pts',(4.69924383924312,0.206133657309007,-2.16141840423657));
#8025=CARTESIAN_POINT('Ctrl Pts',(4.69046214842808,0.251317478911881,-2.15821132314327));
#8026=CARTESIAN_POINT('Ctrl Pts',(4.68437077120608,0.27774958959409,-2.15629477942774));
#8027=CARTESIAN_POINT('Ctrl Pts',(4.65162394725014,0.400340676491821,-2.14721891650269));
#8028=CARTESIAN_POINT('Ctrl Pts',(4.61373470193974,0.493059158604357,-2.13976386588413));
#8029=CARTESIAN_POINT('Ctrl Pts',(4.55193428615204,0.602307224508113,-2.1307411603056));
#8030=CARTESIAN_POINT('Ctrl Pts',(4.5385179544109,0.624307633798722,-2.12891358198425));
#8031=CARTESIAN_POINT('Ctrl Pts',(4.52102998027965,0.650975339720166,-2.12670056281189));
#8032=CARTESIAN_POINT('Ctrl Pts',(4.51763024335496,0.656072478203973,-2.12627768945603));
#8033=CARTESIAN_POINT('Ctrl Pts',(4.51221505622762,0.664055667867854,-2.12561584399497));
#8034=CARTESIAN_POINT('Ctrl Pts',(4.51022623855985,0.666959523099655,-2.12537519781994));
#8035=CARTESIAN_POINT('Ctrl Pts',(4.50665998089947,0.672116841662521,-2.12494804067539));
#8036=CARTESIAN_POINT('Ctrl Pts',(4.50508766668906,0.674373691490797,-2.12476120318403));
#8037=CARTESIAN_POINT('Ctrl Pts',(4.50129598067297,0.679775709909808,-2.1243141713941));
#8038=CARTESIAN_POINT('Ctrl Pts',(4.49906908066863,0.682915529074666,-2.12405448696543));
#8039=CARTESIAN_POINT('Ctrl Pts',(4.49223419721483,0.692452938799442,-2.12326593058064));
#8040=CARTESIAN_POINT('Ctrl Pts',(4.48757721896689,0.698815383849004,-2.12274022981454));
#8041=CARTESIAN_POINT('Ctrl Pts',(4.47658100425813,0.713526330734583,-2.12152430837908));
#8042=CARTESIAN_POINT('Ctrl Pts',(4.47019342475584,0.721838039770002,-2.12083698845388));
#8043=CARTESIAN_POINT('Ctrl Pts',(4.44740839806692,0.750681256627044,-2.11844635983074));
#8044=CARTESIAN_POINT('Ctrl Pts',(4.43043479654834,0.770749463485985,-2.11677300933939));
#8045=CARTESIAN_POINT('Ctrl Pts',(4.36050131592672,0.848032599723353,-2.1102126406485));
#8046=CARTESIAN_POINT('Ctrl Pts',(4.3025902750351,0.900496669303082,-2.10548104231662));
#8047=CARTESIAN_POINT('Ctrl Pts',(4.20175653762746,0.975084504588112,-2.09760778914742));
#8048=CARTESIAN_POINT('Ctrl Pts',(4.16192695028842,1.00097746188242,-2.09457846753382));
#8049=CARTESIAN_POINT('Ctrl Pts',(4.11127305683629,1.0297128581226,-2.09075148776885));
#8050=CARTESIAN_POINT('Ctrl Pts',(4.10182672876283,1.03490157809261,-2.0900389666824));
#8051=CARTESIAN_POINT('Ctrl Pts',(4.08677129796594,1.04290430817441,-2.08890449710871));
#8052=CARTESIAN_POINT('Ctrl Pts',(4.08120847701314,1.04580446595101,-2.08848556605197));
#8053=CARTESIAN_POINT('Ctrl Pts',(4.07079358406968,1.05112884525956,-2.08770154637793));
#8054=CARTESIAN_POINT('Ctrl Pts',(4.06594740098486,1.05356426926796,-2.08733685853089));
#8055=CARTESIAN_POINT('Ctrl Pts',(4.05511558356286,1.05891434936965,-2.0865219260801));
#8056=CARTESIAN_POINT('Ctrl Pts',(4.04912174727154,1.06181188188193,-2.0860711070971));
#8057=CARTESIAN_POINT('Ctrl Pts',(4.03143809584658,1.07017627064171,-2.08474123869227));
#8058=CARTESIAN_POINT('Ctrl Pts',(4.01968293775442,1.07550184372176,-2.08385743759266));
#8059=CARTESIAN_POINT('Ctrl Pts',(3.99273256546268,1.08718157750333,-2.08183095835449));
#8060=CARTESIAN_POINT('Ctrl Pts',(3.97748708335784,1.09341219513607,-2.08068441911204));
#8061=CARTESIAN_POINT('Ctrl Pts',(3.92569009147095,1.11332383607517,-2.07678754461713));
#8062=CARTESIAN_POINT('Ctrl Pts',(3.88859349658233,1.12550635338703,-2.07399316840746));
#8063=CARTESIAN_POINT('Ctrl Pts',(3.7814610450674,1.15488222956353,-2.06593461515874));
#8064=CARTESIAN_POINT('Ctrl Pts',(3.71035896181017,1.16751964654541,-2.06059098939022));
#8065=CARTESIAN_POINT('Ctrl Pts',(3.60548304147,1.17636940656165,-2.05296937992301));
#8066=CARTESIAN_POINT('Ctrl Pts',(3.57231008323076,1.1777611902697,-2.0505982642458));
#8067=CARTESIAN_POINT('Ctrl Pts',(3.53312072607992,1.17774789747898,-2.04787495365456));
#8068=CARTESIAN_POINT('Ctrl Pts',(3.52712183278505,1.17770003027821,-2.04746024793411));
#8069=CARTESIAN_POINT('Ctrl Pts',(3.51731756208877,1.17754687569113,-2.04678628912809));
#8070=CARTESIAN_POINT('Ctrl Pts',(3.51351195435492,1.1774689730574,-2.04652562603348));
#8071=CARTESIAN_POINT('Ctrl Pts',(3.50666647525204,1.17729563825144,-2.04605851795721));
#8072=CARTESIAN_POINT('Ctrl Pts',(3.5036265483414,1.17720688090659,-2.04585171945102));
#8073=CARTESIAN_POINT('Ctrl Pts',(3.49691052135481,1.17698475189216,-2.04539624495085));
#8074=CARTESIAN_POINT('Ctrl Pts',(3.49323468466054,1.17684593356359,-2.04514786960628));
#8075=CARTESIAN_POINT('Ctrl Pts',(3.48252650955096,1.17639128900629,-2.04442683417521));
#8076=CARTESIAN_POINT('Ctrl Pts',(3.47549612928041,1.17602962807248,-2.04395660247968));
#8077=CARTESIAN_POINT('Ctrl Pts',(3.41115089259976,1.17214080537759,-2.03967830741393));
#8078=CARTESIAN_POINT('Ctrl Pts',(3.3541541710711,1.16448880190623,-2.03607198645818));
#8079=CARTESIAN_POINT('Ctrl Pts',(3.2024120382917,1.1326869105901,-2.02644088861025));
#8080=CARTESIAN_POINT('Ctrl Pts',(3.10975637537805,1.10087381460123,-2.02049531625501));
#8081=CARTESIAN_POINT('Ctrl Pts',(3.00780374125507,1.05101224451846,-2.01310856129686));
#8082=CARTESIAN_POINT('Ctrl Pts',(2.99366295095826,1.04373798808611,-2.01206470887801));
#8083=CARTESIAN_POINT('Ctrl Pts',(2.97379801676143,1.03300502674894,-2.01056840659868));
#8084=CARTESIAN_POINT('Ctrl Pts',(2.9679489654152,1.02978022319167,-2.01012408261745));
#8085=CARTESIAN_POINT('Ctrl Pts',(2.95729270577498,1.02378626686852,-2.00930750860868));
#8086=CARTESIAN_POINT('Ctrl Pts',(2.9524769999611,1.02103254885945,-2.0089358110551));
#8087=CARTESIAN_POINT('Ctrl Pts',(2.94285131455196,1.01543777826472,-2.00818736994075));
#8088=CARTESIAN_POINT('Ctrl Pts',(2.938041738276,1.01259632118592,-2.00781061903259));
#8089=CARTESIAN_POINT('Ctrl Pts',(2.92626881634285,1.00552750842987,-2.0068814297528));
#8090=CARTESIAN_POINT('Ctrl Pts',(2.91932885318496,1.00126197035577,-2.00632762542175));
#8091=CARTESIAN_POINT('Ctrl Pts',(2.90451906600554,0.991946325149986,-2.00513248953443));
#8092=CARTESIAN_POINT('Ctrl Pts',(2.89666406024447,0.986873824292692,-2.00449036917237));
#8093=CARTESIAN_POINT('Ctrl Pts',(2.87464714894385,0.972281638756984,-2.00266682334521));
#8094=CARTESIAN_POINT('Ctrl Pts',(2.86063103430509,0.962547266700664,-2.00147770287939));
#8095=CARTESIAN_POINT('Ctrl Pts',(2.81349702912591,0.928270418454225,-1.99738015845952));
#8096=CARTESIAN_POINT('Ctrl Pts',(2.78146088420264,0.902297715308902,-1.99442252922296));
#8097=CARTESIAN_POINT('Ctrl Pts',(2.70616918336809,0.834411838518283,-1.98705391224051));
#8098=CARTESIAN_POINT('Ctrl Pts',(2.66463857002055,0.790758461605782,-1.98260760915353));
#8099=CARTESIAN_POINT('Ctrl Pts',(2.60063731001027,0.712241557537544,-1.97522936642346));
#8100=CARTESIAN_POINT('Ctrl Pts',(2.57633397546382,0.679015628986144,-1.97226989362256));
#8101=CARTESIAN_POINT('Ctrl Pts',(2.55037091061868,0.639312652357029,-1.96897017960545));
#8102=CARTESIAN_POINT('Ctrl Pts',(2.54696699242296,0.634015083744507,-1.96853455859723));
#8103=CARTESIAN_POINT('Ctrl Pts',(2.54152603994987,0.625396027070788,-1.96783363163928));
#8104=CARTESIAN_POINT('Ctrl Pts',(2.53946276683566,0.622091368194459,-1.96756672717929));
#8105=CARTESIAN_POINT('Ctrl Pts',(2.53581561511723,0.616184837461929,-1.96709303220929));
#8106=CARTESIAN_POINT('Ctrl Pts',(2.53422539493126,0.613587000271265,-1.96688584118828));
#8107=CARTESIAN_POINT('Ctrl Pts',(2.53077500214972,0.6079008999427,-1.96643486230176));
#8108=CARTESIAN_POINT('Ctrl Pts',(2.52891892131867,0.60481025041238,-1.96619133536824));
#8109=CARTESIAN_POINT('Ctrl Pts',(2.52365889129935,0.595959697982457,-1.96549837076114));
#8110=CARTESIAN_POINT('Ctrl Pts',(2.52028972365367,0.590179133082911,-1.96505108093439));
#8111=CARTESIAN_POINT('Ctrl Pts',(2.49641477132662,0.5484019851808,-1.96185407804208));
#8112=CARTESIAN_POINT('Ctrl Pts',(2.47776918723934,0.511370038509786,-1.95920885266609));
#8113=CARTESIAN_POINT('Ctrl Pts',(2.41980830418625,0.379342855806727,-1.95015498242245));
#8114=CARTESIAN_POINT('Ctrl Pts',(2.39099501075109,0.280260983889823,-1.94396970864142));
#8115=CARTESIAN_POINT('Ctrl Pts',(2.37173171027098,0.154769869163562,-1.93580584997123));
#8116=CARTESIAN_POINT('Ctrl Pts',(2.36879774570251,0.130738213834044,-1.93423048381664));
#8117=CARTESIAN_POINT('Ctrl Pts',(2.36581330168438,0.0979111982545516,-1.93205397431837));
#8118=CARTESIAN_POINT('Ctrl Pts',(2.36511758903647,0.0891795268502272,-1.93147270768654));
#8119=CARTESIAN_POINT('Ctrl Pts',(2.36416443601409,0.0752568612788502,-1.9305418081047));
#8120=CARTESIAN_POINT('Ctrl Pts',(2.36384383938036,0.0700704035632612,-1.93019413285541));
#8121=CARTESIAN_POINT('Ctrl Pts',(2.36326952695623,0.0596612204248427,-1.92949447181395));
#8122=CARTESIAN_POINT('Ctrl Pts',(2.36301624930578,0.0544385904398576,-1.92914248066085));
#8123=CARTESIAN_POINT('Ctrl Pts',(2.36257502195804,0.0438888252418186,-1.9284294689818));
#8124=CARTESIAN_POINT('Ctrl Pts',(2.36238844412332,0.0385617584877063,-1.92806841444257));
#8125=CARTESIAN_POINT('Ctrl Pts',(2.36208103489016,0.0276719919876058,-1.92732818045086));
#8126=CARTESIAN_POINT('Ctrl Pts',(2.36196344888742,0.0221093421832516,-1.92694890990719));
#8127=CARTESIAN_POINT('Ctrl Pts',(2.36180593426867,0.0108986051649463,-1.92618216766589));
#8128=CARTESIAN_POINT('Ctrl Pts',(2.36176721246393,0.005250664645738,-1.92579466996232));
#8129=CARTESIAN_POINT('Ctrl Pts',(2.36176911741392,-0.000397236870587705,
-1.92540593443103));
#8130=CARTESIAN_POINT('Ctrl Pts',(2.36176911714533,-0.000396439730100908,
-1.92540598929686));
#8131=CARTESIAN_POINT('Ctrl Pts',(2.36177360458169,-0.0137277924659618,
-1.9244884150583));
#8132=CARTESIAN_POINT('Ctrl Pts',(2.36200444424012,-0.0270577270212485,
-1.92356401270832));
#8133=CARTESIAN_POINT('Ctrl Pts',(2.36611628666943,-0.146914392811943,-1.91518818397968));
#8134=CARTESIAN_POINT('Ctrl Pts',(2.38421792108532,-0.252445856471833,-1.9072920268355));
#8135=CARTESIAN_POINT('Ctrl Pts',(2.42501706749847,-0.38187722484146,-1.89739960912129));
#8136=CARTESIAN_POINT('Ctrl Pts',(2.43481099395957,-0.409347312572779,-1.89529194144152));
#8137=CARTESIAN_POINT('Ctrl Pts',(2.45179991403706,-0.451930007109447,-1.89203809039909));
#8138=CARTESIAN_POINT('Ctrl Pts',(2.45831418179976,-0.467300496119891,-1.89086647598472));
#8139=CARTESIAN_POINT('Ctrl Pts',(2.46726361058637,-0.487226705758264,-1.88935603669819));
#8140=CARTESIAN_POINT('Ctrl Pts',(2.46940467226192,-0.491911385485655,-1.88900155139795));
#8141=CARTESIAN_POINT('Ctrl Pts',(2.47295453766577,-0.499545678890405,-1.88842506642008));
#8142=CARTESIAN_POINT('Ctrl Pts',(2.47434498083374,-0.502503678900463,-1.88820199553867));
#8143=CARTESIAN_POINT('Ctrl Pts',(2.47708545361274,-0.508271217330545,-1.88776768216505));
#8144=CARTESIAN_POINT('Ctrl Pts',(2.47843434718703,-0.511081237085492,-1.88755637793785));
#8145=CARTESIAN_POINT('Ctrl Pts',(2.4814747551645,-0.517351102284731,-1.88708550310272));
#8146=CARTESIAN_POINT('Ctrl Pts',(2.48317213206339,-0.520808105612696,-1.88682628661972));
#8147=CARTESIAN_POINT('Ctrl Pts',(2.48911617902321,-0.532765577293923,-1.88593088563877));
#8148=CARTESIAN_POINT('Ctrl Pts',(2.49344887670079,-0.541223205602549,-1.88529968282114));
#8149=CARTESIAN_POINT('Ctrl Pts',(2.53336507659208,-0.61687099516147,-1.87966485145346));
#8150=CARTESIAN_POINT('Ctrl Pts',(2.57527987022109,-0.680530520336309,-1.87499314778836));
#8151=CARTESIAN_POINT('Ctrl Pts',(2.66797915093551,-0.795381322042224,-1.86586289647907));
#8152=CARTESIAN_POINT('Ctrl Pts',(2.71788600011217,-0.84683577792764,-1.86142447049118));
#8153=CARTESIAN_POINT('Ctrl Pts',(2.78174873683519,-0.901686943084073,-1.85596479727039));
#8154=CARTESIAN_POINT('Ctrl Pts',(2.79148018452138,-0.909776361245537,-1.85513860171519));
#8155=CARTESIAN_POINT('Ctrl Pts',(2.80727902080868,-0.922484525026616,-1.8538050253309));
#8156=CARTESIAN_POINT('Ctrl Pts',(2.8132643597579,-0.927204011927492,-1.8533015366715));
#8157=CARTESIAN_POINT('Ctrl Pts',(2.82453300300452,-0.935913372547308,-1.85235653442545));
#8158=CARTESIAN_POINT('Ctrl Pts',(2.82980498081155,-0.939917456651158,-1.85191559017098));
#8159=CARTESIAN_POINT('Ctrl Pts',(2.83519496547793,-0.943939964730064,-1.85146586633317));
#8160=CARTESIAN_POINT('Ctrl Pts',(2.83527959262677,-0.944003103666063,-1.85145880557425));
#8161=CARTESIAN_POINT('Ctrl Pts',(2.8354527940327,-0.944132290158664,-1.85144435528945));
#8162=CARTESIAN_POINT('Ctrl Pts',(2.83554136909888,-0.944198336635476,-1.85143696572185));
#8163=CARTESIAN_POINT('Ctrl Pts',(2.8357229870537,-0.94433372128218,-1.85142181445682));
#8164=CARTESIAN_POINT('Ctrl Pts',(2.83581603089438,-0.94440305816482,-1.85141405271051));
#8165=CARTESIAN_POINT('Ctrl Pts',(2.84009552768198,-0.947591183775108,-1.85105707076736));
#8166=CARTESIAN_POINT('Ctrl Pts',(2.84430260203152,-0.950682073104077,-1.85070679058275));
#8167=CARTESIAN_POINT('Ctrl Pts',(2.85334745514616,-0.957235077514597,-1.84995504258621));
#8168=CARTESIAN_POINT('Ctrl Pts',(2.85819117774096,-0.960688700598437,-1.84955326459499));
#8169=CARTESIAN_POINT('Ctrl Pts',(2.87089783940785,-0.969604246685182,-1.84850121891595));
#8170=CARTESIAN_POINT('Ctrl Pts',(2.87880144704677,-0.975007158032249,-1.84784876253529));
#8171=CARTESIAN_POINT('Ctrl Pts',(2.91242640798183,-0.997396606049062,-1.84508033262812));
#8172=CARTESIAN_POINT('Ctrl Pts',(2.93874148677876,-1.01346494208846,-1.84293125248958));
#8173=CARTESIAN_POINT('Ctrl Pts',(3.03829916564307,-1.06901540417245,-1.83485851947973));
#8174=CARTESIAN_POINT('Ctrl Pts',(3.11502681593287,-1.10173421117534,-1.82872715827693));
#8175=CARTESIAN_POINT('Ctrl Pts',(3.2444557225463,-1.14138396422128,-1.81881798355753));
#8176=CARTESIAN_POINT('Ctrl Pts',(3.29533213345813,-1.1533402676166,-1.81503085952394));
#8177=CARTESIAN_POINT('Ctrl Pts',(3.35370407295029,-1.16302032485042,-1.81091549033579));
#8178=CARTESIAN_POINT('Ctrl Pts',(3.36057888706232,-1.16409789350249,-1.81043439770678));
#8179=CARTESIAN_POINT('Ctrl Pts',(3.37108528036573,-1.16564940452219,-1.80970505990988));
#8180=CARTESIAN_POINT('Ctrl Pts',(3.37471004518275,-1.16616742445791,-1.80945450122438));
#8181=CARTESIAN_POINT('Ctrl Pts',(3.38135057827423,-1.16708485146139,-1.80899750398719));
#8182=CARTESIAN_POINT('Ctrl Pts',(3.38436548948961,-1.16748948135267,-1.80879078943669));
#8183=CARTESIAN_POINT('Ctrl Pts',(3.39117569250037,-1.16837662875644,-1.80832557224422));
#8184=CARTESIAN_POINT('Ctrl Pts',(3.39497178976563,-1.16885233837873,-1.80806744772615));
#8185=CARTESIAN_POINT('Ctrl Pts',(3.4047897262201,-1.17003411545846,-1.80740278079862));
#8186=CARTESIAN_POINT('Ctrl Pts',(3.41081490970927,-1.17071220635879,-1.80699772225349));
#8187=CARTESIAN_POINT('Ctrl Pts',(3.45130532084887,-1.1749527326332,-1.80429309236003));
#8188=CARTESIAN_POINT('Ctrl Pts',(3.48591164305039,-1.17703964982149,-1.80206608865917));
#8189=CARTESIAN_POINT('Ctrl Pts',(3.54876402026999,-1.17805139772025,-1.79809409568572));
#8190=CARTESIAN_POINT('Ctrl Pts',(3.57697333670722,-1.17749219207441,-1.79633788044243));
#8191=CARTESIAN_POINT('Ctrl Pts',(3.65301400391627,-1.17324906472264,-1.79161586896054));
#8192=CARTESIAN_POINT('Ctrl Pts',(3.70068297840015,-1.16765601455771,-1.78866702832243));
#8193=CARTESIAN_POINT('Ctrl Pts',(3.80039134664677,-1.14973365439901,-1.78233193561143));
#8194=CARTESIAN_POINT('Ctrl Pts',(3.85219647212967,-1.13673812976287,-1.778940256606));
#8195=CARTESIAN_POINT('Ctrl Pts',(3.91324241519934,-1.1169347600789,-1.77472224660336));
#8196=CARTESIAN_POINT('Ctrl Pts',(3.92349967124746,-1.11345017028379,-1.77400592937972));
#8197=CARTESIAN_POINT('Ctrl Pts',(3.93957104330274,-1.10774193241084,-1.77287089204711));
#8198=CARTESIAN_POINT('Ctrl Pts',(3.94541826155139,-1.10561277748005,-1.77245526212335));
#8199=CARTESIAN_POINT('Ctrl Pts',(3.95633383295694,-1.10153981486296,-1.77167421786054));
#8200=CARTESIAN_POINT('Ctrl Pts',(3.96140617304079,-1.09960710289953,-1.77130917756624));
#8201=CARTESIAN_POINT('Ctrl Pts',(3.97273223910564,-1.095201633497,-1.77048927582917));
#8202=CARTESIAN_POINT('Ctrl Pts',(3.9789784692958,-1.09271025472641,-1.77003380660955));
#8203=CARTESIAN_POINT('Ctrl Pts',(3.9948183226715,-1.08623457137148,-1.76887018649871));
#8204=CARTESIAN_POINT('Ctrl Pts',(4.00438102869661,-1.08217664940954,-1.76815960546792));
#8205=CARTESIAN_POINT('Ctrl Pts',(4.03563143166245,-1.0684249463463,-1.76581014368275));
#8206=CARTESIAN_POINT('Ctrl Pts',(4.05706783446607,-1.05820667714026,-1.7641546497058));
#8207=CARTESIAN_POINT('Ctrl Pts',(4.07816941925732,-1.04735421069218,-1.7624800269618));
#8208=CARTESIAN_POINT('Ctrl Pts',(4.07816926735968,-1.04735428881255,-1.66387346933803));
#8209=CARTESIAN_POINT('Ctrl Pts',(4.06720879457529,-1.0529912171243,-1.66468166682041));
#8210=CARTESIAN_POINT('Ctrl Pts',(4.05615954688209,-1.0584562438635,-1.66548147668066));
#8211=CARTESIAN_POINT('Ctrl Pts',(3.95081656761454,-1.1085165965364,-1.67298556491338));
#8212=CARTESIAN_POINT('Ctrl Pts',(3.85107146589306,-1.14057620227135,-1.67921900281393));
#8213=CARTESIAN_POINT('Ctrl Pts',(3.70750636862628,-1.1664483987049,-1.68842713204318));
#8214=CARTESIAN_POINT('Ctrl Pts',(3.6662561153982,-1.1716478754437,-1.69109333101217));
#8215=CARTESIAN_POINT('Ctrl Pts',(3.61469131315169,-1.17539241730269,-1.69449615845441));
#8216=CARTESIAN_POINT('Ctrl Pts',(3.60455331739282,-1.17599691210483,-1.69516843657527));
#8217=CARTESIAN_POINT('Ctrl Pts',(3.58834038871373,-1.17675335051725,-1.69624933443881));
#8218=CARTESIAN_POINT('Ctrl Pts',(3.58226974978789,-1.17698952688365,-1.69665534808521));
#8219=CARTESIAN_POINT('Ctrl Pts',(3.57075183295034,-1.17734840277255,-1.69742825479403));
#8220=CARTESIAN_POINT('Ctrl Pts',(3.56530498397853,-1.17748028948946,-1.69779485387303));
#8221=CARTESIAN_POINT('Ctrl Pts',(3.55290674205266,-1.17769442537928,-1.69863188744016));
#8222=CARTESIAN_POINT('Ctrl Pts',(3.5459551962096,-1.17775292922565,-1.69910304251821));
#8223=CARTESIAN_POINT('Ctrl Pts',(3.52460097443909,-1.17774358461091,-1.70055623898748));
#8224=CARTESIAN_POINT('Ctrl Pts',(3.51020019158431,-1.17747308790573,-1.7015444624602));
#8225=CARTESIAN_POINT('Ctrl Pts',(3.39981744033141,-1.17337356395114,-1.70918556258179));
#8226=CARTESIAN_POINT('Ctrl Pts',(3.30464033561589,-1.15807896331459,-1.71620325589538));
#8227=CARTESIAN_POINT('Ctrl Pts',(3.17118047132161,-1.11949215940773,-1.72639536639203));
#8228=CARTESIAN_POINT('Ctrl Pts',(3.13064186749986,-1.10533067999223,-1.72953388205583));
#8229=CARTESIAN_POINT('Ctrl Pts',(3.07773670939239,-1.08353901177537,-1.73362270517513));
#8230=CARTESIAN_POINT('Ctrl Pts',(3.06460873182975,-1.07784968770978,-1.73463657268711));
#8231=CARTESIAN_POINT('Ctrl Pts',(3.04248008501204,-1.06777687330759,-1.73634061445457));
#8232=CARTESIAN_POINT('Ctrl Pts',(3.03342591750481,-1.06351536976818,-1.73703640312354));
#8233=CARTESIAN_POINT('Ctrl Pts',(3.02061712131598,-1.05728605250369,-1.73801755906626));
#8234=CARTESIAN_POINT('Ctrl Pts',(3.01681739688841,-1.05541271151954,-1.73830821718948));
#8235=CARTESIAN_POINT('Ctrl Pts',(3.01026757547089,-1.05213946808544,-1.73880844269938));
#8236=CARTESIAN_POINT('Ctrl Pts',(3.00751274636819,-1.05074919814524,-1.73901858715715));
#8237=CARTESIAN_POINT('Ctrl Pts',(3.0017307039087,-1.04780262552922,-1.73945909634588));
#8238=CARTESIAN_POINT('Ctrl Pts',(2.99870474602553,-1.04624401389536,-1.73968931698272));
#8239=CARTESIAN_POINT('Ctrl Pts',(2.99057264262707,-1.0420106189605,-1.74030728991804));
#8240=CARTESIAN_POINT('Ctrl Pts',(2.98547922572389,-1.03931138965471,-1.74069356553669));
#8241=CARTESIAN_POINT('Ctrl Pts',(2.96226964450017,-1.02679247971709,-1.74245109736812));
#8242=CARTESIAN_POINT('Ctrl Pts',(2.94439209618264,-1.01653514714861,-1.74379747133573));
#8243=CARTESIAN_POINT('Ctrl Pts',(2.85433860876496,-0.961675819485388,-1.7505892773089));
#8244=CARTESIAN_POINT('Ctrl Pts',(2.78686020957013,-0.909835205613063,-1.75572663758296));
#8245=CARTESIAN_POINT('Ctrl Pts',(2.68595027687882,-0.813335780464355,-1.7644227735283));
#8246=CARTESIAN_POINT('Ctrl Pts',(2.64906016171293,-0.772772056499071,-1.76788111736715));
#8247=CARTESIAN_POINT('Ctrl Pts',(2.60629376462096,-0.718602046806227,-1.7723880742219));
#8248=CARTESIAN_POINT('Ctrl Pts',(2.59766342985112,-0.707252640307025,-1.77332641156375));
#8249=CARTESIAN_POINT('Ctrl Pts',(2.58515126005506,-0.690163114121485,-1.77473223660069));
#8250=CARTESIAN_POINT('Ctrl Pts',(2.58111040059674,-0.684540619608032,-1.7751936418779));
#8251=CARTESIAN_POINT('Ctrl Pts',(2.57398056398201,-0.674433203603279,-1.77602130128997));
#8252=CARTESIAN_POINT('Ctrl Pts',(2.57087264862487,-0.669961835857362,-1.7763868265982));
#8253=CARTESIAN_POINT('Ctrl Pts',(2.56435408651734,-0.66044338135412,-1.77716372753591));
#8254=CARTESIAN_POINT('Ctrl Pts',(2.56095137473905,-0.655391080581236,-1.77757538558351));
#8255=CARTESIAN_POINT('Ctrl Pts',(2.55193958339063,-0.641783846262471,-1.77868233103703));
#8256=CARTESIAN_POINT('Ctrl Pts',(2.54640262378268,-0.633182012311385,-1.77938024608536));
#8257=CARTESIAN_POINT('Ctrl Pts',(2.52109413313629,-0.592715762147237,-1.78265585148403));
#8258=CARTESIAN_POINT('Ctrl Pts',(2.50274160539872,-0.559994001780803,-1.78528371881742));
#8259=CARTESIAN_POINT('Ctrl Pts',(2.44749598487698,-0.449437143368032,-1.79409891734746));
#8260=CARTESIAN_POINT('Ctrl Pts',(2.41757390006504,-0.368434922198221,-1.80048059439767));
#8261=CARTESIAN_POINT('Ctrl Pts',(2.38989355259196,-0.257409291542364,-1.80881582218067));
#8262=CARTESIAN_POINT('Ctrl Pts',(2.38403177980866,-0.229668696262755,-1.81086321079438));
#8263=CARTESIAN_POINT('Ctrl Pts',(2.3772887773929,-0.190885513886392,-1.81365562251017));
#8264=CARTESIAN_POINT('Ctrl Pts',(2.37555361561142,-0.180002702933001,-1.81443159796881));
#8265=CARTESIAN_POINT('Ctrl Pts',(2.37279471082329,-0.160986159582724,-1.81577256321965));
#8266=CARTESIAN_POINT('Ctrl Pts',(2.37170268528861,-0.152863255524331,-1.81634061688686));
#8267=CARTESIAN_POINT('Ctrl Pts',(2.37021508896511,-0.140849536249192,-1.81717313947139));
#8268=CARTESIAN_POINT('Ctrl Pts',(2.36975398577981,-0.136967298248811,-1.81744099632176));
#8269=CARTESIAN_POINT('Ctrl Pts',(2.36896797372442,-0.130055834766786,-1.81791568526622));
#8270=CARTESIAN_POINT('Ctrl Pts',(2.36863547807778,-0.127027572021349,-1.81812292519326));
#8271=CARTESIAN_POINT('Ctrl Pts',(2.36793635811066,-0.120424137179884,-1.81857319921629));
#8272=CARTESIAN_POINT('Ctrl Pts',(2.36757434493591,-0.11684855962326,-1.818815978365));
#8273=CARTESIAN_POINT('Ctrl Pts',(2.36660784008911,-0.106845813176737,-1.81949241455126));
#8274=CARTESIAN_POINT('Ctrl Pts',(2.36603980413247,-0.100415129805642,-1.81992412617205));
#8275=CARTESIAN_POINT('Ctrl Pts',(2.36304215872024,-0.0629686326593251,
-1.82242132650595));
#8276=CARTESIAN_POINT('Ctrl Pts',(2.36178914359087,-0.03186802865735,-1.82442884456396));
#8277=CARTESIAN_POINT('Ctrl Pts',(2.36173950065284,0.0459379929296807,-1.829365563715));
#8278=CARTESIAN_POINT('Ctrl Pts',(2.36448609594123,0.0925904886839736,-1.8322496682962));
#8279=CARTESIAN_POINT('Ctrl Pts',(2.37933491330058,0.217563020057073,-1.84003412765772));
#8280=CARTESIAN_POINT('Ctrl Pts',(2.39657341976869,0.295015600107938,-1.84493496905921));
#8281=CARTESIAN_POINT('Ctrl Pts',(2.42631095937341,0.3848405948513,-1.85110108312394));
#8282=CARTESIAN_POINT('Ctrl Pts',(2.43146339661839,0.399433560576364,-1.85211805133336));
#8283=CARTESIAN_POINT('Ctrl Pts',(2.43938833097985,0.420544319337278,-1.85361361703527));
#8284=CARTESIAN_POINT('Ctrl Pts',(2.44193459038297,0.427145729013813,-1.85408480430946));
#8285=CARTESIAN_POINT('Ctrl Pts',(2.44655813732052,0.438818336950527,-1.85492441579771));
#8286=CARTESIAN_POINT('Ctrl Pts',(2.44861164599582,0.443898776355467,-1.85529204286599));
#8287=CARTESIAN_POINT('Ctrl Pts',(2.45296908538613,0.454466336746174,-1.85606139942585));
#8288=CARTESIAN_POINT('Ctrl Pts',(2.45527929620904,0.459950683115552,-1.85646333035864));
#8289=CARTESIAN_POINT('Ctrl Pts',(2.46141928971215,0.474223438814875,-1.85751640628447));
#8290=CARTESIAN_POINT('Ctrl Pts',(2.46531492183368,0.482982861669442,-1.85816974850413));
#8291=CARTESIAN_POINT('Ctrl Pts',(2.48365618987188,0.522903792524002,-1.86118056379435));
#8292=CARTESIAN_POINT('Ctrl Pts',(2.49935241787434,0.553468804735726,-1.86358003416854));
#8293=CARTESIAN_POINT('Ctrl Pts',(2.54951603707422,0.641459860708164,-1.87077583092555));
#8294=CARTESIAN_POINT('Ctrl Pts',(2.58756688549411,0.696679239316374,-1.8756796502683));
#8295=CARTESIAN_POINT('Ctrl Pts',(2.66810567521235,0.794551446040531,-1.88498109428815));
#8296=CARTESIAN_POINT('Ctrl Pts',(2.70958277242547,0.837783072776255,-1.88936135877682));
#8297=CARTESIAN_POINT('Ctrl Pts',(2.76165858078287,0.884380661498793,-1.89426200187052));
#8298=CARTESIAN_POINT('Ctrl Pts',(2.7692337839229,0.890986357703456,-1.89496128567395));
#8299=CARTESIAN_POINT('Ctrl Pts',(2.77989802854111,0.900048063570196,-1.89592592050504));
#8300=CARTESIAN_POINT('Ctrl Pts',(2.78291599325332,0.902586521404342,-1.89619674463837));
#8301=CARTESIAN_POINT('Ctrl Pts',(2.78814309287441,0.906938476982544,-1.89666200656722));
#8302=CARTESIAN_POINT('Ctrl Pts',(2.79034615978033,0.908759160055227,-1.89685694706525));
#8303=CARTESIAN_POINT('Ctrl Pts',(2.79500652115651,0.912582162564231,-1.89726685852578));
#8304=CARTESIAN_POINT('Ctrl Pts',(2.79746531079257,0.914582613871321,-1.89748169014809));
#8305=CARTESIAN_POINT('Ctrl Pts',(2.80358423025661,0.919519996773278,-1.89801285172971));
#8306=CARTESIAN_POINT('Ctrl Pts',(2.80725394338851,0.922445065506297,-1.89832835402901));
#8307=CARTESIAN_POINT('Ctrl Pts',(2.82114560724921,0.9333827426984,-1.89951166135836));
#8308=CARTESIAN_POINT('Ctrl Pts',(2.83148282373114,0.94124836479831,-1.90036989352394));
#8309=CARTESIAN_POINT('Ctrl Pts',(2.85835249537242,0.961000356663441,-1.90255025239896));
#8310=CARTESIAN_POINT('Ctrl Pts',(2.87506733994145,0.972632296228121,-1.90385892182145));
#8311=CARTESIAN_POINT('Ctrl Pts',(2.94068114695399,1.01581187999253,-1.90885008290914));
#8312=CARTESIAN_POINT('Ctrl Pts',(2.99159240929114,1.04415412022685,-1.91242235981348));
#8313=CARTESIAN_POINT('Ctrl Pts',(3.1127200429867,1.10027657425597,-1.92068869226887));
#8314=CARTESIAN_POINT('Ctrl Pts',(3.18391629143164,1.12530458544485,-1.92539239021672));
#8315=CARTESIAN_POINT('Ctrl Pts',(3.26709294763647,1.1458564402194,-1.93101549974067));
#8316=CARTESIAN_POINT('Ctrl Pts',(3.27720944777208,1.14821453754936,-1.93170121208814));
#8317=CARTESIAN_POINT('Ctrl Pts',(3.29392371832376,1.15187812233307,-1.93283773257314));
#8318=CARTESIAN_POINT('Ctrl Pts',(3.30050396891324,1.15326148965532,-1.93328608181594));
#8319=CARTESIAN_POINT('Ctrl Pts',(3.31241612433426,1.15565945618393,-1.93409953407945));
#8320=CARTESIAN_POINT('Ctrl Pts',(3.31774391911414,1.15669369634066,-1.93446400765489));
#8321=CARTESIAN_POINT('Ctrl Pts',(3.32919416946672,1.15883442063661,-1.93524880364358));
#8322=CARTESIAN_POINT('Ctrl Pts',(3.33531860239896,1.15992928425166,-1.93566947905483));
#8323=CARTESIAN_POINT('Ctrl Pts',(3.35212676887428,1.16279683415892,-1.93682663542608));
#8324=CARTESIAN_POINT('Ctrl Pts',(3.3628265066516,1.16447072788871,-1.93756617319535));
#8325=CARTESIAN_POINT('Ctrl Pts',(3.42632872900924,1.17350982832436,-1.9419737816769));
#8326=CARTESIAN_POINT('Ctrl Pts',(3.4795514082622,1.17742930915096,-1.94574768365034));
#8327=CARTESIAN_POINT('Ctrl Pts',(3.58083465922324,1.17800283611901,-1.95306801407391));
#8328=CARTESIAN_POINT('Ctrl Pts',(3.62878890282123,1.1753417035512,-1.956592113777));
#8329=CARTESIAN_POINT('Ctrl Pts',(3.70448574153653,1.16648109437251,-1.96218382384049));
#8330=CARTESIAN_POINT('Ctrl Pts',(3.7324008335434,1.16219140627998,-1.96425158999461));
#8331=CARTESIAN_POINT('Ctrl Pts',(3.79416225415088,1.15041376234611,-1.96881017644143));
#8332=CARTESIAN_POINT('Ctrl Pts',(3.82788984446797,1.14242626292964,-1.97128857889477));
#8333=CARTESIAN_POINT('Ctrl Pts',(3.86705082734306,1.13130665409029,-1.97411808040797));
#8334=CARTESIAN_POINT('Ctrl Pts',(3.87286959595853,1.12960578439532,-1.97453722169651));
#8335=CARTESIAN_POINT('Ctrl Pts',(3.8823381901651,1.1267585062086,-1.97521688775381));
#8336=CARTESIAN_POINT('Ctrl Pts',(3.88599593431311,1.1256391357162,-1.97547886183994));
#8337=CARTESIAN_POINT('Ctrl Pts',(3.89255218328838,1.12359775726526,-1.9759473041977));
#8338=CARTESIAN_POINT('Ctrl Pts',(3.89545262032294,1.12268232705864,-1.97615413611128));
#8339=CARTESIAN_POINT('Ctrl Pts',(3.90183641550061,1.12064025962907,-1.97660847690624));
#8340=CARTESIAN_POINT('Ctrl Pts',(3.90531808366598,1.1195086121721,-1.97685569430468));
#8341=CARTESIAN_POINT('Ctrl Pts',(3.91540068528495,1.11617940280244,-1.97757009444221));
#8342=CARTESIAN_POINT('Ctrl Pts',(3.9219876327481,1.11393951899269,-1.9780349161775));
#8343=CARTESIAN_POINT('Ctrl Pts',(3.97779012277,1.09441060402506,-1.98195969015905));
#8344=CARTESIAN_POINT('Ctrl Pts',(4.02583351377513,1.07392542025525,-1.985253356461));
#8345=CARTESIAN_POINT('Ctrl Pts',(4.14646870018387,1.01272491907379,-1.99367970135734));
#8346=CARTESIAN_POINT('Ctrl Pts',(4.2163817871874,0.967396552818754,-1.99873618223097));
#8347=CARTESIAN_POINT('Ctrl Pts',(4.30497128156978,0.895619548860395,-2.00600754950781));
#8348=CARTESIAN_POINT('Ctrl Pts',(4.32822236192517,0.875213300926312,-2.00800807257359));
#8349=CARTESIAN_POINT('Ctrl Pts',(4.35759067701704,0.847316778492877,-2.01067746094749));
#8350=CARTESIAN_POINT('Ctrl Pts',(4.36445823927226,0.840632045031352,-2.01131247663924));
#8351=CARTESIAN_POINT('Ctrl Pts',(4.37545630246784,0.829662208990441,-2.01234761092071));
#8352=CARTESIAN_POINT('Ctrl Pts',(4.37963733664293,0.825428212108018,-2.01274550621023));
#8353=CARTESIAN_POINT('Ctrl Pts',(4.38760684162724,0.817234477347509,-2.0135125265572));
#8354=CARTESIAN_POINT('Ctrl Pts',(4.3914001206636,0.813279615494939,-2.01388143016663));
#8355=CARTESIAN_POINT('Ctrl Pts',(4.40011192760904,0.804068888200546,-2.0147376701685));
#8356=CARTESIAN_POINT('Ctrl Pts',(4.40501010284007,0.798794160870089,-2.01522585004929));
#8357=CARTESIAN_POINT('Ctrl Pts',(4.42045517338131,0.78185289537306,-2.01678718859949));
#8358=CARTESIAN_POINT('Ctrl Pts',(4.43081649732216,0.770020274066548,-2.01786793923086));
#8359=CARTESIAN_POINT('Ctrl Pts',(4.45461110920002,0.741722984126297,-2.02043118988564));
#8360=CARTESIAN_POINT('Ctrl Pts',(4.4678415396249,0.725095662998175,-2.02192111430522));
#8361=CARTESIAN_POINT('Ctrl Pts',(4.51609158939471,0.660971128903884,-2.0276076303749));
#8362=CARTESIAN_POINT('Ctrl Pts',(4.54797162038507,0.611227261504883,-2.03190544218035));
#8363=CARTESIAN_POINT('Ctrl Pts',(4.60968126242485,0.49687190629247,-2.04143738216179));
#8364=CARTESIAN_POINT('Ctrl Pts',(4.637666865582,0.431511327252492,-2.04666771687595));
#8365=CARTESIAN_POINT('Ctrl Pts',(4.66262090364172,0.354729207774051,-2.05232608778339));
#8366=CARTESIAN_POINT('Ctrl Pts',(4.66552604264068,0.345396659632726,-2.05300581402567));
#8367=CARTESIAN_POINT('Ctrl Pts',(4.66942671478405,0.332293425870884,-2.05394797824683));
#8368=CARTESIAN_POINT('Ctrl Pts',(4.67052012076835,0.328552630208662,-2.05421557213698));
#8369=CARTESIAN_POINT('Ctrl Pts',(4.67237993449763,0.322070460370457,-2.05467679946803));
#8370=CARTESIAN_POINT('Ctrl Pts',(4.6731550017904,0.319331636886459,-2.05487091597544));
#8371=CARTESIAN_POINT('Ctrl Pts',(4.67477587322674,0.313523751716991,-2.05528090818236));
#8372=CARTESIAN_POINT('Ctrl Pts',(4.6756191785517,0.310454015882972,-2.05549663488754));
#8373=CARTESIAN_POINT('Ctrl Pts',(4.67769202571387,0.302787031777399,-2.05603309642252));
#8374=CARTESIAN_POINT('Ctrl Pts',(4.6789061867004,0.298185619899464,-2.05635296694511));
#8375=CARTESIAN_POINT('Ctrl Pts',(4.68345081379723,0.280529322081057,-2.05757280381143));
#8376=CARTESIAN_POINT('Ctrl Pts',(4.68658522180455,0.267424412390622,-2.05846241871889));
#8377=CARTESIAN_POINT('Ctrl Pts',(4.69411974484175,0.233348095729801,-2.06074181690958));
#8378=CARTESIAN_POINT('Ctrl Pts',(4.69817385148982,0.21230464175019,-2.06211655363904));
#8379=CARTESIAN_POINT('Ctrl Pts',(4.7108651956415,0.135149674411638,-2.06707563848272));
#8380=CARTESIAN_POINT('Ctrl Pts',(4.7160176858494,0.0785424066773082,-2.07056128549592));
#8381=CARTESIAN_POINT('Ctrl Pts',(4.71845491176731,-0.0532176947246951,
-2.07872190182494));
#8382=CARTESIAN_POINT('Ctrl Pts',(4.71267412206468,-0.12816739160587,-2.08340830867854));
#8383=CARTESIAN_POINT('Ctrl Pts',(4.69802419193994,-0.212294530724692,-2.08901262073761));
#8384=CARTESIAN_POINT('Ctrl Pts',(4.69610527027622,-0.222511652566463,-2.08969885623174));
#8385=CARTESIAN_POINT('Ctrl Pts',(4.69272235996702,-0.239295707541782,-2.09083606503381));
#8386=CARTESIAN_POINT('Ctrl Pts',(4.69133687770206,-0.24587801528933,-2.09128457421128));
#8387=CARTESIAN_POINT('Ctrl Pts',(4.6887317508209,-0.257749275210423,-2.09209819738475));
#8388=CARTESIAN_POINT('Ctrl Pts',(4.68753177703586,-0.263042387226824,-2.09246268071727));
#8389=CARTESIAN_POINT('Ctrl Pts',(4.68487822756179,-0.274383132361227,-2.09324736488095));
#8390=CARTESIAN_POINT('Ctrl Pts',(4.68341324921156,-0.280427900532047,-2.09366791777175));
#8391=CARTESIAN_POINT('Ctrl Pts',(4.67926840384141,-0.296957199951835,-2.09482438870743));
#8392=CARTESIAN_POINT('Ctrl Pts',(4.67649186071571,-0.307416626627177,-2.09556335751577));
#8393=CARTESIAN_POINT('Ctrl Pts',(4.65923185453813,-0.369001073588747,-2.09995818628309));
#8394=CARTESIAN_POINT('Ctrl Pts',(4.64144805162262,-0.41912954585212,-2.10371914225961));
#8395=CARTESIAN_POINT('Ctrl Pts',(4.60123004028068,-0.512034954937896,-2.11103504815499));
#8396=CARTESIAN_POINT('Ctrl Pts',(4.57942904879124,-0.554974571886197,-2.11456849444449));
#8397=CARTESIAN_POINT('Ctrl Pts',(4.5407388631058,-0.620849508269609,-2.12017366499362));
#8398=CARTESIAN_POINT('Ctrl Pts',(4.52553862666622,-0.644717546849175,-2.12224545726128));
#8399=CARTESIAN_POINT('Ctrl Pts',(4.48984118418507,-0.696551057450518,-2.12680858755197));
#8400=CARTESIAN_POINT('Ctrl Pts',(4.46893729297749,-0.724208367484301,-2.12928757302993));
#8401=CARTESIAN_POINT('Ctrl Pts',(4.44297688949179,-0.755576433836276,-2.13211764926407));
#8402=CARTESIAN_POINT('Ctrl Pts',(4.43907558355216,-0.760216983443321,-2.13253681292097));
#8403=CARTESIAN_POINT('Ctrl Pts',(4.4326544468697,-0.767736190521684,-2.13321650785764));
#8404=CARTESIAN_POINT('Ctrl Pts',(4.43015617511438,-0.770632991626648,-2.13347848865331));
#8405=CARTESIAN_POINT('Ctrl Pts',(4.42564622457119,-0.775811152467679,-2.13394693802956));
#8406=CARTESIAN_POINT('Ctrl Pts',(4.42363978820822,-0.77809693143885,-2.13415377030272));
#8407=CARTESIAN_POINT('Ctrl Pts',(4.41919880658925,-0.783116843471275,-2.13460810598139));
#8408=CARTESIAN_POINT('Ctrl Pts',(4.4167603572444,-0.785847411686301,-2.13485531794817));
#8409=CARTESIAN_POINT('Ctrl Pts',(4.40965133867465,-0.793733745118623,-2.13556968649325));
#8410=CARTESIAN_POINT('Ctrl Pts',(4.40494767421071,-0.798859662330359,-2.13603448238837));
#8411=CARTESIAN_POINT('Ctrl Pts',(4.36460601686487,-0.842048311412802,-2.13995780804612));
#8412=CARTESIAN_POINT('Ctrl Pts',(4.32651706350101,-0.877752498900697,-2.14325018980034));
#8413=CARTESIAN_POINT('Ctrl Pts',(4.22196399805932,-0.963462137019431,-2.15167183700275));
#8414=CARTESIAN_POINT('Ctrl Pts',(4.15236205602334,-1.00916473672304,-2.15672494055412));
#8415=CARTESIAN_POINT('Ctrl Pts',(4.07841162190961,-1.04722962021999,-2.16202877425628));
#8416=CARTESIAN_POINT('Ctrl Pts',(4.07829045001313,-1.04729196504753,-2.1620374646626));
#8417=CARTESIAN_POINT('Ctrl Pts',(4.07816926754606,-1.0473542887167,-2.1620461556085));
#8418=CARTESIAN_POINT('Origin',(3.53951905042299,8.32667268468867E-16,0.924367114736157));
#8419=CARTESIAN_POINT('',(4.07816927004253,-1.04735428743277,-2.76055935511047));
#8420=CARTESIAN_POINT('',(4.07816899834492,-1.04735442716575,-2.6623694009368));
#8421=CARTESIAN_POINT('',(4.07816926754759,-1.04735428871592,0.924367114736157));
#8422=CARTESIAN_POINT('Ctrl Pts',(4.07816927004253,-1.04735428743277,-2.76055935511047));
#8423=CARTESIAN_POINT('Ctrl Pts',(4.08356421506408,-1.04457968827797,-2.7601335800222));
#8424=CARTESIAN_POINT('Ctrl Pts',(4.0889381821921,-1.04176316825741,-2.75970976090382));
#8425=CARTESIAN_POINT('Ctrl Pts',(4.10015524195956,-1.03577329741215,-2.75882611700734));
#8426=CARTESIAN_POINT('Ctrl Pts',(4.10599335599956,-1.03259194706589,-2.75836677970824));
#8427=CARTESIAN_POINT('Ctrl Pts',(4.11494742482899,-1.02761382852509,-2.75766352092749));
#8428=CARTESIAN_POINT('Ctrl Pts',(4.11808249898953,-1.02585200272776,-2.75741752642351));
#8429=CARTESIAN_POINT('Ctrl Pts',(4.12385874729127,-1.02257100686899,-2.75696479772187));
#8430=CARTESIAN_POINT('Ctrl Pts',(4.12650209395693,-1.02105594968994,-2.75675782341948));
#8431=CARTESIAN_POINT('Ctrl Pts',(4.13252236890555,-1.01757427095392,-2.75628687613839));
#8432=CARTESIAN_POINT('Ctrl Pts',(4.13589541246349,-1.01560108730532,-2.75602332361189));
#8433=CARTESIAN_POINT('Ctrl Pts',(4.14471215943939,-1.01038434089713,-2.75533507329739));
#8434=CARTESIAN_POINT('Ctrl Pts',(4.15013970282066,-1.00711351829356,-2.75491203938387));
#8435=CARTESIAN_POINT('Ctrl Pts',(4.19375999704026,-0.98034416718816,-2.75151522471897));
#8436=CARTESIAN_POINT('Ctrl Pts',(4.23061342733199,-0.954722710688114,-2.74866372483842));
#8437=CARTESIAN_POINT('Ctrl Pts',(4.31055689783586,-0.892082677190189,-2.74230689562782));
#8438=CARTESIAN_POINT('Ctrl Pts',(4.35261057231845,-0.853928168979994,-2.73883424796629));
#8439=CARTESIAN_POINT('Ctrl Pts',(4.420051454405,-0.783223335717929,-2.7327534570326));
#8440=CARTESIAN_POINT('Ctrl Pts',(4.44677977570563,-0.752099516605598,-2.73017741838101));
#8441=CARTESIAN_POINT('Ctrl Pts',(4.48222070750397,-0.706185417569803,-2.72645139478416));
#8442=CARTESIAN_POINT('Ctrl Pts',(4.49231862592652,-0.692500673860304,-2.72534969240171));
#8443=CARTESIAN_POINT('Ctrl Pts',(4.50974142335659,-0.667786448218728,-2.72337149374909));
#8444=CARTESIAN_POINT('Ctrl Pts',(4.51718338591302,-0.656842916937278,-2.72249938887661));
#8445=CARTESIAN_POINT('Ctrl Pts',(4.5281258286655,-0.640153816361877,-2.72117386781109));
#8446=CARTESIAN_POINT('Ctrl Pts',(4.53176424051348,-0.634499606134734,-2.72072554327277));
#8447=CARTESIAN_POINT('Ctrl Pts',(4.53825205750843,-0.624225044674489,-2.71991206467609));
#8448=CARTESIAN_POINT('Ctrl Pts',(4.54111833285158,-0.619615527238064,-2.71954753954138));
#8449=CARTESIAN_POINT('Ctrl Pts',(4.54720236993772,-0.609678704707029,-2.71876255256481));
#8450=CARTESIAN_POINT('Ctrl Pts',(4.55040996106446,-0.604345397614385,-2.71834173705289));
#8451=CARTESIAN_POINT('Ctrl Pts',(4.55894461604881,-0.589896639534398,-2.71720288834666));
#8452=CARTESIAN_POINT('Ctrl Pts',(4.56419151894789,-0.580734749131844,-2.71648202634855));
#8453=CARTESIAN_POINT('Ctrl Pts',(4.59050099387927,-0.533327585183812,-2.71275748255032));
#8454=CARTESIAN_POINT('Ctrl Pts',(4.60954575662783,-0.49400746775547,-2.7096845237133));
#8455=CARTESIAN_POINT('Ctrl Pts',(4.6574118127644,-0.379350148992415,-2.70077035411512));
#8456=CARTESIAN_POINT('Ctrl Pts',(4.68074320058933,-0.301987209894065,-2.69479568605557));
#8457=CARTESIAN_POINT('Ctrl Pts',(4.70116213171401,-0.196028177435771,-2.6869421640297));
#8458=CARTESIAN_POINT('Ctrl Pts',(4.705397652984,-0.169023596004742,-2.68497042260464));
#8459=CARTESIAN_POINT('Ctrl Pts',(4.70998618472882,-0.131215369309465,-2.68227054088473));
#8460=CARTESIAN_POINT('Ctrl Pts',(4.71113591491256,-0.120518574392876,-2.68151342639212));
#8461=CARTESIAN_POINT('Ctrl Pts',(4.71288899571229,-0.10179758877045,-2.68020177212215));
#8462=CARTESIAN_POINT('Ctrl Pts',(4.71355697154527,-0.0937803083836858,
-2.6796443398046));
#8463=CARTESIAN_POINT('Ctrl Pts',(4.71442533032341,-0.0818862326155545,
-2.67882430828708));
#8464=CARTESIAN_POINT('Ctrl Pts',(4.71468876739008,-0.0780144797335104,
-2.67855846221651));
#8465=CARTESIAN_POINT('Ctrl Pts',(4.71510644160466,-0.0713928088246926,
-2.6781057413469));
#8466=CARTESIAN_POINT('Ctrl Pts',(4.7152701752967,-0.0686435750611099,-2.6779183526165));
#8467=CARTESIAN_POINT('Ctrl Pts',(4.71561998527273,-0.0624010457293062,
-2.67749417834076));
#8468=CARTESIAN_POINT('Ctrl Pts',(4.71580014331346,-0.0589074763591207,
-2.67725772092763));
#8469=CARTESIAN_POINT('Ctrl Pts',(4.71624859182551,-0.0493867073535359,
-2.67661572089007));
#8470=CARTESIAN_POINT('Ctrl Pts',(4.71648614533107,-0.0433580650099662,
-2.67621181963123));
#8471=CARTESIAN_POINT('Ctrl Pts',(4.71745314714548,-0.0128629086343577,
-2.67418077172513));
#8472=CARTESIAN_POINT('Ctrl Pts',(4.71746612650918,0.0116221950734552,-2.67258914283153));
#8473=CARTESIAN_POINT('Ctrl Pts',(4.71334518372222,0.146033717860345,-2.66398032862887));
#8474=CARTESIAN_POINT('Ctrl Pts',(4.69459048873785,0.254966027464975,-2.65742573700325));
#8475=CARTESIAN_POINT('Ctrl Pts',(4.65421625150648,0.380837211625539,-2.64901391847737));
#8476=CARTESIAN_POINT('Ctrl Pts',(4.64684835740117,0.401756826019076,-2.64758864549921));
#8477=CARTESIAN_POINT('Ctrl Pts',(4.63306526629313,0.437625241520115,-2.64508773436085));
#8478=CARTESIAN_POINT('Ctrl Pts',(4.62692272971513,0.452672480738562,-2.64402069230371));
#8479=CARTESIAN_POINT('Ctrl Pts',(4.61757564872198,0.474280739349009,-2.64245988601519));
#8480=CARTESIAN_POINT('Ctrl Pts',(4.61461818840335,0.480947074396737,-2.64197437188364));
#8481=CARTESIAN_POINT('Ctrl Pts',(4.60932433117624,0.492586960732433,-2.64111939192732));
#8482=CARTESIAN_POINT('Ctrl Pts',(4.60701466146038,0.497572478422809,-2.64075083973942));
#8483=CARTESIAN_POINT('Ctrl Pts',(4.60245528306627,0.50723621060023,-2.64003177548476));
#8484=CARTESIAN_POINT('Ctrl Pts',(4.60020936055344,0.511916079567099,-2.63968139955495));
#8485=CARTESIAN_POINT('Ctrl Pts',(4.59410323254831,0.524426818613807,-2.63873885431123));
#8486=CARTESIAN_POINT('Ctrl Pts',(4.59018682912239,0.532229740768374,-2.63814476446553));
#8487=CARTESIAN_POINT('Ctrl Pts',(4.57521163717373,0.561256319106046,-2.63591088128483));
#8488=CARTESIAN_POINT('Ctrl Pts',(4.56359419959941,0.582183592275196,-2.63425190280769));
#8489=CARTESIAN_POINT('Ctrl Pts',(4.4998366670267,0.689214137826032,-2.6255052445153));
#8490=CARTESIAN_POINT('Ctrl Pts',(4.43745757934006,0.768717079948001,-2.61805178385223));
#8491=CARTESIAN_POINT('Ctrl Pts',(4.34455460439164,0.860172994016073,-2.60854445056867));
#8492=CARTESIAN_POINT('Ctrl Pts',(4.3225729302063,0.880231038859097,-2.60639259063669));
#8493=CARTESIAN_POINT('Ctrl Pts',(4.29116808863293,0.90677899388292,-2.60347296115957));
#8494=CARTESIAN_POINT('Ctrl Pts',(4.28237593907986,0.913995669937662,-2.60267143926328));
#8495=CARTESIAN_POINT('Ctrl Pts',(4.26691204521181,0.926317995377002,-2.60129086879716));
#8496=CARTESIAN_POINT('Ctrl Pts',(4.26028778320911,0.931481637672731,-2.60070851745956));
#8497=CARTESIAN_POINT('Ctrl Pts',(4.2504686251344,0.938968240099166,-2.59985916122319));
#8498=CARTESIAN_POINT('Ctrl Pts',(4.2473165538372,0.941346561579019,-2.59958857472766));
#8499=CARTESIAN_POINT('Ctrl Pts',(4.24170856380623,0.945533845344303,-2.59911089964739));
#8500=CARTESIAN_POINT('Ctrl Pts',(4.23925751352847,0.947349169739976,-2.59890338303929));
#8501=CARTESIAN_POINT('Ctrl Pts',(4.23392488638581,0.951266691936722,-2.5984546341473));
#8502=CARTESIAN_POINT('Ctrl Pts',(4.23104079774334,0.953365332931716,-2.59821364156447));
#8503=CARTESIAN_POINT('Ctrl Pts',(4.22300853917452,0.959154473199115,-2.59754706023847));
#8504=CARTESIAN_POINT('Ctrl Pts',(4.2178399709548,0.96281665848811,-2.59712332728447));
#8505=CARTESIAN_POINT('Ctrl Pts',(4.18889814295964,0.982974626727414,-2.59477783334878));
#8506=CARTESIAN_POINT('Ctrl Pts',(4.1645506575597,0.998633128590652,-2.59290608158786));
#8507=CARTESIAN_POINT('Ctrl Pts',(4.05645625592928,1.06264728489848,-2.58491329665853));
#8508=CARTESIAN_POINT('Ctrl Pts',(3.96751097215398,1.10148473096663,-2.57910429978621));
#8509=CARTESIAN_POINT('Ctrl Pts',(3.83593711864401,1.14055954851559,-2.57043258994896));
#8510=CARTESIAN_POINT('Ctrl Pts',(3.7964938881081,1.15008832062027,-2.56782827087683));
#8511=CARTESIAN_POINT('Ctrl Pts',(3.74672745131903,1.15942290482044,-2.56449511859617));
#8512=CARTESIAN_POINT('Ctrl Pts',(3.73679092794977,1.16115485168715,-2.56382737512894));
#8513=CARTESIAN_POINT('Ctrl Pts',(3.72085012638427,1.1637228342143,-2.56275200857603));
#8514=CARTESIAN_POINT('Ctrl Pts',(3.71485936497829,1.16464053070163,-2.56234694340977));
#8515=CARTESIAN_POINT('Ctrl Pts',(3.70346607023002,1.1662959172512,-2.56157470255183));
#8516=CARTESIAN_POINT('Ctrl Pts',(3.69806495991129,1.16704240915702,-2.56120781217038));
#8517=CARTESIAN_POINT('Ctrl Pts',(3.68573763194173,1.1686590252291,-2.56036851394296));
#8518=CARTESIAN_POINT('Ctrl Pts',(3.67880852551826,1.16950512154891,-2.55989537153765));
#8519=CARTESIAN_POINT('Ctrl Pts',(3.65741429672787,1.17192469246386,-2.55843003346276));
#8520=CARTESIAN_POINT('Ctrl Pts',(3.64292768985563,1.17329169193208,-2.55743150569861));
#8521=CARTESIAN_POINT('Ctrl Pts',(3.533990830082,1.18153818006976,-2.54987221544559));
#8522=CARTESIAN_POINT('Ctrl Pts',(3.43906116836297,1.17726987968544,-2.54295841446134));
#8523=CARTESIAN_POINT('Ctrl Pts',(3.30254460625993,1.15449184839412,-2.5328033230465));
#8524=CARTESIAN_POINT('Ctrl Pts',(3.25983209947081,1.14489475278669,-2.52960192552092));
#8525=CARTESIAN_POINT('Ctrl Pts',(3.2038296428696,1.1289894151128,-2.52544026421777));
#8526=CARTESIAN_POINT('Ctrl Pts',(3.18998236256407,1.12477936606106,-2.52441437887715));
#8527=CARTESIAN_POINT('Ctrl Pts',(3.16661424906073,1.11720139229929,-2.52269228422701));
#8528=CARTESIAN_POINT('Ctrl Pts',(3.15705296383702,1.11396438519246,-2.52199031327273));
#8529=CARTESIAN_POINT('Ctrl Pts',(3.14352500969638,1.10918972998623,-2.52100202047301));
#8530=CARTESIAN_POINT('Ctrl Pts',(3.1395235459356,1.10775301182045,-2.5207103062204));
#8531=CARTESIAN_POINT('Ctrl Pts',(3.13262880019684,1.10523523528111,-2.52020883558979));
#8532=CARTESIAN_POINT('Ctrl Pts',(3.12973185657808,1.10416441606982,-2.51999849447311));
#8533=CARTESIAN_POINT('Ctrl Pts',(3.12365672845941,1.10189161735747,-2.51955818469412));
#8534=CARTESIAN_POINT('Ctrl Pts',(3.12047950397054,1.10068727006229,-2.51932835608941));
#8535=CARTESIAN_POINT('Ctrl Pts',(3.11195296446409,1.09741295943522,-2.51871267117988));
#8536=CARTESIAN_POINT('Ctrl Pts',(3.10661340102892,1.09531760847428,-2.51832827245048));
#8537=CARTESIAN_POINT('Ctrl Pts',(3.08243820263907,1.0856263762999,-2.51659224013371));
#8538=CARTESIAN_POINT('Ctrl Pts',(3.06378442333429,1.07758257876514,-2.51526475272673));
#8539=CARTESIAN_POINT('Ctrl Pts',(2.96820091616922,1.03339915209238,-2.50847899445197));
#8540=CARTESIAN_POINT('Ctrl Pts',(2.89513471994717,0.989489723408842,-2.50333256587488));
#8541=CARTESIAN_POINT('Ctrl Pts',(2.78367003400686,0.904878534813775,-2.4946175995915));
#8542=CARTESIAN_POINT('Ctrl Pts',(2.74229610113198,0.868646879644988,-2.49114931914335));
#8543=CARTESIAN_POINT('Ctrl Pts',(2.69354509354465,0.819528540735376,-2.48663029228173));
#8544=CARTESIAN_POINT('Ctrl Pts',(2.68367149815664,0.80921190267889,-2.48569053034149));
#8545=CARTESIAN_POINT('Ctrl Pts',(2.6692893077337,0.793626653985059,-2.48428293920833));
#8546=CARTESIAN_POINT('Ctrl Pts',(2.66463548298678,0.788493380421825,-2.48382121432477));
#8547=CARTESIAN_POINT('Ctrl Pts',(2.65640473565994,0.77925210026199,-2.48299315132483));
#8548=CARTESIAN_POINT('Ctrl Pts',(2.65281047731249,0.775159747003033,-2.48262754415319));
#8549=CARTESIAN_POINT('Ctrl Pts',(2.64525776447829,0.766439106564089,-2.48185064793042));
#8550=CARTESIAN_POINT('Ctrl Pts',(2.64130657679308,0.761804765949063,-2.48143907760195));
#8551=CARTESIAN_POINT('Ctrl Pts',(2.63082066674637,0.749310872098327,-2.48033280208272));
#8552=CARTESIAN_POINT('Ctrl Pts',(2.62435214513884,0.74139669515883,-2.47963547541483));
#8553=CARTESIAN_POINT('Ctrl Pts',(2.5947125794674,0.704153978543222,-2.476368939241));
#8554=CARTESIAN_POINT('Ctrl Pts',(2.57284537383398,0.673820129410011,-2.47374990132801));
#8555=CARTESIAN_POINT('Ctrl Pts',(2.49950212062077,0.561144488798077,-2.46416186660919));
#8556=CARTESIAN_POINT('Ctrl Pts',(2.45680926275963,0.473554783146209,-2.45692639003369));
#8557=CARTESIAN_POINT('Ctrl Pts',(2.41845313384539,0.361606441853206,-2.44837183985799));
#8558=CARTESIAN_POINT('Ctrl Pts',(2.41210147768409,0.341288344614352,-2.44684725501282));
#8559=CARTESIAN_POINT('Ctrl Pts',(2.40265113297913,0.307906157670654,-2.4443988125825));
#8560=CARTESIAN_POINT('Ctrl Pts',(2.39921905502597,0.29494206605236,-2.44346159659141));
#8561=CARTESIAN_POINT('Ctrl Pts',(2.39487179095101,0.277309001589889,-2.44220774981465));
#8562=CARTESIAN_POINT('Ctrl Pts',(2.39376251237781,0.272689545910477,-2.44188120048683));
#8563=CARTESIAN_POINT('Ctrl Pts',(2.39195694067214,0.264964888459799,-2.44133850372109));
#8564=CARTESIAN_POINT('Ctrl Pts',(2.39124523623644,0.261863392333106,-2.44112150903588));
#8565=CARTESIAN_POINT('Ctrl Pts',(2.38992030687273,0.255980280846619,-2.44071165503247));
#8566=CARTESIAN_POINT('Ctrl Pts',(2.38930458983194,0.253199270222425,-2.44051865234454));
#8567=CARTESIAN_POINT('Ctrl Pts',(2.38786888939029,0.246601317977667,-2.44006244603685));
#8568=CARTESIAN_POINT('Ctrl Pts',(2.38705777695381,0.242782449253529,-2.43979973602712));
#8569=CARTESIAN_POINT('Ctrl Pts',(2.38427498531351,0.229352293812495,-2.43888031773015));
#8570=CARTESIAN_POINT('Ctrl Pts',(2.382404365146,0.219720151889708,-2.43822894889428));
#8571=CARTESIAN_POINT('Ctrl Pts',(2.36815362126143,0.141103268443537,-2.43296950297869));
#8572=CARTESIAN_POINT('Ctrl Pts',(2.36183187491525,0.0711529470005039,-2.42864081734748));
#8573=CARTESIAN_POINT('Ctrl Pts',(2.36169695181929,-0.0805315584501841,
-2.41925791481658));
#8574=CARTESIAN_POINT('Ctrl Pts',(2.37010009790866,-0.161887316300625,-2.41421634373057));
#8575=CARTESIAN_POINT('Ctrl Pts',(2.3900025117513,-0.256795913985343,-2.40789614574099));
#8576=CARTESIAN_POINT('Ctrl Pts',(2.39345986337707,-0.27181007742759,-2.40688361418846));
#8577=CARTESIAN_POINT('Ctrl Pts',(2.39893041520147,-0.29360266190163,-2.40539333010729));
#8578=CARTESIAN_POINT('Ctrl Pts',(2.40071180265195,-0.300438024658899,-2.40492291151059));
#8579=CARTESIAN_POINT('Ctrl Pts',(2.40398385702866,-0.312545842562442,-2.40408413437813));
#8580=CARTESIAN_POINT('Ctrl Pts',(2.40545004435078,-0.317824742393573,-2.40371656689995));
#8581=CARTESIAN_POINT('Ctrl Pts',(2.40858747259038,-0.32882263819139,-2.4029467891541));
#8582=CARTESIAN_POINT('Ctrl Pts',(2.41026538261947,-0.334539553161827,-2.40254437373673));
#8583=CARTESIAN_POINT('Ctrl Pts',(2.41476453461829,-0.349449291259322,-2.40148879772812));
#8584=CARTESIAN_POINT('Ctrl Pts',(2.41765506322126,-0.3586205692598,-2.40083342119573));
#8585=CARTESIAN_POINT('Ctrl Pts',(2.43148241528656,-0.400689023674756,-2.39779842541338));
#8586=CARTESIAN_POINT('Ctrl Pts',(2.44375508470654,-0.433125597620229,-2.395375976772));
#8587=CARTESIAN_POINT('Ctrl Pts',(2.48433056127798,-0.527552774009048,-2.38807179302228));
#8588=CARTESIAN_POINT('Ctrl Pts',(2.51659776826546,-0.587677489052723,-2.38307831972427));
#8589=CARTESIAN_POINT('Ctrl Pts',(2.56843384221588,-0.666930334565932,-2.3761297263357));
#8590=CARTESIAN_POINT('Ctrl Pts',(2.58374358041938,-0.688691422818852,-2.37418083962557));
#8591=CARTESIAN_POINT('Ctrl Pts',(2.60684701081892,-0.719274278288497,-2.37139698512298));
#8592=CARTESIAN_POINT('Ctrl Pts',(2.61405623191907,-0.728526736914997,-2.37054858735982));
#8593=CARTESIAN_POINT('Ctrl Pts',(2.63782749577928,-0.758112841823712,-2.36781895349618));
#8594=CARTESIAN_POINT('Ctrl Pts',(2.65493203316285,-0.77800307858689,-2.36595756536672));
#8595=CARTESIAN_POINT('Ctrl Pts',(2.67685714137634,-0.801840022995481,-2.36370986225827));
#8596=CARTESIAN_POINT('Ctrl Pts',(2.68106201494558,-0.806340197523177,-2.36328474478683));
#8597=CARTESIAN_POINT('Ctrl Pts',(2.68773013180696,-0.813365317289847,-2.36262016660146));
#8598=CARTESIAN_POINT('Ctrl Pts',(2.69016967348418,-0.8159124572917,-2.36237900973142));
#8599=CARTESIAN_POINT('Ctrl Pts',(2.69453135392328,-0.820425752264362,-2.36195141279864));
#8600=CARTESIAN_POINT('Ctrl Pts',(2.69644893347515,-0.822396133487094,-2.3617646421664));
#8601=CARTESIAN_POINT('Ctrl Pts',(2.70106050587343,-0.827101607451648,-2.36131836561036));
#8602=CARTESIAN_POINT('Ctrl Pts',(2.70376098991346,-0.829830262953716,-2.36105936447165));
#8603=CARTESIAN_POINT('Ctrl Pts',(2.71201107194797,-0.838085285069375,-2.36027497813601));
#8604=CARTESIAN_POINT('Ctrl Pts',(2.71760262960361,-0.843569679865628,-2.35975271542219));
#8605=CARTESIAN_POINT('Ctrl Pts',(2.73073995524549,-0.856200580080385,-2.358546021087));
#8606=CARTESIAN_POINT('Ctrl Pts',(2.73832653224468,-0.863303899720868,-2.35786442975006));
#8607=CARTESIAN_POINT('Ctrl Pts',(2.76517301860309,-0.887781523375701,-2.35550092673505));
#8608=CARTESIAN_POINT('Ctrl Pts',(2.78491299221078,-0.904620189321162,-2.35384824180508));
#8609=CARTESIAN_POINT('Ctrl Pts',(2.86563192122239,-0.968992784711524,-2.34734669568882));
#8610=CARTESIAN_POINT('Ctrl Pts',(2.9306690175001,-1.01112478070619,-2.34265324003624));
#8611=CARTESIAN_POINT('Ctrl Pts',(3.04248362075683,-1.06883348508297,-2.33476087469136));
#8612=CARTESIAN_POINT('Ctrl Pts',(3.08692875914478,-1.08839809462577,-2.33166698148866));
#8613=CARTESIAN_POINT('Ctrl Pts',(3.14261604257234,-1.10890956936754,-2.32776766192681));
#8614=CARTESIAN_POINT('Ctrl Pts',(3.15283291597908,-1.1125134836653,-2.32705148179739));
#8615=CARTESIAN_POINT('Ctrl Pts',(3.16905424463737,-1.11798497585398,-2.32591248050451));
#8616=CARTESIAN_POINT('Ctrl Pts',(3.17502659879194,-1.11994635080558,-2.325492718003));
#8617=CARTESIAN_POINT('Ctrl Pts',(3.18617977620866,-1.12351049263088,-2.32470793492378));
#8618=CARTESIAN_POINT('Ctrl Pts',(3.19135654397516,-1.12512547619105,-2.32434332179092));
#8619=CARTESIAN_POINT('Ctrl Pts',(3.20289765849856,-1.12863865244498,-2.32352957321124));
#8620=CARTESIAN_POINT('Ctrl Pts',(3.20926723983762,-1.13051886661665,-2.32307987142123));
#8621=CARTESIAN_POINT('Ctrl Pts',(3.22798301238288,-1.13587184345754,-2.32175659594079));
#8622=CARTESIAN_POINT('Ctrl Pts',(3.24037009594021,-1.13919683473104,-2.3208783417576));
#8623=CARTESIAN_POINT('Ctrl Pts',(3.32523751935868,-1.160497699507,-2.31484238902654));
#8624=CARTESIAN_POINT('Ctrl Pts',(3.39921806453577,-1.17174375096012,-2.30947146078027));
#8625=CARTESIAN_POINT('Ctrl Pts',(3.55574322131604,-1.18049793974909,-2.29799821274768));
#8626=CARTESIAN_POINT('Ctrl Pts',(3.63799406062758,-1.17649616270969,-2.2919071136245));
#8627=CARTESIAN_POINT('Ctrl Pts',(3.72835482879296,-1.16255004039011,-2.28550938483745));
#8628=CARTESIAN_POINT('Ctrl Pts',(3.73752898362188,-1.16102266447757,-2.28486348988142));
#8629=CARTESIAN_POINT('Ctrl Pts',(3.75069102938883,-1.15867080016363,-2.28394299616137));
#8630=CARTESIAN_POINT('Ctrl Pts',(3.75469396270291,-1.15793410270981,-2.28366387221191));
#8631=CARTESIAN_POINT('Ctrl Pts',(3.76171161989338,-1.15660492955911,-2.28317607173157));
#8632=CARTESIAN_POINT('Ctrl Pts',(3.76472796135646,-1.1560213874877,-2.28296690780228));
#8633=CARTESIAN_POINT('Ctrl Pts',(3.77112722427484,-1.15475738688068,-2.28252425789375));
#8634=CARTESIAN_POINT('Ctrl Pts',(3.77450946342174,-1.15407386042605,-2.28229094443978));
#8635=CARTESIAN_POINT('Ctrl Pts',(3.78374049293312,-1.15216607118534,-2.28165580593086));
#8636=CARTESIAN_POINT('Ctrl Pts',(3.78958314567294,-1.15091212547518,-2.28125560119713));
#8637=CARTESIAN_POINT('Ctrl Pts',(3.82109279913945,-1.14389826612583,-2.27910575677516));
#8638=CARTESIAN_POINT('Ctrl Pts',(3.846573064171,-1.1373236548044,-2.27739769368109));
#8639=CARTESIAN_POINT('Ctrl Pts',(3.94312692874197,-1.10892792673493,-2.27096787394003));
#8640=CARTESIAN_POINT('Ctrl Pts',(4.01221342001257,-1.08127513956293,-2.2664476753402));
#8641=CARTESIAN_POINT('Ctrl Pts',(4.07816947157471,-1.04735418378554,-2.26183802367812));
#8642=CARTESIAN_POINT('',(2.3617693920187,-0.000311670151205854,-2.32461248197894));
#8643=CARTESIAN_POINT('Ctrl Pts',(4.07816926754606,-1.0473542887167,-2.1620461556085));
#8644=CARTESIAN_POINT('Ctrl Pts',(4.05073123587279,-1.06146556116525,-2.16401395222577));
#8645=CARTESIAN_POINT('Ctrl Pts',(4.0227513290571,-1.07449213620125,-2.16600987267141));
#8646=CARTESIAN_POINT('Ctrl Pts',(3.98544740015946,-1.09010776812031,-2.16867491911241));
#8647=CARTESIAN_POINT('Ctrl Pts',(3.9765560990177,-1.09370272397537,-2.16931037608124));
#8648=CARTESIAN_POINT('Ctrl Pts',(3.96207729854973,-1.09935208867815,-2.17034605191304));
#8649=CARTESIAN_POINT('Ctrl Pts',(3.95651626700993,-1.10147347090154,-2.17074404308492));
#8650=CARTESIAN_POINT('Ctrl Pts',(3.94580518148661,-1.10546671915603,-2.17151112655334));
#8651=CARTESIAN_POINT('Ctrl Pts',(3.9406576631559,-1.10734497745289,-2.17187999651113));
#8652=CARTESIAN_POINT('Ctrl Pts',(3.92872118666874,-1.11160628245965,-2.17273597810724));
#8653=CARTESIAN_POINT('Ctrl Pts',(3.92192318277157,-1.11396315273396,-2.17322393158914));
#8654=CARTESIAN_POINT('Ctrl Pts',(3.90021537039549,-1.12126713977771,-2.17478379865724));
#8655=CARTESIAN_POINT('Ctrl Pts',(3.88522852241034,-1.12597813197835,-2.1758632840228));
#8656=CARTESIAN_POINT('Ctrl Pts',(3.84979136327779,-1.13634334630803,-2.17842299651224));
#8657=CARTESIAN_POINT('Ctrl Pts',(3.82927415636777,-1.14174734116409,-2.17991062022575));
#8658=CARTESIAN_POINT('Ctrl Pts',(3.75132958942065,-1.16004083512243,-2.18558355348006));
#8659=CARTESIAN_POINT('Ctrl Pts',(3.693114645676,-1.16917297213438,-2.18986954975729));
#8660=CARTESIAN_POINT('Ctrl Pts',(3.56352584634092,-1.17965434944569,-2.19940625143114));
#8661=CARTESIAN_POINT('Ctrl Pts',(3.49220386942015,-1.17895029048881,-2.2046537977874));
#8662=CARTESIAN_POINT('Ctrl Pts',(3.41162541470622,-1.1708263485179,-2.21032971493028));
#8663=CARTESIAN_POINT('Ctrl Pts',(3.401886185522,-1.16972147562266,-2.21101132249905));
#8664=CARTESIAN_POINT('Ctrl Pts',(3.38830852202504,-1.16800921234235,-2.21195436499361));
#8665=CARTESIAN_POINT('Ctrl Pts',(3.38445790451514,-1.16750425528745,-2.21222100019463));
#8666=CARTESIAN_POINT('Ctrl Pts',(3.37779285987008,-1.16659666723653,-2.21268103350148));
#8667=CARTESIAN_POINT('Ctrl Pts',(3.37497729212429,-1.16620287897618,-2.21287490887173));
#8668=CARTESIAN_POINT('Ctrl Pts',(3.36900778119692,-1.1653459276259,-2.21328494394368));
#8669=CARTESIAN_POINT('Ctrl Pts',(3.36585423437264,-1.16488014669123,-2.21350095173145));
#8670=CARTESIAN_POINT('Ctrl Pts',(3.35797752004533,-1.16368405343863,-2.21403905898488));
#8671=CARTESIAN_POINT('Ctrl Pts',(3.35325677320652,-1.16293777543066,-2.21436028270096));
#8672=CARTESIAN_POINT('Ctrl Pts',(3.33509476144177,-1.15995320822496,-2.21559164140253));
#8673=CARTESIAN_POINT('Ctrl Pts',(3.3216875660417,-1.15751035369551,-2.21649117263143));
#8674=CARTESIAN_POINT('Ctrl Pts',(3.28698142459966,-1.15056230603112,-2.21880218404987));
#8675=CARTESIAN_POINT('Ctrl Pts',(3.26575898043834,-1.14569822064141,-2.22019808965914));
#8676=CARTESIAN_POINT('Ctrl Pts',(3.14379313867637,-1.11416122386063,-2.22818307382671));
#8677=CARTESIAN_POINT('Ctrl Pts',(3.04681164316509,-1.07480035543966,-2.23442602583379));
#8678=CARTESIAN_POINT('Ctrl Pts',(2.92954936891031,-1.00795739017186,-2.24303561309381));
#8679=CARTESIAN_POINT('Ctrl Pts',(2.90343689296424,-0.991685608863961,-2.24502553812767));
#8680=CARTESIAN_POINT('Ctrl Pts',(2.87007837176057,-0.96903856849742,-2.24768277519579));
#8681=CARTESIAN_POINT('Ctrl Pts',(2.86222995372842,-0.963569426720093,-2.24831663448374));
#8682=CARTESIAN_POINT('Ctrl Pts',(2.84961214042061,-0.954546426283682,-2.24935034965688));
#8683=CARTESIAN_POINT('Ctrl Pts',(2.84480141064312,-0.951050904623204,-2.24974799373266));
#8684=CARTESIAN_POINT('Ctrl Pts',(2.83580388540701,-0.944408523379313,-2.250498486953));
#8685=CARTESIAN_POINT('Ctrl Pts',(2.83161119403172,-0.941269864515296,-2.25085101504504));
#8686=CARTESIAN_POINT('Ctrl Pts',(2.82736461161161,-0.938046441628834,-2.25121098673338));
#8687=CARTESIAN_POINT('Ctrl Pts',(2.82728959612224,-0.937989485973974,-2.25121734653013));
#8688=CARTESIAN_POINT('Ctrl Pts',(2.82714379967878,-0.937878762169231,-2.25122970892862));
#8689=CARTESIAN_POINT('Ctrl Pts',(2.82707301797973,-0.937824995005365,-2.25123571149178));
#8690=CARTESIAN_POINT('Ctrl Pts',(2.82170413031255,-0.933745724259574,-2.25169107689551));
#8691=CARTESIAN_POINT('Ctrl Pts',(2.81644032390447,-0.929675475216095,-2.25214217511832));
#8692=CARTESIAN_POINT('Ctrl Pts',(2.8052578576919,-0.920876188440969,-2.25311062189075));
#8693=CARTESIAN_POINT('Ctrl Pts',(2.79934979658597,-0.916134228491322,-2.25362846614165));
#8694=CARTESIAN_POINT('Ctrl Pts',(2.78378447258346,-0.903392255485656,-2.25500950386272));
#8695=CARTESIAN_POINT('Ctrl Pts',(2.7742087560986,-0.895294617426583,-2.25587652190288));
#8696=CARTESIAN_POINT('Ctrl Pts',(2.71438152075821,-0.843040923127297,-2.26140644628375));
#8697=CARTESIAN_POINT('Ctrl Pts',(2.66784692635009,-0.794830251945468,-2.26623266981025));
#8698=CARTESIAN_POINT('Ctrl Pts',(2.57427819926975,-0.67973528537226,-2.27709019012116));
#8699=CARTESIAN_POINT('Ctrl Pts',(2.52958757441272,-0.611367573177025,-2.2831299420389));
#8700=CARTESIAN_POINT('Ctrl Pts',(2.48802228786831,-0.530600958041598,-2.28948697036161));
#8701=CARTESIAN_POINT('Ctrl Pts',(2.48383500333495,-0.522220283805889,-2.29013766994944));
#8702=CARTESIAN_POINT('Ctrl Pts',(2.47796741466395,-0.510117483123086,-2.29106370037916));
#8703=CARTESIAN_POINT('Ctrl Pts',(2.47620589792119,-0.50643544794795,-2.29134363020673));
#8704=CARTESIAN_POINT('Ctrl Pts',(2.47315155044716,-0.499964862595573,-2.291832325748));
#8705=CARTESIAN_POINT('Ctrl Pts',(2.4718504413181,-0.497180300149088,-2.29204158487014));
#8706=CARTESIAN_POINT('Ctrl Pts',(2.46911472805537,-0.491265209968073,-2.29248385705357));
#8707=CARTESIAN_POINT('Ctrl Pts',(2.46768294128971,-0.488133461044548,-2.29271670158411));
#8708=CARTESIAN_POINT('Ctrl Pts',(2.46381687895138,-0.479578189661555,-2.29334932101888));
#8709=CARTESIAN_POINT('Ctrl Pts',(2.46140985699213,-0.474142354593266,-2.29374749673964));
#8710=CARTESIAN_POINT('Ctrl Pts',(2.44875489332431,-0.444968659549882,-2.29586555627874));
#8711=CARTESIAN_POINT('Ctrl Pts',(2.43924871055521,-0.420914440670272,-2.29754530190582));
#8712=CARTESIAN_POINT('Ctrl Pts',(2.39454646724692,-0.295906384200299,-2.30603247300616));
#8713=CARTESIAN_POINT('Ctrl Pts',(2.37242132185075,-0.190812240438875,-2.3124152820028));
#8714=CARTESIAN_POINT('Ctrl Pts',(2.36278079051669,-0.0562588296494679,
-2.3209841257008));
#8715=CARTESIAN_POINT('Ctrl Pts',(2.36177651634134,-0.0282893539699714,
-2.32278333724587));
#8716=CARTESIAN_POINT('Ctrl Pts',(2.36176909189499,-0.000312549685508988,
-2.32461190331719));
#8717=CARTESIAN_POINT('Ctrl Pts',(2.36176909165296,-0.000311636306741051,
-2.32461196301571));
#8718=CARTESIAN_POINT('Ctrl Pts',(2.36176714494032,0.00704546771741885,
-2.32509282406184));
#8719=CARTESIAN_POINT('Ctrl Pts',(2.36183413518344,0.014402326824858,-2.32557564586804));
#8720=CARTESIAN_POINT('Ctrl Pts',(2.36209751886435,0.0286567381129853,-2.3265152767732));
#8721=CARTESIAN_POINT('Ctrl Pts',(2.3622856101691,0.0355541200457753,-2.32697181785634));
#8722=CARTESIAN_POINT('Ctrl Pts',(2.36272874286164,0.0478407777693243,-2.32778862113952));
#8723=CARTESIAN_POINT('Ctrl Pts',(2.36296023165427,0.0532307462102336,-2.32814815608438));
#8724=CARTESIAN_POINT('Ctrl Pts',(2.36348635219762,0.0637882783698974,-2.32885486723026));
#8725=CARTESIAN_POINT('Ctrl Pts',(2.36377803381177,0.0689558710647757,-2.32920194478199));
#8726=CARTESIAN_POINT('Ctrl Pts',(2.36446929188937,0.079917838391069,-2.32994074744835));
#8727=CARTESIAN_POINT('Ctrl Pts',(2.36487768690705,0.0857114984080915,-2.33033273623927));
#8728=CARTESIAN_POINT('Ctrl Pts',(2.36602230913766,0.100399777229516,-2.33133047839124));
#8729=CARTESIAN_POINT('Ctrl Pts',(2.36681680914094,0.1092893533962,-2.33193801732483));
#8730=CARTESIAN_POINT('Ctrl Pts',(2.37026510927065,0.143484000467958,-2.33428971046191));
#8731=CARTESIAN_POINT('Ctrl Pts',(2.3736374575342,0.168707962199148,-2.33605579014994));
#8732=CARTESIAN_POINT('Ctrl Pts',(2.39405402143647,0.291090120934524,-2.34478381037125));
#8733=CARTESIAN_POINT('Ctrl Pts',(2.42244047808055,0.385944445135463,-2.35208776465424));
#8734=CARTESIAN_POINT('Ctrl Pts',(2.4800226550828,0.516220521963633,-2.36247573798136));
#8735=CARTESIAN_POINT('Ctrl Pts',(2.49996870468376,0.555294700243881,-2.36563471135706));
#8736=CARTESIAN_POINT('Ctrl Pts',(2.52545543365817,0.599012339321944,-2.36915238976667));
#8737=CARTESIAN_POINT('Ctrl Pts',(2.52891199031007,0.604825740975665,-2.36961977464174));
#8738=CARTESIAN_POINT('Ctrl Pts',(2.53429539853988,0.613704796668374,-2.3703326686158));
#8739=CARTESIAN_POINT('Ctrl Pts',(2.53618655810856,0.616791762681776,-2.37058033854345));
#8740=CARTESIAN_POINT('Ctrl Pts',(2.53969411591302,0.62245837562568,-2.37103457256516));
#8741=CARTESIAN_POINT('Ctrl Pts',(2.54130628236905,0.62504047800591,-2.3712413902536));
#8742=CARTESIAN_POINT('Ctrl Pts',(2.54499339671477,0.630895237902823,-2.37170999020497));
#8743=CARTESIAN_POINT('Ctrl Pts',(2.54707449718152,0.634163927470638,-2.37197136873037));
#8744=CARTESIAN_POINT('Ctrl Pts',(2.5525422508336,0.642659040999688,-2.37265021423398));
#8745=CARTESIAN_POINT('Ctrl Pts',(2.55595434474355,0.647869060667929,-2.37306608994603));
#8746=CARTESIAN_POINT('Ctrl Pts',(2.58117657951703,0.685723017493762,-2.37608623415576));
#8747=CARTESIAN_POINT('Ctrl Pts',(2.6045680189091,0.717289075709418,-2.37859711033031));
#8748=CARTESIAN_POINT('Ctrl Pts',(2.70003622473673,0.833493945439406,-2.38805530972885));
#8749=CARTESIAN_POINT('Ctrl Pts',(2.782369527941,0.908938386376902,-2.39472051930603));
#8750=CARTESIAN_POINT('Ctrl Pts',(2.88510326384161,0.979292735583572,-2.40278182644444));
#8751=CARTESIAN_POINT('Ctrl Pts',(2.89627659879153,0.986667831489673,-2.40365465971774));
#8752=CARTESIAN_POINT('Ctrl Pts',(2.91425338258447,0.998098482295169,-2.40505442507073));
#8753=CARTESIAN_POINT('Ctrl Pts',(2.92097640840086,1.00227876899897,-2.40557692470281));
#8754=CARTESIAN_POINT('Ctrl Pts',(2.93383567404664,1.01009582840448,-2.40657478804085));
#8755=CARTESIAN_POINT('Ctrl Pts',(2.93996382704281,1.0137452665026,-2.40704967468512));
#8756=CARTESIAN_POINT('Ctrl Pts',(2.95078359394454,1.02005623146141,-2.40788718810417));
#8757=CARTESIAN_POINT('Ctrl Pts',(2.95546109373587,1.02274163630893,-2.40824894964358));
#8758=CARTESIAN_POINT('Ctrl Pts',(2.96528111377719,1.02829008353822,-2.40900789227968));
#8759=CARTESIAN_POINT('Ctrl Pts',(2.97042696863603,1.03114688772593,-2.4094052816034));
#8760=CARTESIAN_POINT('Ctrl Pts',(2.98374589794393,1.03841103977904,-2.41043316627688));
#8761=CARTESIAN_POINT('Ctrl Pts',(2.99194994108768,1.04276044540044,-2.41106566776457));
#8762=CARTESIAN_POINT('Ctrl Pts',(3.0253289204826,1.05995391520183,-2.41363707451244));
#8763=CARTESIAN_POINT('Ctrl Pts',(3.05090914878522,1.0719859708675,-2.41560347251735));
#8764=CARTESIAN_POINT('Ctrl Pts',(3.18168690422588,1.12784569423022,-2.42564263867971));
#8765=CARTESIAN_POINT('Ctrl Pts',(3.2923946298944,1.15715238259871,-2.43417590664319));
#8766=CARTESIAN_POINT('Ctrl Pts',(3.4317982713568,1.17311044143113,-2.44426477971486));
#8767=CARTESIAN_POINT('Ctrl Pts',(3.45812012148976,1.17523033301461,-2.44613762042885));
#8768=CARTESIAN_POINT('Ctrl Pts',(3.49046756576221,1.1767432965422,-2.44838325310531));
#8769=CARTESIAN_POINT('Ctrl Pts',(3.49644417215425,1.17697722694499,-2.4487958201167));
#8770=CARTESIAN_POINT('Ctrl Pts',(3.50587215824342,1.17727433565949,-2.44944267781701));
#8771=CARTESIAN_POINT('Ctrl Pts',(3.50932237676741,1.17736788491519,-2.44967856286774));
#8772=CARTESIAN_POINT('Ctrl Pts',(3.51584363896025,1.17751601730299,-2.45012276810754));
#8773=CARTESIAN_POINT('Ctrl Pts',(3.51891446205776,1.1775737544982,-2.45033124613507));
#8774=CARTESIAN_POINT('Ctrl Pts',(3.52605185125736,1.17768002245485,-2.45081423666654));
#8775=CARTESIAN_POINT('Ctrl Pts',(3.53011848621199,1.1777195045357,-2.45108825140376));
#8776=CARTESIAN_POINT('Ctrl Pts',(3.54346813430815,1.17777996232603,-2.4519841446979));
#8777=CARTESIAN_POINT('Ctrl Pts',(3.55275147825245,1.17771225304544,-2.45260140044808));
#8778=CARTESIAN_POINT('Ctrl Pts',(3.64428176549376,1.17596220270868,-2.45863916813081));
#8779=CARTESIAN_POINT('Ctrl Pts',(3.72615182411669,1.16577640389569,-2.46366698742564));
#8780=CARTESIAN_POINT('Ctrl Pts',(3.8566515644846,1.13542693010188,-2.47196101923897));
#8781=CARTESIAN_POINT('Ctrl Pts',(3.90617352466559,1.12041565887996,-2.47517572290052));
#8782=CARTESIAN_POINT('Ctrl Pts',(3.97294596164391,1.09527289972979,-2.47973602958418));
#8783=CARTESIAN_POINT('Ctrl Pts',(3.99116843908936,1.08788527730156,-2.48100438058015));
#8784=CARTESIAN_POINT('Ctrl Pts',(4.02278286221714,1.07413716067061,-2.48325347544909));
#8785=CARTESIAN_POINT('Ctrl Pts',(4.03625577210155,1.06797338411652,-2.48422785320584));
#8786=CARTESIAN_POINT('Ctrl Pts',(4.05594479107972,1.05851260625127,-2.48567722236988));
#8787=CARTESIAN_POINT('Ctrl Pts',(4.06225371764276,1.05541126927136,-2.48614555682778));
#8788=CARTESIAN_POINT('Ctrl Pts',(4.07341047867017,1.04980226286008,-2.48698093689607));
#8789=CARTESIAN_POINT('Ctrl Pts',(4.07826939854137,1.04731700499614,-2.48734720081016));
#8790=CARTESIAN_POINT('Ctrl Pts',(4.08846220851999,1.04201384890239,-2.48812078749652));
#8791=CARTESIAN_POINT('Ctrl Pts',(4.09379205849155,1.03918856918159,-2.48852835943091));
#8792=CARTESIAN_POINT('Ctrl Pts',(4.10786329610926,1.03159055333359,-2.48961266336607));
#8793=CARTESIAN_POINT('Ctrl Pts',(4.11656609128106,1.02674775548998,-2.49029183840444));
#8794=CARTESIAN_POINT('Ctrl Pts',(4.15515103655396,1.00463108833202,-2.49334228693625));
#8795=CARTESIAN_POINT('Ctrl Pts',(4.18432395214428,0.986160526803372,-2.49575566049454));
#8796=CARTESIAN_POINT('Ctrl Pts',(4.29478593303441,0.909223897929501,-2.50532712296572));
#8797=CARTESIAN_POINT('Ctrl Pts',(4.36929693350183,0.841772125940284,-2.51279052793263));
#8798=CARTESIAN_POINT('Ctrl Pts',(4.4483440591119,0.749395963933119,-2.52158205437072));
#8799=CARTESIAN_POINT('Ctrl Pts',(4.46187202106959,0.732681593081876,-2.52312248253535));
#8800=CARTESIAN_POINT('Ctrl Pts',(4.48314152308866,0.704878774787815,-2.52559334453062));
#8801=CARTESIAN_POINT('Ctrl Pts',(4.49116278496185,0.694011310819136,-2.52653742320049));
#8802=CARTESIAN_POINT('Ctrl Pts',(4.50175800458639,0.679127340725465,-2.52779885391969));
#8803=CARTESIAN_POINT('Ctrl Pts',(4.50449675698573,0.675230166406004,-2.52812627574458));
#8804=CARTESIAN_POINT('Ctrl Pts',(4.50902690176018,0.668700028797116,-2.52866999942555));
#8805=CARTESIAN_POINT('Ctrl Pts',(4.5108313682993,0.666076260037713,-2.52888715539594));
#8806=CARTESIAN_POINT('Ctrl Pts',(4.51422817391446,0.661094005805544,-2.52929699090346));
#8807=CARTESIAN_POINT('Ctrl Pts',(4.51582263969086,0.658737020327767,-2.52948981583178));
#8808=CARTESIAN_POINT('Ctrl Pts',(4.51957889465443,0.65314081911715,-2.52994519919291));
#8809=CARTESIAN_POINT('Ctrl Pts',(4.52173320828097,0.649896589500528,-2.53020726807833));
#8810=CARTESIAN_POINT('Ctrl Pts',(4.52922797928574,0.638487650169794,-2.53112237803691));
#8811=CARTESIAN_POINT('Ctrl Pts',(4.53448321935766,0.630267055273255,-2.53177014428657));
#8812=CARTESIAN_POINT('Ctrl Pts',(4.57742867063534,0.561212830679454,-2.53712388786931));
#8813=CARTESIAN_POINT('Ctrl Pts',(4.6096096461867,0.497116894239392,-2.54153801287404));
#8814=CARTESIAN_POINT('Ctrl Pts',(4.65718428524163,0.375966075302231,-2.5495888659345));
#8815=CARTESIAN_POINT('Ctrl Pts',(4.67449578182659,0.319926912502816,-2.55320965941292));
#8816=CARTESIAN_POINT('Ctrl Pts',(4.69228824251175,0.242210470480923,-2.55829191314062));
#8817=CARTESIAN_POINT('Ctrl Pts',(4.69645315165062,0.221463603923614,-2.559653780897));
#8818=CARTESIAN_POINT('Ctrl Pts',(4.70272726024923,0.185168818388048,-2.5620532991407));
#8819=CARTESIAN_POINT('Ctrl Pts',(4.70508885038399,0.169669780928801,-2.56308329841438));
#8820=CARTESIAN_POINT('Ctrl Pts',(4.70808112462437,0.147001447260928,-2.56459962712176));
#8821=CARTESIAN_POINT('Ctrl Pts',(4.70895665440399,0.139865768943647,-2.56507836328552));
#8822=CARTESIAN_POINT('Ctrl Pts',(4.71038418714273,0.127278867426568,-2.56592552043681));
#8823=CARTESIAN_POINT('Ctrl Pts',(4.71096358752092,0.121830920761624,-2.56629307990902));
#8824=CARTESIAN_POINT('Ctrl Pts',(4.71209334488938,0.110453805093115,-2.56706260785041));
#8825=CARTESIAN_POINT('Ctrl Pts',(4.71263678741601,0.10452412166865,-2.5674647798512));
#8826=CARTESIAN_POINT('Ctrl Pts',(4.71393906526567,0.0890218998158714,-2.56851919093632));
#8827=CARTESIAN_POINT('Ctrl Pts',(4.71462582199949,0.0794439162948227,-2.56917363755248));
#8828=CARTESIAN_POINT('Ctrl Pts',(4.71704036438852,0.0388088294362735,-2.57196347131861));
#8829=CARTESIAN_POINT('Ctrl Pts',(4.71765442451819,0.00770065833032227,
-2.57413261346457));
#8830=CARTESIAN_POINT('Ctrl Pts',(4.7149742090219,-0.127211525198988,-2.58369058201898));
#8831=CARTESIAN_POINT('Ctrl Pts',(4.6991895760309,-0.230296077338879,-2.5914341498898));
#8832=CARTESIAN_POINT('Ctrl Pts',(4.66401479646512,-0.350823526437734,-2.6005160207918));
#8833=CARTESIAN_POINT('Ctrl Pts',(4.65734612672852,-0.371524659118201,-2.60207455748754));
#8834=CARTESIAN_POINT('Ctrl Pts',(4.64557562306867,-0.40486948655366,-2.60457103662758));
#8835=CARTESIAN_POINT('Ctrl Pts',(4.64082098287936,-0.417629664262643,-2.60552295342225));
#8836=CARTESIAN_POINT('Ctrl Pts',(4.63410025134089,-0.434752670455405,-2.60679307347657));
#8837=CARTESIAN_POINT('Ctrl Pts',(4.63232753935671,-0.439189592727695,-2.60712152010739));
#8838=CARTESIAN_POINT('Ctrl Pts',(4.62932726301842,-0.446568339363818,-2.60766647800685));
#8839=CARTESIAN_POINT('Ctrl Pts',(4.62811468607908,-0.449516145100719,-2.60788385130585));
#8840=CARTESIAN_POINT('Ctrl Pts',(4.6257978724115,-0.455084021856134,-2.60829374278524));
#8841=CARTESIAN_POINT('Ctrl Pts',(4.62469609298194,-0.457705071841693,-2.60848640862326));
#8842=CARTESIAN_POINT('Ctrl Pts',(4.6220665896892,-0.463897592790223,-2.60894097825564));
#8843=CARTESIAN_POINT('Ctrl Pts',(4.62053065523347,-0.467465573806555,-2.60920239673242));
#8844=CARTESIAN_POINT('Ctrl Pts',(4.6150560812966,-0.480011746047182,-2.61012010957465));
#8845=CARTESIAN_POINT('Ctrl Pts',(4.61102288771898,-0.488948589470601,-2.61077106036355));
#8846=CARTESIAN_POINT('Ctrl Pts',(4.57684652289852,-0.56222288362376,-2.6160938940057));
#8847=CARTESIAN_POINT('Ctrl Pts',(4.54104547186122,-0.623771193209739,-2.62047829871699));
#8848=CARTESIAN_POINT('Ctrl Pts',(4.46579723399229,-0.729778559808056,-2.62851950498376));
#8849=CARTESIAN_POINT('Ctrl Pts',(4.42812909766632,-0.775202906246022,-2.63216127658421));
#8850=CARTESIAN_POINT('Ctrl Pts',(4.37248221861363,-0.8328974688399,-2.63727032110493));
#8851=CARTESIAN_POINT('Ctrl Pts',(4.35733320394883,-0.847776953516559,-2.63863676512808));
#8852=CARTESIAN_POINT('Ctrl Pts',(4.33028321266681,-0.872945691321945,-2.64104361591959));
#8853=CARTESIAN_POINT('Ctrl Pts',(4.31856270978703,-0.88342123544306,-2.64207630525539));
#8854=CARTESIAN_POINT('Ctrl Pts',(4.30117573251054,-0.898346232910581,-2.64359586499526));
#8855=CARTESIAN_POINT('Ctrl Pts',(4.29567221033426,-0.902983527239545,-2.64407509531094));
#8856=CARTESIAN_POINT('Ctrl Pts',(4.2859039545646,-0.911062382650963,-2.64492281687599));
#8857=CARTESIAN_POINT('Ctrl Pts',(4.28165701469321,-0.914525194005671,-2.64529044280048));
#8858=CARTESIAN_POINT('Ctrl Pts',(4.27274771403405,-0.921686609048955,-2.64605980217086));
#8859=CARTESIAN_POINT('Ctrl Pts',(4.26808118581423,-0.925379755059735,-2.64646173709269));
#8860=CARTESIAN_POINT('Ctrl Pts',(4.25582465277012,-0.934929544448758,-2.64751483515616));
#8861=CARTESIAN_POINT('Ctrl Pts',(4.24819090344159,-0.940729060013479,-2.64816819569537));
#8862=CARTESIAN_POINT('Ctrl Pts',(4.21561129091714,-0.964858859684301,-2.65094665999334));
#8863=CARTESIAN_POINT('Ctrl Pts',(4.1900206592744,-0.982293585291936,-2.65310517502672));
#8864=CARTESIAN_POINT('Ctrl Pts',(4.13591074816408,-1.01611602628934,-2.65762425458699));
#8865=CARTESIAN_POINT('Ctrl Pts',(4.10734937419749,-1.03234708339974,-2.65998568832657));
#8866=CARTESIAN_POINT('Ctrl Pts',(4.07816899834492,-1.04735442716575,-2.6623694009368));
#8867=CARTESIAN_POINT('Origin',(3.53951905042299,8.32667268468867E-16,0.924367114736157));
#8868=CARTESIAN_POINT('',(4.07816931781854,-1.04735426286176,-3.26243320031815));
#8869=CARTESIAN_POINT('',(4.07816926753082,-1.04735428872454,-3.16389876579091));
#8870=CARTESIAN_POINT('',(4.07816926754759,-1.04735428871592,0.924367114736157));
#8871=CARTESIAN_POINT('',(2.36176898865594,-0.000625254868193132,-2.92357953805437));
#8872=CARTESIAN_POINT('Ctrl Pts',(4.07816931781854,-1.04735426286176,-3.26243320031815));
#8873=CARTESIAN_POINT('Ctrl Pts',(4.09898123165306,-1.03665077565644,-3.26077374776886));
#8874=CARTESIAN_POINT('Ctrl Pts',(4.11947420255453,-1.02532691942579,-3.25909590190709));
#8875=CARTESIAN_POINT('Ctrl Pts',(4.18089036335886,-0.988958206562127,-3.25393705625322));
#8876=CARTESIAN_POINT('Ctrl Pts',(4.22062680818187,-0.962022496624445,-3.25041459606803));
#8877=CARTESIAN_POINT('Ctrl Pts',(4.28095180582499,-0.91551542035171,-3.24482602715964));
#8878=CARTESIAN_POINT('Ctrl Pts',(4.30266984491695,-0.897492047178338,-3.2427597435237));
#8879=CARTESIAN_POINT('Ctrl Pts',(4.34956955752838,-0.855636381517705,-3.23820211300989));
#8880=CARTESIAN_POINT('Ctrl Pts',(4.37439114140176,-0.831435222165497,-3.23572322234103));
#8881=CARTESIAN_POINT('Ctrl Pts',(4.40226168444952,-0.801752435915756,-3.23289319515093));
#8882=CARTESIAN_POINT('Ctrl Pts',(4.40637765999414,-0.797300430167136,-3.2324739926128));
#8883=CARTESIAN_POINT('Ctrl Pts',(4.41303447604109,-0.789987657795277,-3.23179422630176));
#8884=CARTESIAN_POINT('Ctrl Pts',(4.4155960194558,-0.787146011634137,-3.23153221282202));
#8885=CARTESIAN_POINT('Ctrl Pts',(4.42016942300341,-0.782022529874782,-3.23106369850168));
#8886=CARTESIAN_POINT('Ctrl Pts',(4.42218632461181,-0.77974534283531,-3.23085683392516));
#8887=CARTESIAN_POINT('Ctrl Pts',(4.4266115195677,-0.774709894419688,-3.23040241652877));
#8888=CARTESIAN_POINT('Ctrl Pts',(4.42901578492135,-0.771948203931422,-3.2301551553211));
#8889=CARTESIAN_POINT('Ctrl Pts',(4.43595169874441,-0.763905747078712,-3.2294406123789));
#8890=CARTESIAN_POINT('Ctrl Pts',(4.44044957034633,-0.7585958656908,-3.22897569269589));
#8891=CARTESIAN_POINT('Ctrl Pts',(4.47828760051015,-0.713115599425455,-3.22504820078121));
#8892=CARTESIAN_POINT('Ctrl Pts',(4.50897454489097,-0.670803815023034,-3.22175216591452));
#8893=CARTESIAN_POINT('Ctrl Pts',(4.58101811686311,-0.556144329431365,-3.21331711446517));
#8894=CARTESIAN_POINT('Ctrl Pts',(4.61769001547176,-0.48121076433104,-3.20825435836269));
#8895=CARTESIAN_POINT('Ctrl Pts',(4.65670197413009,-0.374094002510949,-3.20098314537484));
#8896=CARTESIAN_POINT('Ctrl Pts',(4.66610330262087,-0.344748712049452,-3.19899026191916));
#8897=CARTESIAN_POINT('Ctrl Pts',(4.67690373392857,-0.305847614166114,-3.19632957539751));
#8898=CARTESIAN_POINT('Ctrl Pts',(4.67935177201027,-0.296594064800206,-3.19569533491674));
#8899=CARTESIAN_POINT('Ctrl Pts',(4.68313781807165,-0.28154317784173,-3.19466111171145));
#8900=CARTESIAN_POINT('Ctrl Pts',(4.68454519643704,-0.275763611550849,-3.19426334430423));
#8901=CARTESIAN_POINT('Ctrl Pts',(4.68716528611193,-0.264637922322687,-3.19349632801746));
#8902=CARTESIAN_POINT('Ctrl Pts',(4.68838457508171,-0.259293495348176,-3.19312729888676));
#8903=CARTESIAN_POINT('Ctrl Pts',(4.69112020017064,-0.246904394060618,-3.19227040691711));
#8904=CARTESIAN_POINT('Ctrl Pts',(4.69260926728713,-0.239853988261029,-3.19178169703675));
#8905=CARTESIAN_POINT('Ctrl Pts',(4.69714974273213,-0.217335695288724,-3.19021715824792));
#8906=CARTESIAN_POINT('Ctrl Pts',(4.69995519319665,-0.201820566466135,-3.18913369440768));
#8907=CARTESIAN_POINT('Ctrl Pts',(4.70581889874727,-0.165208956842626,-3.18656290822938));
#8908=CARTESIAN_POINT('Ctrl Pts',(4.70861743537951,-0.144077077533306,-3.18506810293955));
#8909=CARTESIAN_POINT('Ctrl Pts',(4.717031610013,-0.0638724316287148,-3.17935291486217));
#8910=CARTESIAN_POINT('Ctrl Pts',(4.7187535358822,-0.00448560868510401,
-3.17503018604703));
#8911=CARTESIAN_POINT('Ctrl Pts',(4.71271772414196,0.125161570364879,-3.16550907888864));
#8912=CARTESIAN_POINT('Ctrl Pts',(4.70312976001682,0.195121626808908,-3.16031579482553));
#8913=CARTESIAN_POINT('Ctrl Pts',(4.68514159142383,0.27338733275801,-3.15468723984344));
#8914=CARTESIAN_POINT('Ctrl Pts',(4.6828204263157,0.28293748383211,-3.15400375945776));
#8915=CARTESIAN_POINT('Ctrl Pts',(4.67941435630051,0.296224362767218,-3.15305853801882));
#8916=CARTESIAN_POINT('Ctrl Pts',(4.67843015055881,0.299986147212322,-3.15279156679651));
#8917=CARTESIAN_POINT('Ctrl Pts',(4.67669373836408,0.306491243403072,-3.15233109522539));
#8918=CARTESIAN_POINT('Ctrl Pts',(4.67595019803625,0.309236803032795,-3.15213711568797));
#8919=CARTESIAN_POINT('Ctrl Pts',(4.67435251456974,0.315052737656819,-3.15172702876877));
#8920=CARTESIAN_POINT('Ctrl Pts',(4.67349584063548,0.318122395669769,-3.1515110724618));
#8921=CARTESIAN_POINT('Ctrl Pts',(4.67132482986644,0.325781413123964,-3.15097337925169));
#8922=CARTESIAN_POINT('Ctrl Pts',(4.66999501323815,0.330366388979926,-3.15065251490368));
#8923=CARTESIAN_POINT('Ctrl Pts',(4.66477473877105,0.347964317304035,-3.14942445343302));
#8924=CARTESIAN_POINT('Ctrl Pts',(4.66068699494352,0.360918286318838,-3.14852778654404));
#8925=CARTESIAN_POINT('Ctrl Pts',(4.64949903311173,0.394346254053465,-3.1462259827269));
#8926=CARTESIAN_POINT('Ctrl Pts',(4.64205607681412,0.414700796148441,-3.14483626430258));
#8927=CARTESIAN_POINT('Ctrl Pts',(4.59616468852104,0.530214176758995,-3.13695652331111));
#8928=CARTESIAN_POINT('Ctrl Pts',(4.54597120322335,0.620228405255614,-3.13080422978946));
#8929=CARTESIAN_POINT('Ctrl Pts',(4.46554235428616,0.728431022590795,-3.12221841882979));
#8930=CARTESIAN_POINT('Ctrl Pts',(4.44529301680332,0.753461443599445,-3.12013877275636));
#8931=CARTESIAN_POINT('Ctrl Pts',(4.41762695646553,0.784930613853651,-3.11737826916035));
#8932=CARTESIAN_POINT('Ctrl Pts',(4.4111184186301,0.792151560787731,-3.11673429720841));
#8933=CARTESIAN_POINT('Ctrl Pts',(4.40046232468838,0.803683714867934,-3.11568812872689));
#8934=CARTESIAN_POINT('Ctrl Pts',(4.39636991474247,0.808045437540622,-3.11528824500119));
#8935=CARTESIAN_POINT('Ctrl Pts',(4.3884701358773,0.816337589057383,-3.11451980373157));
#8936=CARTESIAN_POINT('Ctrl Pts',(4.38466823967373,0.820273034408421,-3.11415148542705));
#8937=CARTESIAN_POINT('Ctrl Pts',(4.37584579462664,0.829278935926336,-3.1133001398748));
#8938=CARTESIAN_POINT('Ctrl Pts',(4.37080635692301,0.834330502148808,-3.11281630092054));
#8939=CARTESIAN_POINT('Ctrl Pts',(4.35476144899995,0.850124347571058,-3.11128325649028));
#8940=CARTESIAN_POINT('Ctrl Pts',(4.34359168879005,0.860696652868589,-3.11022684326068));
#8941=CARTESIAN_POINT('Ctrl Pts',(4.31695691172093,0.884935734864475,-3.10773149347546));
#8942=CARTESIAN_POINT('Ctrl Pts',(4.30133372362759,0.898420390301959,-3.10628565668475));
#8943=CARTESIAN_POINT('Ctrl Pts',(4.24195762342701,0.947006308644113,-3.10085503001304));
#8944=CARTESIAN_POINT('Ctrl Pts',(4.19607283038112,0.979375707133186,-3.09677880310597));
#8945=CARTESIAN_POINT('Ctrl Pts',(4.08355915014974,1.04727809421341,-3.0871456659951));
#8946=CARTESIAN_POINT('Ctrl Pts',(4.01546488997766,1.07992985167665,-3.08157798058244));
#8947=CARTESIAN_POINT('Ctrl Pts',(3.93575110257492,1.10913764914287,-3.07563112378125));
#8948=CARTESIAN_POINT('Ctrl Pts',(3.92674910943286,1.11231248295765,-3.07496757098236));
#8949=CARTESIAN_POINT('Ctrl Pts',(3.9140550111687,1.11661665964354,-3.07404402858618));
#8950=CARTESIAN_POINT('Ctrl Pts',(3.91039472619574,1.11783772733574,-3.07377913886759));
#8951=CARTESIAN_POINT('Ctrl Pts',(3.90376503254966,1.12001323850551,-3.0733019843398));
#8952=CARTESIAN_POINT('Ctrl Pts',(3.90079771314711,1.12097391521363,-3.07308936738531));
#8953=CARTESIAN_POINT('Ctrl Pts',(3.89471579394369,1.12291629237651,-3.07265556628039));
#8954=CARTESIAN_POINT('Ctrl Pts',(3.89160087318409,1.12389684448009,-3.07243444833196));
#8955=CARTESIAN_POINT('Ctrl Pts',(3.88357512311059,1.1263866452399,-3.07186734855767));
#8956=CARTESIAN_POINT('Ctrl Pts',(3.87865836036316,1.12787676037447,-3.07152244821973));
#8957=CARTESIAN_POINT('Ctrl Pts',(3.85784106680156,1.13403738478238,-3.07007215887183));
#8958=CARTESIAN_POINT('Ctrl Pts',(3.84185175910993,1.13840445255659,-3.06898279057254));
#8959=CARTESIAN_POINT('Ctrl Pts',(3.79779539720328,1.14944350812838,-3.06603464785777));
#8960=CARTESIAN_POINT('Ctrl Pts',(3.76956603617532,1.15542445294395,-3.06420426936595));
#8961=CARTESIAN_POINT('Ctrl Pts',(3.65236277013015,1.17578968781411,-3.05674162313343));
#8962=CARTESIAN_POINT('Ctrl Pts',(3.56210673468793,1.18097644135648,-3.05129224510835));
#8963=CARTESIAN_POINT('Ctrl Pts',(3.43874818711212,1.17390757964574,-3.04343456534833));
#8964=CARTESIAN_POINT('Ctrl Pts',(3.40545524523167,1.17057265804319,-3.04127573186305));
#8965=CARTESIAN_POINT('Ctrl Pts',(3.36258897377222,1.16442607196494,-3.03842366942584));
#8966=CARTESIAN_POINT('Ctrl Pts',(3.35284466320023,1.16290369014257,-3.03777049843266));
#8967=CARTESIAN_POINT('Ctrl Pts',(3.33719321170105,1.16025663519616,-3.03671303332578));
#8968=CARTESIAN_POINT('Ctrl Pts',(3.33127342281148,1.15920876499731,-3.03631114569044));
#8969=CARTESIAN_POINT('Ctrl Pts',(3.31998938642432,1.15712213755397,-3.03554128387523));
#8970=CARTESIAN_POINT('Ctrl Pts',(3.3146238230945,1.15609128082198,-3.0351735670076));
#8971=CARTESIAN_POINT('Ctrl Pts',(3.30232945122369,1.15364040328501,-3.03432712145705));
#8972=CARTESIAN_POINT('Ctrl Pts',(3.29540592976194,1.15219523805879,-3.03384761236167));
#8973=CARTESIAN_POINT('Ctrl Pts',(3.27380142659997,1.14748220578995,-3.0323422102748));
#8974=CARTESIAN_POINT('Ctrl Pts',(3.25917025366127,1.14399553500785,-3.03130947404064));
#8975=CARTESIAN_POINT('Ctrl Pts',(3.22520160006125,1.13520989456155,-3.0288797077516));
#8976=CARTESIAN_POINT('Ctrl Pts',(3.20592516664892,1.12969553558251,-3.02747626244873));
#8977=CARTESIAN_POINT('Ctrl Pts',(3.13584961030794,1.1076993002196,-3.02228289252604));
#8978=CARTESIAN_POINT('Ctrl Pts',(3.08605149873003,1.08826137209012,-3.01841009580805));
#8979=CARTESIAN_POINT('Ctrl Pts',(2.96575488118993,1.03161149525829,-3.00867214789956));
#8980=CARTESIAN_POINT('Ctrl Pts',(2.89737749811574,0.990496727423987,-3.00277772670497));
#8981=CARTESIAN_POINT('Ctrl Pts',(2.82609590149246,0.937129602496751,-2.99654461758004));
#8982=CARTESIAN_POINT('Ctrl Pts',(2.81859441315035,0.931371119807035,-2.99588768084404));
#8983=CARTESIAN_POINT('Ctrl Pts',(2.80823067980064,0.923215198836997,-2.99497962198354));
#8984=CARTESIAN_POINT('Ctrl Pts',(2.80530948450529,0.920893749918574,-2.9947236181095));
#8985=CARTESIAN_POINT('Ctrl Pts',(2.7999920613324,0.916626653290633,-2.99425759677987));
#8986=CARTESIAN_POINT('Ctrl Pts',(2.79759235621169,0.914685394228212,-2.99404727900163));
#8987=CARTESIAN_POINT('Ctrl Pts',(2.79267853624424,0.910678261920784,-2.99361664491302));
#8988=CARTESIAN_POINT('Ctrl Pts',(2.79016531906168,0.908611378037216,-2.99339640243066));
#8989=CARTESIAN_POINT('Ctrl Pts',(2.78382471910707,0.903352631117224,-2.99284068094873));
#8990=CARTESIAN_POINT('Ctrl Pts',(2.78000892335124,0.900146803362335,-2.99250617943619));
#8991=CARTESIAN_POINT('Ctrl Pts',(2.77156590826644,0.892961521124877,-2.99176559787924));
#8992=CARTESIAN_POINT('Ctrl Pts',(2.76694900595163,0.888970098961088,-2.99136032179021));
#8993=CARTESIAN_POINT('Ctrl Pts',(2.75336838547996,0.877043613453188,-2.99016656850655));
#8994=CARTESIAN_POINT('Ctrl Pts',(2.74449412509974,0.869007341765758,-2.98938437205073));
#8995=CARTESIAN_POINT('Ctrl Pts',(2.71221159401029,0.838864687616953,-2.98652411146555));
#8996=CARTESIAN_POINT('Ctrl Pts',(2.68958869158389,0.815935216623709,-2.98449006959003));
#8997=CARTESIAN_POINT('Ctrl Pts',(2.64741628714215,0.76953118962899,-2.98057109969574));
#8998=CARTESIAN_POINT('Ctrl Pts',(2.62778452086387,0.74616742064803,-2.97868545287518));
#8999=CARTESIAN_POINT('Ctrl Pts',(2.56081044010637,0.659866347285038,-2.971928474251));
#9000=CARTESIAN_POINT('Ctrl Pts',(2.51890383847443,0.592989679325828,-2.96705225778148));
#9001=CARTESIAN_POINT('Ctrl Pts',(2.47711476945722,0.508558740284475,-2.96091314815011));
#9002=CARTESIAN_POINT('Ctrl Pts',(2.47052042962176,0.494547026085853,-2.959895532211));
#9003=CARTESIAN_POINT('Ctrl Pts',(2.46131737641683,0.473947580961091,-2.95839914599736));
#9004=CARTESIAN_POINT('Ctrl Pts',(2.45848862975219,0.467459501193249,-2.95792779670517));
#9005=CARTESIAN_POINT('Ctrl Pts',(2.4535735037439,0.45590280947347,-2.95708795222146));
#9006=CARTESIAN_POINT('Ctrl Pts',(2.4514636859194,0.45084434573589,-2.95672025509591));
#9007=CARTESIAN_POINT('Ctrl Pts',(2.44713671866986,0.440262788288645,-2.95595080791469));
#9008=CARTESIAN_POINT('Ctrl Pts',(2.44492597767211,0.434737258954002,-2.95554885673257));
#9009=CARTESIAN_POINT('Ctrl Pts',(2.43926421024867,0.420269229374129,-2.95449585176128));
#9010=CARTESIAN_POINT('Ctrl Pts',(2.43588036676449,0.411301088013082,-2.95384260188764));
#9011=CARTESIAN_POINT('Ctrl Pts',(2.42088304839541,0.370035825769206,-2.9508336237206));
#9012=CARTESIAN_POINT('Ctrl Pts',(2.41057640581616,0.337284906602885,-2.94843596440213));
#9013=CARTESIAN_POINT('Ctrl Pts',(2.37514083636209,0.204715705984923,-2.93868725117212));
#9014=CARTESIAN_POINT('Ctrl Pts',(2.3617147452602,0.102251104413654,-2.93100628751565));
#9015=CARTESIAN_POINT('Ctrl Pts',(2.36176921551447,-0.000623596785416757,
-2.92357926301356));
#9016=CARTESIAN_POINT('Ctrl Pts',(2.36176921637844,-0.000625226391580778,
-2.9235791453644));
#9017=CARTESIAN_POINT('Ctrl Pts',(2.36177995253325,-0.0208491080398596,
-2.92211908578818));
#9018=CARTESIAN_POINT('Ctrl Pts',(2.36231160441552,-0.0410707918882081,
-2.92067213902583));
#9019=CARTESIAN_POINT('Ctrl Pts',(2.36393814619697,-0.0722942803543454,
-2.91846711246166));
#9020=CARTESIAN_POINT('Ctrl Pts',(2.36466742904508,-0.0833103485689905,
-2.91769478376438));
#9021=CARTESIAN_POINT('Ctrl Pts',(2.36588675799784,-0.0984877076839081,
-2.91663990991943));
#9022=CARTESIAN_POINT('Ctrl Pts',(2.36624423883107,-0.102658677967047,-2.91635097498123));
#9023=CARTESIAN_POINT('Ctrl Pts',(2.36690394968759,-0.109901850026181,-2.91585098981703));
#9024=CARTESIAN_POINT('Ctrl Pts',(2.36719603042186,-0.112974901773122,-2.91563941588688));
#9025=CARTESIAN_POINT('Ctrl Pts',(2.36778565625838,-0.118929848571435,-2.91523054885575));
#9026=CARTESIAN_POINT('Ctrl Pts',(2.36808176065682,-0.121811874484103,-2.91503317878497));
#9027=CARTESIAN_POINT('Ctrl Pts',(2.36874028834502,-0.127996847255564,-2.91461074374743));
#9028=CARTESIAN_POINT('Ctrl Pts',(2.36910605785658,-0.131299391329682,-2.91438586583273));
#9029=CARTESIAN_POINT('Ctrl Pts',(2.37010253801986,-0.139961438132476,-2.91379774505669));
#9030=CARTESIAN_POINT('Ctrl Pts',(2.37075612493424,-0.145318307266515,-2.91343574125296));
#9031=CARTESIAN_POINT('Ctrl Pts',(2.37364228282265,-0.167693218127024,-2.9119301331203));
#9032=CARTESIAN_POINT('Ctrl Pts',(2.37621003124648,-0.184666870926862,-2.91080354726058));
#9033=CARTESIAN_POINT('Ctrl Pts',(2.38355629806838,-0.226954902118574,-2.90802219860602));
#9034=CARTESIAN_POINT('Ctrl Pts',(2.38879601553485,-0.25218064174336,-2.90638596880244));
#9035=CARTESIAN_POINT('Ctrl Pts',(2.40573826379939,-0.322137397521182,-2.90186293844977));
#9036=CARTESIAN_POINT('Ctrl Pts',(2.41925278262559,-0.3663811617874,-2.89901814094692));
#9037=CARTESIAN_POINT('Ctrl Pts',(2.46094290425218,-0.478735797902303,-2.89159887795137));
#9038=CARTESIAN_POINT('Ctrl Pts',(2.49296361809847,-0.545191890575193,-2.88700593960339));
#9039=CARTESIAN_POINT('Ctrl Pts',(2.53773130295301,-0.61942519771123,-2.88133325212123));
#9040=CARTESIAN_POINT('Ctrl Pts',(2.54467449665439,-0.630516104614747,-2.88047081024581));
#9041=CARTESIAN_POINT('Ctrl Pts',(2.55544671078219,-0.647102386879967,-2.87915704588438));
#9042=CARTESIAN_POINT('Ctrl Pts',(2.55914034169745,-0.652684803809364,-2.87871067758816));
#9043=CARTESIAN_POINT('Ctrl Pts',(2.56591382321415,-0.662734762261757,-2.87789928167066));
#9044=CARTESIAN_POINT('Ctrl Pts',(2.56897736423906,-0.667213112322162,-2.87753486806232));
#9045=CARTESIAN_POINT('Ctrl Pts',(2.57563359381759,-0.676800485599777,-2.87674847577718));
#9046=CARTESIAN_POINT('Ctrl Pts',(2.57923618273684,-0.68190239931979,-2.87632613176537));
#9047=CARTESIAN_POINT('Ctrl Pts',(2.58909409001416,-0.695629919435375,-2.87517908045506));
#9048=CARTESIAN_POINT('Ctrl Pts',(2.59542603320923,-0.704199511570753,-2.87445147492619));
#9049=CARTESIAN_POINT('Ctrl Pts',(2.62928880728463,-0.748751358861594,-2.87060648219384));
#9050=CARTESIAN_POINT('Ctrl Pts',(2.65875935563354,-0.783204399808276,-2.86741420673774));
#9051=CARTESIAN_POINT('Ctrl Pts',(2.76508018517716,-0.893892150996087,-2.85638692434851));
#9052=CARTESIAN_POINT('Ctrl Pts',(2.85040651993699,-0.961207661226993,-2.8482589597979));
#9053=CARTESIAN_POINT('Ctrl Pts',(2.95210904712649,-1.02085220409374,-2.83992351738191));
#9054=CARTESIAN_POINT('Ctrl Pts',(2.96056311954913,-1.02567040445183,-2.83924029034334));
#9055=CARTESIAN_POINT('Ctrl Pts',(2.97369773304519,-1.03294201375371,-2.83819467877136));
#9056=CARTESIAN_POINT('Ctrl Pts',(2.97833649597358,-1.03546951189299,-2.8378284118626));
#9057=CARTESIAN_POINT('Ctrl Pts',(2.98698223012976,-1.04010510128481,-2.83715155103884));
#9058=CARTESIAN_POINT('Ctrl Pts',(2.99098463496274,-1.04222145259095,-2.83684049007336));
#9059=CARTESIAN_POINT('Ctrl Pts',(2.99775568870063,-1.045751971641,-2.83631821348526));
#9060=CARTESIAN_POINT('Ctrl Pts',(3.00051788250106,-1.04717833629616,-2.8361062587771));
#9061=CARTESIAN_POINT('Ctrl Pts',(3.00582895168737,-1.04989432818294,-2.83570087696403));
#9062=CARTESIAN_POINT('Ctrl Pts',(3.00837691587402,-1.05118564259061,-2.83550734240186));
#9063=CARTESIAN_POINT('Ctrl Pts',(3.0144471776645,-1.05423435985338,-2.8350484510906));
#9064=CARTESIAN_POINT('Ctrl Pts',(3.01797366531702,-1.05598341342791,-2.83478360193138));
#9065=CARTESIAN_POINT('Ctrl Pts',(3.03049394491246,-1.06211515308135,-2.83384921154611));
#9066=CARTESIAN_POINT('Ctrl Pts',(3.03953504296172,-1.06640103384721,-2.8331852396339));
#9067=CARTESIAN_POINT('Ctrl Pts',(3.10446791240979,-1.09617469918957,-2.82848527632254));
#9068=CARTESIAN_POINT('Ctrl Pts',(3.16223100034578,-1.11737377807566,-2.82466175740634));
#9069=CARTESIAN_POINT('Ctrl Pts',(3.28255192659474,-1.15112901954021,-2.81692226045837));
#9070=CARTESIAN_POINT('Ctrl Pts',(3.34499733525782,-1.16331031487389,-2.81301786135179));
#9071=CARTESIAN_POINT('Ctrl Pts',(3.43177991591932,-1.17305338855851,-2.80747544948084));
#9072=CARTESIAN_POINT('Ctrl Pts',(3.45551501799545,-1.17499156879255,-2.80594867875171));
#9073=CARTESIAN_POINT('Ctrl Pts',(3.49642316028897,-1.17708626329455,-2.80328652079047));
#9074=CARTESIAN_POINT('Ctrl Pts',(3.51357121823404,-1.17758905744754,-2.80216136987946));
#9075=CARTESIAN_POINT('Ctrl Pts',(3.53817314099144,-1.17777279299101,-2.80053111148832));
#9076=CARTESIAN_POINT('Ctrl Pts',(3.54562303807762,-1.17775774268812,-2.80003533961058));
#9077=CARTESIAN_POINT('Ctrl Pts',(3.55859111690027,-1.17760850107451,-2.79916846485678));
#9078=CARTESIAN_POINT('Ctrl Pts',(3.56410948687455,-1.17750619284652,-2.79879835572167));
#9079=CARTESIAN_POINT('Ctrl Pts',(3.57547557982453,-1.17721553695408,-2.79803343347121));
#9080=CARTESIAN_POINT('Ctrl Pts',(3.581323016198,-1.17702239518642,-2.79763848250897));
#9081=CARTESIAN_POINT('Ctrl Pts',(3.59628177395603,-1.17641669502769,-2.79662435825079));
#9082=CARTESIAN_POINT('Ctrl Pts',(3.60539004330609,-1.17594185711139,-2.79600328115178));
#9083=CARTESIAN_POINT('Ctrl Pts',(3.64131579082277,-1.17365026633381,-2.79353885603012));
#9084=CARTESIAN_POINT('Ctrl Pts',(3.66807143424096,-1.17102160798452,-2.79167083174068));
#9085=CARTESIAN_POINT('Ctrl Pts',(3.71514288197416,-1.16476440979611,-2.78832427819953));
#9086=CARTESIAN_POINT('Ctrl Pts',(3.73549795867999,-1.1615128274658,-2.78685710071484));
#9087=CARTESIAN_POINT('Ctrl Pts',(3.83437104187927,-1.14304559977494,-2.77963608550316));
#9088=CARTESIAN_POINT('Ctrl Pts',(3.9112827884676,-1.12039316030081,-2.77370749788644));
#9089=CARTESIAN_POINT('Ctrl Pts',(4.01685826394394,-1.07722098807654,-2.76540715412209));
#9090=CARTESIAN_POINT('Ctrl Pts',(4.04784516790297,-1.06294985473338,-2.76295256712908));
#9091=CARTESIAN_POINT('Ctrl Pts',(4.07816927004253,-1.04735428743277,-2.76055935511047));
#9092=CARTESIAN_POINT('Ctrl Pts',(4.07816899834492,-1.04735442716575,-2.6623694009368));
#9093=CARTESIAN_POINT('Ctrl Pts',(4.0335762669856,-1.07028828012076,-2.66601213181191));
#9094=CARTESIAN_POINT('Ctrl Pts',(3.98753809253346,-1.0903643388365,-2.66970861591428));
#9095=CARTESIAN_POINT('Ctrl Pts',(3.89128984941738,-1.12519885517188,-2.67720140153078));
#9096=CARTESIAN_POINT('Ctrl Pts',(3.84111741288379,-1.13967314890724,-2.68098522172963));
#9097=CARTESIAN_POINT('Ctrl Pts',(3.78334776792184,-1.152254753361,-2.68509742216502));
#9098=CARTESIAN_POINT('Ctrl Pts',(3.77653707951909,-1.15367496282613,-2.68557840510683));
#9099=CARTESIAN_POINT('Ctrl Pts',(3.76612376885243,-1.15575030428102,-2.686307588158));
#9100=CARTESIAN_POINT('Ctrl Pts',(3.76253015568023,-1.15644909620269,-2.68655810071));
#9101=CARTESIAN_POINT('Ctrl Pts',(3.75594503727697,-1.15769776081088,-2.68701501927083));
#9102=CARTESIAN_POINT('Ctrl Pts',(3.75295464911626,-1.15825280436929,-2.68722170114632));
#9103=CARTESIAN_POINT('Ctrl Pts',(3.74619844681159,-1.15947976322849,-2.68768684842611));
#9104=CARTESIAN_POINT('Ctrl Pts',(3.74243148748152,-1.16014492118331,-2.68794493579724));
#9105=CARTESIAN_POINT('Ctrl Pts',(3.73268641675675,-1.16181675872849,-2.68860951174878));
#9106=CARTESIAN_POINT('Ctrl Pts',(3.72670356511524,-1.16279567145485,-2.68901451683044));
#9107=CARTESIAN_POINT('Ctrl Pts',(3.6864822382747,-1.16905819113362,-2.6917187615668));
#9108=CARTESIAN_POINT('Ctrl Pts',(3.65202899538887,-1.17287563292434,-2.69394545358489));
#9109=CARTESIAN_POINT('Ctrl Pts',(3.58929340211189,-1.17703614795284,-2.69791828714987));
#9110=CARTESIAN_POINT('Ctrl Pts',(3.56107348878191,-1.17789095713726,-2.69967561287454));
#9111=CARTESIAN_POINT('Ctrl Pts',(3.48487642248419,-1.17745942740425,-2.70440004502096));
#9112=CARTESIAN_POINT('Ctrl Pts',(3.43696596257267,-1.17425691029762,-2.70735019626798));
#9113=CARTESIAN_POINT('Ctrl Pts',(3.33649323509623,-1.16134375120642,-2.71368497026683));
#9114=CARTESIAN_POINT('Ctrl Pts',(3.28413075753254,-1.15096243469239,-2.7170749199365));
#9115=CARTESIAN_POINT('Ctrl Pts',(3.22219955533574,-1.13424895742127,-2.72129091886645));
#9116=CARTESIAN_POINT('Ctrl Pts',(3.21178298297185,-1.13128308424335,-2.72200707908536));
#9117=CARTESIAN_POINT('Ctrl Pts',(3.19544928162242,-1.12638792875238,-2.72314188347338));
#9118=CARTESIAN_POINT('Ctrl Pts',(3.189503838138,-1.12455463206792,-2.72355743895784));
#9119=CARTESIAN_POINT('Ctrl Pts',(3.17839984088432,-1.1210340913855,-2.72433835221193));
#9120=CARTESIAN_POINT('Ctrl Pts',(3.17323786273431,-1.1193581229451,-2.72470333613297));
#9121=CARTESIAN_POINT('Ctrl Pts',(3.16170697771525,-1.11552602427491,-2.7255231221525));
#9122=CARTESIAN_POINT('Ctrl Pts',(3.1553446233849,-1.11335092378222,-2.72597853192961));
#9123=CARTESIAN_POINT('Ctrl Pts',(3.13920211123965,-1.1076774338607,-2.72714201907597));
#9124=CARTESIAN_POINT('Ctrl Pts',(3.12944913969143,-1.10410398315409,-2.72785252619133));
#9125=CARTESIAN_POINT('Ctrl Pts',(3.04922531641467,-1.07350073234107,-2.73376105817357));
#9126=CARTESIAN_POINT('Ctrl Pts',(2.98146806609331,-1.03988796688262,-2.73918081187918));
#9127=CARTESIAN_POINT('Ctrl Pts',(2.86829878120403,-0.969485798722418,-2.74893061046611));
#9128=CARTESIAN_POINT('Ctrl Pts',(2.8215111047524,-0.935363141093665,-2.75320181318344));
#9129=CARTESIAN_POINT('Ctrl Pts',(2.76180456356438,-0.884689017107384,-2.75885673514513));
#9130=CARTESIAN_POINT('Ctrl Pts',(2.74653778073392,-0.871031162163133,-2.7603222094531));
#9131=CARTESIAN_POINT('Ctrl Pts',(2.72214329356571,-0.848034233290433,-2.76268655246011));
#9132=CARTESIAN_POINT('Ctrl Pts',(2.71280125319164,-0.838929620280964,-2.76359773775796));
#9133=CARTESIAN_POINT('Ctrl Pts',(2.70030074536453,-0.826335157333877,-2.76482260626028));
#9134=CARTESIAN_POINT('Ctrl Pts',(2.69700949265504,-0.822979223762437,-2.76514564572327));
#9135=CARTESIAN_POINT('Ctrl Pts',(2.6915314441139,-0.817326213328243,-2.76568410084221));
#9136=CARTESIAN_POINT('Ctrl Pts',(2.68933370360339,-0.815039874042446,-2.76590033690781));
#9137=CARTESIAN_POINT('Ctrl Pts',(2.68517389987865,-0.810677239313141,-2.76630997969622));
#9138=CARTESIAN_POINT('Ctrl Pts',(2.68321011946522,-0.808602645187202,-2.76650352192994));
#9139=CARTESIAN_POINT('Ctrl Pts',(2.67855715943709,-0.803651163410908,-2.76696253162854));
#9140=CARTESIAN_POINT('Ctrl Pts',(2.67587480087992,-0.800767869932894,-2.76722749067123));
#9141=CARTESIAN_POINT('Ctrl Pts',(2.66642093822593,-0.790503059292525,-2.768162799715));
#9142=CARTESIAN_POINT('Ctrl Pts',(2.65972896781401,-0.783048419406329,-2.76882756556243));
#9143=CARTESIAN_POINT('Ctrl Pts',(2.61337929261124,-0.730071959822742,-2.77345875290756));
#9144=CARTESIAN_POINT('Ctrl Pts',(2.57717310846499,-0.681639268235826,-2.77722018773758));
#9145=CARTESIAN_POINT('Ctrl Pts',(2.50919862475178,-0.574425642562403,-2.78508434954684));
#9146=CARTESIAN_POINT('Ctrl Pts',(2.47839070263651,-0.515297023926705,-2.78917202812655));
#9147=CARTESIAN_POINT('Ctrl Pts',(2.43954676301574,-0.422289475615677,-2.79558046347222));
#9148=CARTESIAN_POINT('Ctrl Pts',(2.42773646914373,-0.390136619642021,-2.79779068394603));
#9149=CARTESIAN_POINT('Ctrl Pts',(2.41443695070717,-0.348392093178328,-2.80067799789226));
#9150=CARTESIAN_POINT('Ctrl Pts',(2.41164124116129,-0.339232103672854,-2.80131257946533));
#9151=CARTESIAN_POINT('Ctrl Pts',(2.40729053770484,-0.324328611294449,-2.80234718099593));
#9152=CARTESIAN_POINT('Ctrl Pts',(2.40566677569756,-0.31860550845748,-2.80274498196999));
#9153=CARTESIAN_POINT('Ctrl Pts',(2.40263058552118,-0.307586924253439,-2.80351194039831));
#9154=CARTESIAN_POINT('Ctrl Pts',(2.40121162223718,-0.302293391912137,-2.80388087728166));
#9155=CARTESIAN_POINT('Ctrl Pts',(2.39804435933927,-0.290139133727082,-2.80472916029831));
#9156=CARTESIAN_POINT('Ctrl Pts',(2.3963208896416,-0.283272216609131,-2.80520928361004));
#9157=CARTESIAN_POINT('Ctrl Pts',(2.39102206727324,-0.26132351785221,-2.80674687234254));
#9158=CARTESIAN_POINT('Ctrl Pts',(2.38768260469289,-0.246187050675711,-2.80781172133476));
#9159=CARTESIAN_POINT('Ctrl Pts',(2.36935963841847,-0.154577960164166,-2.8142863291644));
#9160=CARTESIAN_POINT('Ctrl Pts',(2.3617001877326,-0.0768513395504396,-2.81992377176816));
#9161=CARTESIAN_POINT('Ctrl Pts',(2.36183524319387,0.0748995426607242,-2.83105050793921));
#9162=CARTESIAN_POINT('Ctrl Pts',(2.36884709221586,0.14858707453323,-2.83650379562567));
#9163=CARTESIAN_POINT('Ctrl Pts',(2.38452687808435,0.230610412638048,-2.84235479586892));
#9164=CARTESIAN_POINT('Ctrl Pts',(2.38645413805029,0.240061249095705,-2.84302540859916));
#9165=CARTESIAN_POINT('Ctrl Pts',(2.38931827618977,0.253275066697978,-2.84395707350117));
#9166=CARTESIAN_POINT('Ctrl Pts',(2.39015790003458,0.257058412619488,-2.84422313681158));
#9167=CARTESIAN_POINT('Ctrl Pts',(2.3917078613311,0.263883099285725,-2.84470175377106));
#9168=CARTESIAN_POINT('Ctrl Pts',(2.39241164933604,0.2669258830746,-2.84491466651426));
#9169=CARTESIAN_POINT('Ctrl Pts',(2.39387441982059,0.273137436772038,-2.84534828083118));
#9170=CARTESIAN_POINT('Ctrl Pts',(2.39463446173581,0.276305914225063,-2.84556892121881));
#9171=CARTESIAN_POINT('Ctrl Pts',(2.39661924858808,0.284431319942791,-2.84613344178053));
#9172=CARTESIAN_POINT('Ctrl Pts',(2.39786311222177,0.289383575791147,-2.8464762589737));
#9173=CARTESIAN_POINT('Ctrl Pts',(2.40321135187452,0.310105461421779,-2.84790609600727));
#9174=CARTESIAN_POINT('Ctrl Pts',(2.40761078629632,0.325797988927075,-2.84897765068756));
#9175=CARTESIAN_POINT('Ctrl Pts',(2.42049043011143,0.3683227135144,-2.85186331623996));
#9176=CARTESIAN_POINT('Ctrl Pts',(2.42960900065448,0.394951357489642,-2.8536504727228));
#9177=CARTESIAN_POINT('Ctrl Pts',(2.47001081814081,0.500441992274455,-2.86074316543338));
#9178=CARTESIAN_POINT('Ctrl Pts',(2.50881643998352,0.576144737026474,-2.86588065053091));
#9179=CARTESIAN_POINT('Ctrl Pts',(2.57675976314412,0.679484183467396,-2.8737022703326));
#9180=CARTESIAN_POINT('Ctrl Pts',(2.59969254572535,0.710865572105115,-2.87619844151437));
#9181=CARTESIAN_POINT('Ctrl Pts',(2.63064319301569,0.749097337641925,-2.8794346587919));
#9182=CARTESIAN_POINT('Ctrl Pts',(2.63725987636683,0.757053840289884,-2.88011944859016));
#9183=CARTESIAN_POINT('Ctrl Pts',(2.64795330045068,0.769573255148537,-2.88121571921039));
#9184=CARTESIAN_POINT('Ctrl Pts',(2.65196233903132,0.774193492121676,-2.88162445988091));
#9185=CARTESIAN_POINT('Ctrl Pts',(2.65924507690931,0.78245560395874,-2.88236305960074));
#9186=CARTESIAN_POINT('Ctrl Pts',(2.66250586409672,0.786108714098411,-2.88269238206574));
#9187=CARTESIAN_POINT('Ctrl Pts',(2.67022557207439,0.794649407414818,-2.88346888193945));
#9188=CARTESIAN_POINT('Ctrl Pts',(2.67470304495316,0.799519922078523,-2.8839168274462));
#9189=CARTESIAN_POINT('Ctrl Pts',(2.68789710546321,0.813631674369067,-2.88522997529913));
#9190=CARTESIAN_POINT('Ctrl Pts',(2.69672222941865,0.822769673289093,-2.88609975058559));
#9191=CARTESIAN_POINT('Ctrl Pts',(2.75544243813209,0.881635529218473,-2.89183407931891));
#9192=CARTESIAN_POINT('Ctrl Pts',(2.80955700845613,0.926935598762338,-2.89688685172822));
#9193=CARTESIAN_POINT('Ctrl Pts',(2.92891917880187,1.00989025676959,-2.90750836594389));
#9194=CARTESIAN_POINT('Ctrl Pts',(2.99439671839709,1.04668667507222,-2.91306538149354));
#9195=CARTESIAN_POINT('Ctrl Pts',(3.07927804988984,1.08424763401174,-2.919668682244));
#9196=CARTESIAN_POINT('Ctrl Pts',(3.09579125817803,1.09110972947562,-2.9209262365287));
#9197=CARTESIAN_POINT('Ctrl Pts',(3.11756094675155,1.09958011736903,-2.92254340301155));
#9198=CARTESIAN_POINT('Ctrl Pts',(3.12268045111398,1.10153105304701,-2.92292080691102));
#9199=CARTESIAN_POINT('Ctrl Pts',(3.13094325152188,1.10461397690072,-2.92352506638373));
#9200=CARTESIAN_POINT('Ctrl Pts',(3.13407800040985,1.10576841023846,-2.92375319036565));
#9201=CARTESIAN_POINT('Ctrl Pts',(3.14014190090279,1.10797230814809,-2.92419225802817));
#9202=CARTESIAN_POINT('Ctrl Pts',(3.14307033957583,1.10902351782215,-2.92440329559957));
#9203=CARTESIAN_POINT('Ctrl Pts',(3.15014043093986,1.11152985715307,-2.92491045940089));
#9204=CARTESIAN_POINT('Ctrl Pts',(3.15428617306356,1.11297347874417,-2.9252059207994));
#9205=CARTESIAN_POINT('Ctrl Pts',(3.16879417479833,1.11793464719039,-2.92623348568788));
#9206=CARTESIAN_POINT('Ctrl Pts',(3.17919767980351,1.12133105717032,-2.92695897524762));
#9207=CARTESIAN_POINT('Ctrl Pts',(3.20503835131956,1.12937041381321,-2.92873651172546));
#9208=CARTESIAN_POINT('Ctrl Pts',(3.22052671523768,1.13384249926455,-2.92978056944618));
#9209=CARTESIAN_POINT('Ctrl Pts',(3.28711731929589,1.15159711617302,-2.9341977534465));
#9210=CARTESIAN_POINT('Ctrl Pts',(3.33899277892716,1.16175411399418,-2.93746206694308));
#9211=CARTESIAN_POINT('Ctrl Pts',(3.47218680818687,1.17864177879736,-2.94576709366524));
#9212=CARTESIAN_POINT('Ctrl Pts',(3.55383019208463,1.18047584862365,-2.95080150113667));
#9213=CARTESIAN_POINT('Ctrl Pts',(3.65036408158042,1.17262351110741,-2.95711383275943));
#9214=CARTESIAN_POINT('Ctrl Pts',(3.66569638951891,1.17107291109217,-2.95812658599492));
#9215=CARTESIAN_POINT('Ctrl Pts',(3.68800579075667,1.16837350421285,-2.9596170929776));
#9216=CARTESIAN_POINT('Ctrl Pts',(3.69501036944245,1.16746194947664,-2.96008750865481));
#9217=CARTESIAN_POINT('Ctrl Pts',(3.70743185487514,1.16573168505209,-2.96092623525085));
#9218=CARTESIAN_POINT('Ctrl Pts',(3.71285209198115,1.16493807835835,-2.96129375483313));
#9219=CARTESIAN_POINT('Ctrl Pts',(3.7241541323763,1.16320266088734,-2.9620633854663));
#9220=CARTESIAN_POINT('Ctrl Pts',(3.73003470803057,1.16225398504054,-2.96246570129351));
#9221=CARTESIAN_POINT('Ctrl Pts',(3.74538514863154,1.15965796779391,-2.96352090887798));
#9222=CARTESIAN_POINT('Ctrl Pts',(3.7548423262836,1.15793926008036,-2.96417601432317));
#9223=CARTESIAN_POINT('Ctrl Pts',(3.79827410539926,1.14949569767008,-2.96720840084931));
#9224=CARTESIAN_POINT('Ctrl Pts',(3.83195960865803,1.1413906570153,-2.96962842398467));
#9225=CARTESIAN_POINT('Ctrl Pts',(3.9305775594233,1.11301005192873,-2.97692129466239));
#9226=CARTESIAN_POINT('Ctrl Pts',(3.99416128827089,1.08858471369999,-2.98190543918507));
#9227=CARTESIAN_POINT('Ctrl Pts',(4.07809681896068,1.04769911045244,-2.98875613486848));
#9228=CARTESIAN_POINT('Ctrl Pts',(4.10055312323137,1.03584760849696,-2.99061629496205));
#9229=CARTESIAN_POINT('Ctrl Pts',(4.13649242886478,1.01536849010507,-2.99362343919519));
#9230=CARTESIAN_POINT('Ctrl Pts',(4.15021358238763,1.00717556059032,-2.99477893875998));
#9231=CARTESIAN_POINT('Ctrl Pts',(4.18385514791999,0.986147759027043,-2.99762386402038));
#9232=CARTESIAN_POINT('Ctrl Pts',(4.20356425842518,0.972985382392181,-2.99930126104937));
#9233=CARTESIAN_POINT('Ctrl Pts',(4.22778394907507,0.955731644877706,-3.0013638055988));
#9234=CARTESIAN_POINT('Ctrl Pts',(4.2326766615559,0.952189097687222,-3.0017805295991));
#9235=CARTESIAN_POINT('Ctrl Pts',(4.24033242442056,0.946555692800768,-3.00243241348149));
#9236=CARTESIAN_POINT('Ctrl Pts',(4.24311378988524,0.944490078365305,-3.00266920817979));
#9237=CARTESIAN_POINT('Ctrl Pts',(4.24834109212685,0.94057205414652,-3.0031141079217));
#9238=CARTESIAN_POINT('Ctrl Pts',(4.25078888783022,0.938722373484953,-3.00332237844579));
#9239=CARTESIAN_POINT('Ctrl Pts',(4.25650196318259,0.934370102917066,-3.00380837484998));
#9240=CARTESIAN_POINT('Ctrl Pts',(4.25976139332397,0.931859943971826,-3.00408557452722));
#9241=CARTESIAN_POINT('Ctrl Pts',(4.2703463713036,0.92361950331609,-3.00498579089503));
#9242=CARTESIAN_POINT('Ctrl Pts',(4.27761742887499,0.917819348700225,-3.00560418907907));
#9243=CARTESIAN_POINT('Ctrl Pts',(4.31722890209964,0.885445889293677,-3.00897802170675));
#9244=CARTESIAN_POINT('Ctrl Pts',(4.34820714564328,0.857246388547044,-3.01163524727034));
#9245=CARTESIAN_POINT('Ctrl Pts',(4.42941672544203,0.774991806784186,-3.01886716324334));
#9246=CARTESIAN_POINT('Ctrl Pts',(4.47617196535344,0.717782524193531,-3.02335472003506));
#9247=CARTESIAN_POINT('Ctrl Pts',(4.54221317293923,0.619436069024034,-3.03080749755189));
#9248=CARTESIAN_POINT('Ctrl Pts',(4.56501481159752,0.580908164784793,-3.03366873407391));
#9249=CARTESIAN_POINT('Ctrl Pts',(4.59044763483391,0.531748927645906,-3.03730711659445));
#9250=CARTESIAN_POINT('Ctrl Pts',(4.5951988950759,0.522252683228913,-3.03800929981587));
#9251=CARTESIAN_POINT('Ctrl Pts',(4.60253594345096,0.5070789334289,-3.03913092362594));
#9252=CARTESIAN_POINT('Ctrl Pts',(4.60520621607486,0.501442740531811,-3.03954746167587));
#9253=CARTESIAN_POINT('Ctrl Pts',(4.6101156057203,0.490864052200142,-3.04032925083983));
#9254=CARTESIAN_POINT('Ctrl Pts',(4.61236558545537,0.485926756351989,-3.04069412011171));
#9255=CARTESIAN_POINT('Ctrl Pts',(4.61731886118822,0.474855309311859,-3.04151238006665));
#9256=CARTESIAN_POINT('Ctrl Pts',(4.6200040459766,0.468713311139167,-3.04196636822741));
#9257=CARTESIAN_POINT('Ctrl Pts',(4.62779530919577,0.450469066727201,-3.04331523884543));
#9258=CARTESIAN_POINT('Ctrl Pts',(4.63275137798849,0.438304288431218,-3.04421508189992));
#9259=CARTESIAN_POINT('Ctrl Pts',(4.66604231991797,0.352511327546618,-3.05056683363867));
#9260=CARTESIAN_POINT('Ctrl Pts',(4.68711461112448,0.276295233872228,-3.05625822540346));
#9261=CARTESIAN_POINT('Ctrl Pts',(4.71336463499763,0.122823006347651,-3.06766803820147));
#9262=CARTESIAN_POINT('Ctrl Pts',(4.71887708067265,0.0459944917971725,-3.07335114027535));
#9263=CARTESIAN_POINT('Ctrl Pts',(4.71661769191039,-0.040292448793193,-3.07939638705071));
#9264=CARTESIAN_POINT('Ctrl Pts',(4.7162557612288,-0.0497536006386948,-3.08005447272371));
#9265=CARTESIAN_POINT('Ctrl Pts',(4.71558647540485,-0.0630496367147106,
-3.08097167532275));
#9266=CARTESIAN_POINT('Ctrl Pts',(4.71537437936358,-0.0668886480235825,
-3.08123560754887));
#9267=CARTESIAN_POINT('Ctrl Pts',(4.71495642520805,-0.0738359208558632,
-3.08171153084766));
#9268=CARTESIAN_POINT('Ctrl Pts',(4.71475702857496,-0.0769445305130917,
-3.08192386863788));
#9269=CARTESIAN_POINT('Ctrl Pts',(4.7143230205281,-0.083314994928684,-3.08235769795794));
#9270=CARTESIAN_POINT('Ctrl Pts',(4.71408715356602,-0.0865767191283937,
-3.08257911951936));
#9271=CARTESIAN_POINT('Ctrl Pts',(4.71344409921951,-0.0949824625354806,
-3.08314802887223));
#9272=CARTESIAN_POINT('Ctrl Pts',(4.71301668094232,-0.100124931904641,-3.08349442159543));
#9273=CARTESIAN_POINT('Ctrl Pts',(4.71105559052224,-0.121978733833372,-3.08496006975015));
#9274=CARTESIAN_POINT('Ctrl Pts',(4.70919855654215,-0.138660015302232,-3.08606287801184));
#9275=CARTESIAN_POINT('Ctrl Pts',(4.70311045986344,-0.184428137373731,-3.08905871835853));
#9276=CARTESIAN_POINT('Ctrl Pts',(4.69814614018654,-0.213406222610518,-3.09092222271414));
#9277=CARTESIAN_POINT('Ctrl Pts',(4.67176970809976,-0.338942110519832,-3.09896414320742));
#9278=CARTESIAN_POINT('Ctrl Pts',(4.63933208403852,-0.432764229062663,-3.10492954575326));
#9279=CARTESIAN_POINT('Ctrl Pts',(4.58417377415846,-0.544474066613465,-3.11292500272328));
#9280=CARTESIAN_POINT('Ctrl Pts',(4.57204550526483,-0.567137079342937,-3.11459516879936));
#9281=CARTESIAN_POINT('Ctrl Pts',(4.55469807558289,-0.597149102400174,-3.11688292310302));
#9282=CARTESIAN_POINT('Ctrl Pts',(4.55012130311004,-0.604862449771233,-3.11747786294999));
#9283=CARTESIAN_POINT('Ctrl Pts',(4.54243145243252,-0.617491391945533,-3.11846390342629));
#9284=CARTESIAN_POINT('Ctrl Pts',(4.53936919452817,-0.622437621377973,-3.11885316566017));
#9285=CARTESIAN_POINT('Ctrl Pts',(4.53332257392306,-0.632044496402879,-3.11961534360429));
#9286=CARTESIAN_POINT('Ctrl Pts',(4.53034175313901,-0.636707200164753,-3.11998812283273));
#9287=CARTESIAN_POINT('Ctrl Pts',(4.52322112801467,-0.647674431118855,-3.12087181936196));
#9288=CARTESIAN_POINT('Ctrl Pts',(4.51905344718641,-0.653960478284892,-3.12138375493938));
#9289=CARTESIAN_POINT('Ctrl Pts',(4.50490111068044,-0.674867392270231,-3.1231049975264));
#9290=CARTESIAN_POINT('Ctrl Pts',(4.49464761806124,-0.689302458850134,-3.12432425689994));
#9291=CARTESIAN_POINT('Ctrl Pts',(4.43174018789539,-0.773765068565763,-3.131648665262));
#9292=CARTESIAN_POINT('Ctrl Pts',(4.37173890373178,-0.837959298383006,-3.1380419329809));
#9293=CARTESIAN_POINT('Ctrl Pts',(4.25928925017479,-0.934170902709694,-3.14890258317132));
#9294=CARTESIAN_POINT('Ctrl Pts',(4.21042926884041,-0.969858418313633,-3.15332771524153));
#9295=CARTESIAN_POINT('Ctrl Pts',(4.15052345754858,-1.00691062518918,-3.15826714305432));
#9296=CARTESIAN_POINT('Ctrl Pts',(4.14193749774653,-1.01207085895719,-3.15896405732997));
#9297=CARTESIAN_POINT('Ctrl Pts',(4.12988556169194,-1.01910644785608,-3.15992597233075));
#9298=CARTESIAN_POINT('Ctrl Pts',(4.12647472527301,-1.02107473113599,-3.1601964072787));
#9299=CARTESIAN_POINT('Ctrl Pts',(4.1205727225867,-1.02444123919993,-3.16066118221608));
#9300=CARTESIAN_POINT('Ctrl Pts',(4.11808625028956,-1.02584756089346,-3.16085602253505));
#9301=CARTESIAN_POINT('Ctrl Pts',(4.11282860208563,-1.02879603309051,-3.16126593870442));
#9302=CARTESIAN_POINT('Ctrl Pts',(4.11005626905409,-1.03033606280896,-3.16148087406596));
#9303=CARTESIAN_POINT('Ctrl Pts',(4.1031595129035,-1.03413083585424,-3.16201265489975));
#9304=CARTESIAN_POINT('Ctrl Pts',(4.09902769247929,-1.0363721522411,-3.16232866844552));
#9305=CARTESIAN_POINT('Ctrl Pts',(4.08933494865176,-1.04155514270696,-3.16306426060349));
#9306=CARTESIAN_POINT('Ctrl Pts',(4.08376370001831,-1.04447709396206,-3.16348268836972));
#9307=CARTESIAN_POINT('Ctrl Pts',(4.07816926753082,-1.04735428872454,-3.16389876579091));
#9308=CARTESIAN_POINT('Origin',(3.53951905042299,8.32667268468867E-16,0.924367114736157));
#9309=CARTESIAN_POINT('',(4.07816926790565,-1.04735428853177,-3.76191690485895));
#9310=CARTESIAN_POINT('',(4.07816923053759,-1.04735430775001,-3.66210420774532));
#9311=CARTESIAN_POINT('',(4.07816926754759,-1.04735428871592,0.924367114736157));
#9312=CARTESIAN_POINT('Ctrl Pts',(4.07816926790565,-1.04735428853177,-3.76191690485895));
#9313=CARTESIAN_POINT('Ctrl Pts',(4.07913040768384,-1.04685997810002,-3.76184957489129));
#9314=CARTESIAN_POINT('Ctrl Pts',(4.08009089746488,-1.0463643289823,-3.761782224073));
#9315=CARTESIAN_POINT('Ctrl Pts',(4.11564773853268,-1.02795362310974,-3.75928643561599));
#9316=CARTESIAN_POINT('Ctrl Pts',(4.14933213202587,-1.00833553976734,-3.75683339652415));
#9317=CARTESIAN_POINT('Ctrl Pts',(4.19576812665263,-0.978111870791754,-3.75327013250654));
#9318=CARTESIAN_POINT('Ctrl Pts',(4.20936541715728,-0.96885060086797,-3.75220341416066));
#9319=CARTESIAN_POINT('Ctrl Pts',(4.23326615670184,-0.951827855217013,-3.75028257824101));
#9320=CARTESIAN_POINT('Ctrl Pts',(4.24364462199304,-0.944176080840029,-3.74943248778705));
#9321=CARTESIAN_POINT('Ctrl Pts',(4.25918621132288,-0.932318900452617,-3.74813376356517));
#9322=CARTESIAN_POINT('Ctrl Pts',(4.26444296706617,-0.928237397783566,-3.74768991086955));
#9323=CARTESIAN_POINT('Ctrl Pts',(4.2739203505149,-0.920749264722594,-3.74688117308109));
#9324=CARTESIAN_POINT('Ctrl Pts',(4.27815260316191,-0.917357591755194,-3.74651688280406));
#9325=CARTESIAN_POINT('Ctrl Pts',(4.28723076988238,-0.909978914539727,-3.74572858673261));
#9326=CARTESIAN_POINT('Ctrl Pts',(4.29206852757928,-0.905982186427791,-3.74530420012196));
#9327=CARTESIAN_POINT('Ctrl Pts',(4.30513347654585,-0.895011693009504,-3.74414616680766));
#9328=CARTESIAN_POINT('Ctrl Pts',(4.31329701650725,-0.88796341473122,-3.74340952778165));
#9329=CARTESIAN_POINT('Ctrl Pts',(4.35696903772125,-0.84919807072921,-3.73939614747191));
#9330=CARTESIAN_POINT('Ctrl Pts',(4.39062172332617,-0.815466138952654,-3.73603627742989));
#9331=CARTESIAN_POINT('Ctrl Pts',(4.47369508999095,-0.72143867311156,-3.72700399104586));
#9332=CARTESIAN_POINT('Ctrl Pts',(4.5193364470668,-0.658114769689083,-3.72123031367233));
#9333=CARTESIAN_POINT('Ctrl Pts',(4.57154702260122,-0.568068013996911,-3.71366271554842));
#9334=CARTESIAN_POINT('Ctrl Pts',(4.58394252942266,-0.544942914614651,-3.71177235849283));
#9335=CARTESIAN_POINT('Ctrl Pts',(4.60019133093315,-0.512034166401618,-3.70917251056938));
#9336=CARTESIAN_POINT('Ctrl Pts',(4.60470128900284,-0.502584808570494,-3.70843612169731));
#9337=CARTESIAN_POINT('Ctrl Pts',(4.61238262758632,-0.485922685028345,-3.70715679460331));
#9338=CARTESIAN_POINT('Ctrl Pts',(4.6156087080141,-0.478736010989915,-3.70661114642421));
#9339=CARTESIAN_POINT('Ctrl Pts',(4.62030305592095,-0.467991241391654,-3.70580503026968));
#9340=CARTESIAN_POINT('Ctrl Pts',(4.62182630327857,-0.464457619199869,-3.7055414685735));
#9341=CARTESIAN_POINT('Ctrl Pts',(4.62440861127644,-0.458385501473841,-3.70509129008527));
#9342=CARTESIAN_POINT('Ctrl Pts',(4.62547612573965,-0.455850697419985,-3.70490417570074));
#9343=CARTESIAN_POINT('Ctrl Pts',(4.62788982772629,-0.450062782041408,-3.70447878315827));
#9344=CARTESIAN_POINT('Ctrl Pts',(4.62923031620903,-0.446807357482324,-3.70424084560102));
#9345=CARTESIAN_POINT('Ctrl Pts',(4.63286515675581,-0.4378663528556,-3.70359084847328));
#9346=CARTESIAN_POINT('Ctrl Pts',(4.63512978205513,-0.432168693839955,-3.70318049874956));
#9347=CARTESIAN_POINT('Ctrl Pts',(4.64669944591711,-0.402384591266964,-3.70105418308748));
#9348=CARTESIAN_POINT('Ctrl Pts',(4.65525578379767,-0.378012644262554,-3.69937784663078));
#9349=CARTESIAN_POINT('Ctrl Pts',(4.69291802244623,-0.258273751545842,-3.69135780128932));
#9350=CARTESIAN_POINT('Ctrl Pts',(4.71063673094573,-0.159752786772782,-3.68538053575237));
#9351=CARTESIAN_POINT('Ctrl Pts',(4.71711618857534,-0.0330932096947441,
-3.67737082054352));
#9352=CARTESIAN_POINT('Ctrl Pts',(4.71756586535087,-0.00597737547596642,
-3.67563990514936));
#9353=CARTESIAN_POINT('Ctrl Pts',(4.71674028366827,0.0400350078241747,-3.67265703435896));
#9354=CARTESIAN_POINT('Ctrl Pts',(4.71594578446671,0.0589296926818208,-3.67141909724141));
#9355=CARTESIAN_POINT('Ctrl Pts',(4.71418562626999,0.0855183635478312,-3.66965486510587));
#9356=CARTESIAN_POINT('Ctrl Pts',(4.71359833520841,0.0932350963669577,-3.66914020458147));
#9357=CARTESIAN_POINT('Ctrl Pts',(4.71245768337484,0.106494343779003,-3.66825110682771));
#9358=CARTESIAN_POINT('Ctrl Pts',(4.71194097070631,0.112039818611494,-3.66787781374963));
#9359=CARTESIAN_POINT('Ctrl Pts',(4.71087767805621,0.122637047736332,-3.66716161340163));
#9360=CARTESIAN_POINT('Ctrl Pts',(4.71033769923394,0.127689350427545,-3.66681891907835));
#9361=CARTESIAN_POINT('Ctrl Pts',(4.70899435805145,0.139532533501534,-3.66601261776856));
#9362=CARTESIAN_POINT('Ctrl Pts',(4.70816451799257,0.146320165290306,-3.66554819793542));
#9363=CARTESIAN_POINT('Ctrl Pts',(4.70553512146864,0.166375644178311,-3.66416894962612));
#9364=CARTESIAN_POINT('Ctrl Pts',(4.70356841932231,0.179620082701609,-3.66324898203622));
#9365=CARTESIAN_POINT('Ctrl Pts',(4.68641257396649,0.282990345069766,-3.65599471603356));
#9366=CARTESIAN_POINT('Ctrl Pts',(4.66100707201946,0.371088524346489,-3.64933334001237));
#9367=CARTESIAN_POINT('Ctrl Pts',(4.60795979972711,0.497625507950008,-3.63926398568833));
#9368=CARTESIAN_POINT('Ctrl Pts',(4.58778065409507,0.538836604957881,-3.63590395664767));
#9369=CARTESIAN_POINT('Ctrl Pts',(4.55793853455741,0.591724706893877,-3.6315594540595));
#9370=CARTESIAN_POINT('Ctrl Pts',(4.55038271832034,0.604542027586616,-3.63050408280422));
#9371=CARTESIAN_POINT('Ctrl Pts',(4.53718488130465,0.625990543464053,-3.62873786458802));
#9372=CARTESIAN_POINT('Ctrl Pts',(4.5316688386142,0.634696846124991,-3.62802088628616));
#9373=CARTESIAN_POINT('Ctrl Pts',(4.52369733746608,0.646920813731741,-3.62701536518473));
#9374=CARTESIAN_POINT('Ctrl Pts',(4.52133604766966,0.650498904908845,-3.6267211791538));
#9375=CARTESIAN_POINT('Ctrl Pts',(4.51723689446967,0.656637231386399,-3.62621684548329));
#9376=CARTESIAN_POINT('Ctrl Pts',(4.51550839725881,0.659203634695818,-3.62600609476067));
#9377=CARTESIAN_POINT('Ctrl Pts',(4.51186927544589,0.664561165290996,-3.62556640418511));
#9378=CARTESIAN_POINT('Ctrl Pts',(4.50995672343349,0.667350901733266,-3.62533759457949));
#9379=CARTESIAN_POINT('Ctrl Pts',(4.50480830310536,0.674791688798884,-3.62472758490312));
#9380=CARTESIAN_POINT('Ctrl Pts',(4.50155079635148,0.679427764842924,-3.62434779627613));
#9381=CARTESIAN_POINT('Ctrl Pts',(4.48686800385198,0.700006951953834,-3.62266234343192));
#9382=CARTESIAN_POINT('Ctrl Pts',(4.47507823580574,0.715687705074197,-3.62137914501653));
#9383=CARTESIAN_POINT('Ctrl Pts',(4.40984906847535,0.798076061005048,-3.61459937138855));
#9384=CARTESIAN_POINT('Ctrl Pts',(4.34965543213657,0.859116851982129,-3.60942454688346));
#9385=CARTESIAN_POINT('Ctrl Pts',(4.24056146039214,0.947989794624799,-3.60066308310607));
#9386=CARTESIAN_POINT('Ctrl Pts',(4.19534830471168,0.979812238336118,-3.59717724242399));
#9387=CARTESIAN_POINT('Ctrl Pts',(4.13581582552705,1.01574120085896,-3.59263698308964));
#9388=CARTESIAN_POINT('Ctrl Pts',(4.1234249907903,1.02291439283484,-3.59169481078906));
#9389=CARTESIAN_POINT('Ctrl Pts',(4.10484187890954,1.03322469474088,-3.59028430386699));
#9390=CARTESIAN_POINT('Ctrl Pts',(4.09874736112685,1.03653599227891,-3.58982211125941));
#9391=CARTESIAN_POINT('Ctrl Pts',(4.08781470247116,1.04235148348792,-3.58899353036805));
#9392=CARTESIAN_POINT('Ctrl Pts',(4.08298772559053,1.04487632502354,-3.58862787659347));
#9393=CARTESIAN_POINT('Ctrl Pts',(4.07273129502628,1.05015084779492,-3.58785121994767));
#9394=CARTESIAN_POINT('Ctrl Pts',(4.06729771237416,1.05289210392618,-3.58743993811942));
#9395=CARTESIAN_POINT('Ctrl Pts',(4.05269929998366,1.06011564312644,-3.58633526259548));
#9396=CARTESIAN_POINT('Ctrl Pts',(4.0434972399904,1.06452107467316,-3.58563926063488));
#9397=CARTESIAN_POINT('Ctrl Pts',(4.00054209790992,1.08440379918564,-3.58239097210093));
#9398=CARTESIAN_POINT('Ctrl Pts',(3.96612961488669,1.09839735843773,-3.57978954652323));
#9399=CARTESIAN_POINT('Ctrl Pts',(3.85766511125709,1.13663709834693,-3.57158960543992));
#9400=CARTESIAN_POINT('Ctrl Pts',(3.7818313782277,1.15518101492718,-3.5658414895152));
#9401=CARTESIAN_POINT('Ctrl Pts',(3.67078668784452,1.17091391571905,-3.55763800950096));
#9402=CARTESIAN_POINT('Ctrl Pts',(3.6366435066062,1.17423922092827,-3.55514695149548));
#9403=CARTESIAN_POINT('Ctrl Pts',(3.58385015865952,1.17706200483605,-3.55138375943416));
#9404=CARTESIAN_POINT('Ctrl Pts',(3.56527631492614,1.17761490684344,-3.55007671581533));
#9405=CARTESIAN_POINT('Ctrl Pts',(3.54134826138731,1.17776072071589,-3.54842092535495));
#9406=CARTESIAN_POINT('Ctrl Pts',(3.53600028981212,1.17775688592068,-3.54805265727843));
#9407=CARTESIAN_POINT('Ctrl Pts',(3.5273405797559,1.17769168976857,-3.54745945674535));
#9408=CARTESIAN_POINT('Ctrl Pts',(3.52402882385823,1.17765278620937,-3.54723333600872));
#9409=CARTESIAN_POINT('Ctrl Pts',(3.5176265450913,1.17755056598212,-3.5467976839724));
#9410=CARTESIAN_POINT('Ctrl Pts',(3.51453605982117,1.17748905203869,-3.54658806176255));
#9411=CARTESIAN_POINT('Ctrl Pts',(3.50769720608287,1.17732599259622,-3.546125621358));
#9412=CARTESIAN_POINT('Ctrl Pts',(3.50394897312646,1.17721871085199,-3.54587311516853));
#9413=CARTESIAN_POINT('Ctrl Pts',(3.49063347920839,1.17677394084557,-3.54497925854029));
#9414=CARTESIAN_POINT('Ctrl Pts',(3.48106958058478,1.17633769845862,-3.54434304876719));
#9415=CARTESIAN_POINT('Ctrl Pts',(3.39259245570817,1.17122018450565,-3.53850234645005));
#9416=CARTESIAN_POINT('Ctrl Pts',(3.31432125711008,1.15872075229503,-3.53365785630778));
#9417=CARTESIAN_POINT('Ctrl Pts',(3.18602824906264,1.12472979671431,-3.5254455112722));
#9418=CARTESIAN_POINT('Ctrl Pts',(3.1351744660868,1.1074645372386,-3.52211528317582));
#9419=CARTESIAN_POINT('Ctrl Pts',(3.06712775260272,1.07904848134746,-3.51740583289004));
#9420=CARTESIAN_POINT('Ctrl Pts',(3.04878017546468,1.07082886143696,-3.51610987910902));
#9421=CARTESIAN_POINT('Ctrl Pts',(3.01706022422097,1.0556320377273,-3.51381624026388));
#9422=CARTESIAN_POINT('Ctrl Pts',(3.00359455778155,1.04885991859225,-3.51282528670459));
#9423=CARTESIAN_POINT('Ctrl Pts',(2.98400129684174,1.03853030539245,-3.51135588899236));
#9424=CARTESIAN_POINT('Ctrl Pts',(2.97776956796749,1.03517278029445,-3.51088437414969));
#9425=CARTESIAN_POINT('Ctrl Pts',(2.96678149065349,1.0291241958636,-3.51004536696797));
#9426=CARTESIAN_POINT('Ctrl Pts',(2.96201285313594,1.02645580190351,-3.50967868035459));
#9427=CARTESIAN_POINT('Ctrl Pts',(2.95203986826865,1.02078370831495,-3.50890629107291));
#9428=CARTESIAN_POINT('Ctrl Pts',(2.9468396070646,1.01777317892497,-3.50850035329362));
#9429=CARTESIAN_POINT('Ctrl Pts',(2.93317727489808,1.00972358128782,-3.50742527847184));
#9430=CARTESIAN_POINT('Ctrl Pts',(2.92475513269853,1.00461802422746,-3.50675377269525));
#9431=CARTESIAN_POINT('Ctrl Pts',(2.88813167708821,0.981783658794715,-3.50379425848971));
#9432=CARTESIAN_POINT('Ctrl Pts',(2.86062821320882,0.962970152776744,-3.50146721340666));
#9433=CARTESIAN_POINT('Ctrl Pts',(2.7690877260293,0.89448035155823,-3.49334886704103));
#9434=CARTESIAN_POINT('Ctrl Pts',(2.70940209091129,0.839382163000545,-3.4873737131628));
#9435=CARTESIAN_POINT('Ctrl Pts',(2.6218978513112,0.740070382245344,-3.47768724635673));
#9436=CARTESIAN_POINT('Ctrl Pts',(2.59049722167838,0.699350887025435,-3.47396340714033));
#9437=CARTESIAN_POINT('Ctrl Pts',(2.55798154453704,0.650943460101822,-3.46990768228305));
#9438=CARTESIAN_POINT('Ctrl Pts',(2.55416124778644,0.645145929466778,-3.46942769117538));
#9439=CARTESIAN_POINT('Ctrl Pts',(2.54840654187993,0.636242438506985,-3.46869967140879));
#9440=CARTESIAN_POINT('Ctrl Pts',(2.54643504621833,0.633160806316008,-3.46844934168098));
#9441=CARTESIAN_POINT('Ctrl Pts',(2.54285043239605,0.627499787201232,-3.46799256367277));
#9442=CARTESIAN_POINT('Ctrl Pts',(2.54123294303013,0.62492332755839,-3.4677858411787));
#9443=CARTESIAN_POINT('Ctrl Pts',(2.53760180503328,0.619089299956832,-3.46732035927917));
#9444=CARTESIAN_POINT('Ctrl Pts',(2.53559404947504,0.615828159016731,-3.46706197999346));
#9445=CARTESIAN_POINT('Ctrl Pts',(2.53044216367006,0.607367939266451,-3.46639621163821));
#9446=CARTESIAN_POINT('Ctrl Pts',(2.52732224682173,0.602154142763915,-3.46599031462872));
#9447=CARTESIAN_POINT('Ctrl Pts',(2.50652066783282,0.56677338603445,-3.46326382727266));
#9448=CARTESIAN_POINT('Ctrl Pts',(2.49014784556306,0.535852891814161,-3.46101715709204));
#9449=CARTESIAN_POINT('Ctrl Pts',(2.43618139178108,0.421942460225974,-3.45305531087221));
#9450=CARTESIAN_POINT('Ctrl Pts',(2.40686622677984,0.335392811262,-3.44756195870265));
#9451=CARTESIAN_POINT('Ctrl Pts',(2.37951902092388,0.207530633690691,-3.43929402626011));
#9452=CARTESIAN_POINT('Ctrl Pts',(2.37318769978433,0.16834399623778,-3.43674449872643));
#9453=CARTESIAN_POINT('Ctrl Pts',(2.36774883917496,0.118954059385286,-3.43347314585464));
#9454=CARTESIAN_POINT('Ctrl Pts',(2.36677909526317,0.108979280658975,-3.43280960311076));
#9455=CARTESIAN_POINT('Ctrl Pts',(2.36542855198598,0.0929684089631018,-3.4317393974354));
#9456=CARTESIAN_POINT('Ctrl Pts',(2.36496673391375,0.086939502322136,-3.43133524838191));
#9457=CARTESIAN_POINT('Ctrl Pts',(2.36417659427538,0.0754647974873236,-3.43056370832573));
#9458=CARTESIAN_POINT('Ctrl Pts',(2.3638396469709,0.0700197362499726,-3.4301965946374));
#9459=CARTESIAN_POINT('Ctrl Pts',(2.36315641229044,0.0575768549608456,-3.42935530891398));
#9460=CARTESIAN_POINT('Ctrl Pts',(2.36283471799604,0.0505779474917043,-3.4288803895385));
#9461=CARTESIAN_POINT('Ctrl Pts',(2.3620321106912,0.0289006941063898,-3.42740393499206));
#9462=CARTESIAN_POINT('Ctrl Pts',(2.36176330164812,0.0142163969199187,-3.42639592784049));
#9463=CARTESIAN_POINT('Ctrl Pts',(2.36179229001102,-0.0586529238535955,
-3.42135267703571));
#9464=CARTESIAN_POINT('Ctrl Pts',(2.36612702697649,-0.116746921123347,-3.41719611126923));
#9465=CARTESIAN_POINT('Ctrl Pts',(2.38376036848421,-0.234600825214178,-3.40852461121926));
#9466=CARTESIAN_POINT('Ctrl Pts',(2.39745873432777,-0.294132094370935,-3.40401486542645));
#9467=CARTESIAN_POINT('Ctrl Pts',(2.42064731600968,-0.36809501408863,-3.39837923807716));
#9468=CARTESIAN_POINT('Ctrl Pts',(2.42591994151369,-0.383751171894167,-3.39718482853545));
#9469=CARTESIAN_POINT('Ctrl Pts',(2.43943908531861,-0.421265578299721,-3.39432650354487));
#9470=CARTESIAN_POINT('Ctrl Pts',(2.4480104194524,-0.443000792461012,-3.39267345285986));
#9471=CARTESIAN_POINT('Ctrl Pts',(2.45959453870256,-0.469993900498081,-3.39063627515722));
#9472=CARTESIAN_POINT('Ctrl Pts',(2.46200818721363,-0.47550137857206,-3.39022146981295));
#9473=CARTESIAN_POINT('Ctrl Pts',(2.4658765214276,-0.484147441832999,-3.38957188265893));
#9474=CARTESIAN_POINT('Ctrl Pts',(2.46730299348854,-0.487298423485471,-3.38933548490488));
#9475=CARTESIAN_POINT('Ctrl Pts',(2.47002183568154,-0.493234422993762,-3.38889084801167));
#9476=CARTESIAN_POINT('Ctrl Pts',(2.47131120454452,-0.496020651389935,-3.38868244698977));
#9477=CARTESIAN_POINT('Ctrl Pts',(2.47435902725332,-0.5025397626296,-3.38819549758624));
#9478=CARTESIAN_POINT('Ctrl Pts',(2.47612622151347,-0.506268486763313,-3.38791748155108));
#9479=CARTESIAN_POINT('Ctrl Pts',(2.48196940626618,-0.518431834238853,-3.38701197611357));
#9480=CARTESIAN_POINT('Ctrl Pts',(2.48612655957959,-0.526827381966958,-3.38638918009597));
#9481=CARTESIAN_POINT('Ctrl Pts',(2.50968661975854,-0.573013765869746,-3.38297038948569));
#9482=CARTESIAN_POINT('Ctrl Pts',(2.53102505680056,-0.609787072918135,-3.38027549290668));
#9483=CARTESIAN_POINT('Ctrl Pts',(2.56704905547136,-0.664784173335619,-3.37616427310001));
#9484=CARTESIAN_POINT('Ctrl Pts',(2.58036531360688,-0.683856740537999,-3.37472244524226));
#9485=CARTESIAN_POINT('Ctrl Pts',(2.64628668496426,-0.772557393307044,-3.36788228339454));
#9486=CARTESIAN_POINT('Ctrl Pts',(2.70595046368155,-0.836582497546907,-3.36251284843542));
#9487=CARTESIAN_POINT('Ctrl Pts',(2.7836309232053,-0.903303875352328,-3.35583607373008));
#9488=CARTESIAN_POINT('Ctrl Pts',(2.79531682443236,-0.912955510894286,-3.35483972156162));
#9489=CARTESIAN_POINT('Ctrl Pts',(2.81268160761175,-0.926742492323955,-3.35336887146596));
#9490=CARTESIAN_POINT('Ctrl Pts',(2.8182167185411,-0.9310570647421,-3.35290143382411));
#9491=CARTESIAN_POINT('Ctrl Pts',(2.82813577062354,-0.938647344216288,-3.35206606437501));
#9492=CARTESIAN_POINT('Ctrl Pts',(2.832504640965,-0.941942477372226,-3.35169890121372));
#9493=CARTESIAN_POINT('Ctrl Pts',(2.84169561916302,-0.948774621884138,-3.35092801074458));
#9494=CARTESIAN_POINT('Ctrl Pts',(2.8465220089522,-0.952305582565559,-3.3505240651533));
#9495=CARTESIAN_POINT('Ctrl Pts',(2.85926084867646,-0.961477125330561,-3.34946001733772));
#9496=CARTESIAN_POINT('Ctrl Pts',(2.86721644276734,-0.967056708526007,-3.34879763326682));
#9497=CARTESIAN_POINT('Ctrl Pts',(2.90483268352598,-0.992750003713544,-3.34567482152017));
#9498=CARTESIAN_POINT('Ctrl Pts',(2.93532951997544,-1.01159967163841,-3.3431684547107));
#9499=CARTESIAN_POINT('Ctrl Pts',(3.02184423668056,-1.05976438929647,-3.33612255142302));
#9500=CARTESIAN_POINT('Ctrl Pts',(3.07943182754454,-1.08600460148177,-3.33149741801535));
#9501=CARTESIAN_POINT('Ctrl Pts',(3.19701596866615,-1.12854518700131,-3.32232037541134));
#9502=CARTESIAN_POINT('Ctrl Pts',(3.2567666069878,-1.14497823832997,-3.31778426873837));
#9503=CARTESIAN_POINT('Ctrl Pts',(3.32737802061638,-1.15852995725997,-3.31274229332292));
#9504=CARTESIAN_POINT('Ctrl Pts',(3.33724330873386,-1.16029307475342,-3.31204507588797));
#9505=CARTESIAN_POINT('Ctrl Pts',(3.35101636673719,-1.16257357457425,-3.31108278865973));
#9506=CARTESIAN_POINT('Ctrl Pts',(3.35490570985758,-1.16319752993834,-3.31081227988626));
#9507=CARTESIAN_POINT('Ctrl Pts',(3.3616214755311,-1.16424038692886,-3.31034739291194));
#9508=CARTESIAN_POINT('Ctrl Pts',(3.3644463961517,-1.16466853305111,-3.31015251403851));
#9509=CARTESIAN_POINT('Ctrl Pts',(3.37041048954383,-1.16555026355276,-3.30974253246608));
#9510=CARTESIAN_POINT('Ctrl Pts',(3.37354998763642,-1.1660014549157,-3.30952757021895));
#9511=CARTESIAN_POINT('Ctrl Pts',(3.38134684249088,-1.16708984723169,-3.30899574628352));
#9512=CARTESIAN_POINT('Ctrl Pts',(3.38600632683078,-1.16771186704414,-3.30867971650503));
#9513=CARTESIAN_POINT('Ctrl Pts',(3.40360735039072,-1.16995434831707,-3.30749226675355));
#9514=CARTESIAN_POINT('Ctrl Pts',(3.41657234475879,-1.17138777082818,-3.30663050537581));
#9515=CARTESIAN_POINT('Ctrl Pts',(3.44994668827043,-1.17451741672958,-3.30443914066392));
#9516=CARTESIAN_POINT('Ctrl Pts',(3.47038187695158,-1.17589732585908,-3.30312316525829));
#9517=CARTESIAN_POINT('Ctrl Pts',(3.54862425781716,-1.1791337709615,-3.29814819724476));
#9518=CARTESIAN_POINT('Ctrl Pts',(3.60650567346308,-1.17726502977485,-3.29459727124975));
#9519=CARTESIAN_POINT('Ctrl Pts',(3.73906491257438,-1.1631733033116,-3.28634308521419));
#9520=CARTESIAN_POINT('Ctrl Pts',(3.81316022767033,-1.14800217019918,-3.28162975201806));
#9521=CARTESIAN_POINT('Ctrl Pts',(3.89522057104641,-1.12279980931841,-3.27599581681253));
#9522=CARTESIAN_POINT('Ctrl Pts',(3.90511022897173,-1.11961871302437,-3.27531004044194));
#9523=CARTESIAN_POINT('Ctrl Pts',(3.92133036282158,-1.11416354680174,-3.27417339913102));
#9524=CARTESIAN_POINT('Ctrl Pts',(3.92768587238572,-1.11196528834139,-3.2737249934423));
#9525=CARTESIAN_POINT('Ctrl Pts',(3.93913662693685,-1.10789454342505,-3.2729114281665));
#9526=CARTESIAN_POINT('Ctrl Pts',(3.94423844982924,-1.10604101771551,-3.2725468981214));
#9527=CARTESIAN_POINT('Ctrl Pts',(3.95516102595931,-1.10198708357626,-3.27176196807344));
#9528=CARTESIAN_POINT('Ctrl Pts',(3.96097749592488,-1.09977568637731,-3.27134121487764));
#9529=CARTESIAN_POINT('Ctrl Pts',(3.97687033641353,-1.09358870298832,-3.27018380951579));
#9530=CARTESIAN_POINT('Ctrl Pts',(3.98690960173241,-1.08952011439486,-3.26944409900032));
#9531=CARTESIAN_POINT('Ctrl Pts',(4.02446599860444,-1.07369312990808,-3.26664355615269));
#9532=CARTESIAN_POINT('Ctrl Pts',(4.05157800284191,-1.06103007383657,-3.26455347747179));
#9533=CARTESIAN_POINT('Ctrl Pts',(4.07816931781854,-1.04735426286176,-3.26243320031815));
#9534=CARTESIAN_POINT('',(2.36176924975877,-0.000685226520117502,-3.32646548062114));
#9535=CARTESIAN_POINT('Ctrl Pts',(4.07816926753082,-1.04735428872454,-3.16389876579091));
#9536=CARTESIAN_POINT('Ctrl Pts',(4.07216381045497,-1.05044287182632,-3.16434541254173));
#9537=CARTESIAN_POINT('Ctrl Pts',(4.0661316377366,-1.05347988029879,-3.16478935096556));
#9538=CARTESIAN_POINT('Ctrl Pts',(4.04170150629564,-1.06551739402014,-3.16656977557909));
#9539=CARTESIAN_POINT('Ctrl Pts',(4.02309548108024,-1.07408960108841,-3.16788600383687));
#9540=CARTESIAN_POINT('Ctrl Pts',(3.95114101430919,-1.10499152359238,-3.17286095269525));
#9541=CARTESIAN_POINT('Ctrl Pts',(3.89639619841826,-1.12386761349931,-3.17641164228168));
#9542=CARTESIAN_POINT('Ctrl Pts',(3.76751947088795,-1.15793201295094,-3.1846656140504));
#9543=CARTESIAN_POINT('Ctrl Pts',(3.69288120625955,-1.17015750197088,-3.18937897703656));
#9544=CARTESIAN_POINT('Ctrl Pts',(3.60722745895398,-1.17584800632533,-3.19501288167123));
#9545=CARTESIAN_POINT('Ctrl Pts',(3.59685443481875,-1.17639942412098,-3.19569859243701));
#9546=CARTESIAN_POINT('Ctrl Pts',(3.57975700251857,-1.17708163819283,-3.19683511084415));
#9547=CARTESIAN_POINT('Ctrl Pts',(3.57303621558054,-1.17729217794565,-3.19728345960666));
#9548=CARTESIAN_POINT('Ctrl Pts',(3.56088824968675,-1.17756862858315,-3.19809691136177));
#9549=CARTESIAN_POINT('Ctrl Pts',(3.55546168038015,-1.17765459646126,-3.19846138491279));
#9550=CARTESIAN_POINT('Ctrl Pts',(3.5438134945486,-1.17775860337308,-3.19924618125349));
#9551=CARTESIAN_POINT('Ctrl Pts',(3.53759196465681,-1.17776485507355,-3.19966685704404));
#9552=CARTESIAN_POINT('Ctrl Pts',(3.52054132154316,-1.17764688725659,-3.2008240155209));
#9553=CARTESIAN_POINT('Ctrl Pts',(3.50971373881204,-1.17742259833855,-3.20156355503496));
#9554=CARTESIAN_POINT('Ctrl Pts',(3.44560902489901,-1.17520990930784,-3.2059712027159));
#9555=CARTESIAN_POINT('Ctrl Pts',(3.39252115708324,-1.16975534760865,-3.20974514440144));
#9556=CARTESIAN_POINT('Ctrl Pts',(3.25762230127863,-1.14656638231187,-3.21963791839877));
#9557=CARTESIAN_POINT('Ctrl Pts',(3.17699969890276,-1.12368098674895,-3.22585635791559));
#9558=CARTESIAN_POINT('Ctrl Pts',(3.07352000319832,-1.08199965306938,-3.23389516112285));
#9559=CARTESIAN_POINT('Ctrl Pts',(3.0479379212352,-1.07061974606113,-3.23588521397672));
#9560=CARTESIAN_POINT('Ctrl Pts',(3.01714297967116,-1.05558405785667,-3.23826446056107));
#9561=CARTESIAN_POINT('Ctrl Pts',(3.01152440666644,-1.05278493672653,-3.23869786683944));
#9562=CARTESIAN_POINT('Ctrl Pts',(3.0027605067172,-1.04833103321215,-3.23937250824708));
#9563=CARTESIAN_POINT('Ctrl Pts',(2.99959993404511,-1.04670675838434,-3.23961552229055));
#9564=CARTESIAN_POINT('Ctrl Pts',(2.99379147890894,-1.04368837987008,-3.24006153687712));
#9565=CARTESIAN_POINT('Ctrl Pts',(2.99114156514094,-1.04229849397095,-3.24026477985168));
#9566=CARTESIAN_POINT('Ctrl Pts',(2.9851167029621,-1.03910910259628,-3.24072636597063));
#9567=CARTESIAN_POINT('Ctrl Pts',(2.98174519955562,-1.03730324509577,-3.24098431053808));
#9568=CARTESIAN_POINT('Ctrl Pts',(2.97462662472816,-1.03344562462295,-3.24152830139936));
#9569=CARTESIAN_POINT('Ctrl Pts',(2.97088178778538,-1.03138982763521,-3.24181410286266));
#9570=CARTESIAN_POINT('Ctrl Pts',(2.96091433669886,-1.02584722273583,-3.24257403280044));
#9571=CARTESIAN_POINT('Ctrl Pts',(2.95471196568868,-1.02232412596306,-3.24304609818235));
#9572=CARTESIAN_POINT('Ctrl Pts',(2.93559406328807,-1.01123376733574,-3.24449986382827));
#9573=CARTESIAN_POINT('Ctrl Pts',(2.92279004256329,-1.00347620650165,-3.24547164622372));
#9574=CARTESIAN_POINT('Ctrl Pts',(2.87097312393294,-0.970715356158586,-3.24941137615357));
#9575=CARTESIAN_POINT('Ctrl Pts',(2.83330164012755,-0.943662859352533,-3.25229324189072));
#9576=CARTESIAN_POINT('Ctrl Pts',(2.72694049566269,-0.857337321892232,-3.26077696244841));
#9577=CARTESIAN_POINT('Ctrl Pts',(2.66339886031281,-0.792289386717381,-3.2663405929274));
#9578=CARTESIAN_POINT('Ctrl Pts',(2.5988142427707,-0.708796378478885,-3.27322579319779));
#9579=CARTESIAN_POINT('Ctrl Pts',(2.58990756260922,-0.696818362934043,-3.27420731383331));
#9580=CARTESIAN_POINT('Ctrl Pts',(2.57717627467303,-0.678999335343267,-3.27566028473674));
#9581=CARTESIAN_POINT('Ctrl Pts',(2.57317189606556,-0.673288117522481,-3.27612492073691));
#9582=CARTESIAN_POINT('Ctrl Pts',(2.56612069163644,-0.663038890473538,-3.27695705544193));
#9583=CARTESIAN_POINT('Ctrl Pts',(2.563054255402,-0.658514568962686,-3.27732380621339));
#9584=CARTESIAN_POINT('Ctrl Pts',(2.55668771755714,-0.648978918308727,-3.27809566859469));
#9585=CARTESIAN_POINT('Ctrl Pts',(2.55339420794947,-0.64396339805248,-3.27850101078419));
#9586=CARTESIAN_POINT('Ctrl Pts',(2.54481625845102,-0.630680341864174,-3.27957297180535));
#9587=CARTESIAN_POINT('Ctrl Pts',(2.53959665666902,-0.622371701106363,-3.28024193531335));
#9588=CARTESIAN_POINT('Ctrl Pts',(2.51519668230655,-0.58243208119117,-3.2834510873421));
#9589=CARTESIAN_POINT('Ctrl Pts',(2.49741168586041,-0.549977425545492,-3.28604039349646));
#9590=CARTESIAN_POINT('Ctrl Pts',(2.4403237665403,-0.433056350756097,-3.29531007800162));
#9591=CARTESIAN_POINT('Ctrl Pts',(2.40953591555949,-0.344822560384054,-3.30223383750231));
#9592=CARTESIAN_POINT('Ctrl Pts',(2.38405244258881,-0.229394596659508,-3.31081303448707));
#9593=CARTESIAN_POINT('Ctrl Pts',(2.37942619461876,-0.204718573781859,-3.31261802054143));
#9594=CARTESIAN_POINT('Ctrl Pts',(2.37343136057271,-0.165935454035137,-3.31539256510061));
#9595=CARTESIAN_POINT('Ctrl Pts',(2.37152275457443,-0.151920282863744,-3.31638258817523));
#9596=CARTESIAN_POINT('Ctrl Pts',(2.3692807833377,-0.132900467540097,-3.31770615523241));
#9597=CARTESIAN_POINT('Ctrl Pts',(2.36872630502981,-0.127923749240768,-3.31805063293189));
#9598=CARTESIAN_POINT('Ctrl Pts',(2.36789925913393,-0.120044264887885,-3.31859295730121));
#9599=CARTESIAN_POINT('Ctrl Pts',(2.36760570750693,-0.117143834827476,-3.318791927765));
#9600=CARTESIAN_POINT('Ctrl Pts',(2.36704181257365,-0.111357926906338,-3.31918749063668));
#9601=CARTESIAN_POINT('Ctrl Pts',(2.36677134744997,-0.108472515060543,-3.31938408141543));
#9602=CARTESIAN_POINT('Ctrl Pts',(2.36623498913183,-0.102513849152593,-3.31978871643012));
#9603=CARTESIAN_POINT('Ctrl Pts',(2.36597051258046,-0.099440472716324,-3.31999668348267));
#9604=CARTESIAN_POINT('Ctrl Pts',(2.36537601758768,-0.0921991383807463,
-3.32048502538132));
#9605=CARTESIAN_POINT('Ctrl Pts',(2.36505610945279,-0.0880303597128459,
-3.32076486606148));
#9606=CARTESIAN_POINT('Ctrl Pts',(2.36403603387288,-0.0737405169386048,
-3.32171995080133));
#9607=CARTESIAN_POINT('Ctrl Pts',(2.36344441969837,-0.0636118322215455,
-3.32238977303471));
#9608=CARTESIAN_POINT('Ctrl Pts',(2.36218445924856,-0.0358914046913295,
-3.32420652091499));
#9609=CARTESIAN_POINT('Ctrl Pts',(2.36177949234592,-0.0182899231070387,
-3.3253420215642));
#9610=CARTESIAN_POINT('Ctrl Pts',(2.36176924975877,-0.000685226520117502,
-3.32646548062114));
#9611=CARTESIAN_POINT('Ctrl Pts',(2.36176925070335,-0.000686848120440911,
-3.32646537713726));
#9612=CARTESIAN_POINT('Ctrl Pts',(2.36170726434664,0.105602180019166,-3.33324830865505));
#9613=CARTESIAN_POINT('Ctrl Pts',(2.37603299620722,0.211421176431465,-3.33959912714655));
#9614=CARTESIAN_POINT('Ctrl Pts',(2.41354804809705,0.347088586105826,-3.34854667360927));
#9615=CARTESIAN_POINT('Ctrl Pts',(2.42417784471382,0.379861592893897,-3.35076944568466));
#9616=CARTESIAN_POINT('Ctrl Pts',(2.43958484639731,0.421107908988138,-3.35367101025298));
#9617=CARTESIAN_POINT('Ctrl Pts',(2.44305192570047,0.430054600776447,-3.35430675582835));
#9618=CARTESIAN_POINT('Ctrl Pts',(2.44884654203039,0.444481696883111,-3.35534278585602));
#9619=CARTESIAN_POINT('Ctrl Pts',(2.45110705102283,0.449988685178161,-3.35574083974396));
#9620=CARTESIAN_POINT('Ctrl Pts',(2.45552818028636,0.460531082118157,-3.3565079645948));
#9621=CARTESIAN_POINT('Ctrl Pts',(2.45768238753637,0.465569025204975,-3.35687681263688));
#9622=CARTESIAN_POINT('Ctrl Pts',(2.46269720757444,0.477074195585782,-3.35772443494346));
#9623=CARTESIAN_POINT('Ctrl Pts',(2.4655810480382,0.483531004785404,-3.3582039823009));
#9624=CARTESIAN_POINT('Ctrl Pts',(2.47495167208151,0.504014056184857,-3.35973781742062));
#9625=CARTESIAN_POINT('Ctrl Pts',(2.48165621733334,0.517938277138569,-3.36079943799464));
#9626=CARTESIAN_POINT('Ctrl Pts',(2.52476112601509,0.603129462187264,-3.36741575042592));
#9627=CARTESIAN_POINT('Ctrl Pts',(2.56806658265669,0.670652369217492,-3.37321192652271));
#9628=CARTESIAN_POINT('Ctrl Pts',(2.64656377591275,0.76931775989478,-3.3824597156805));
#9629=CARTESIAN_POINT('Ctrl Pts',(2.67734899298471,0.803667839564259,-3.38585092263168));
#9630=CARTESIAN_POINT('Ctrl Pts',(2.72500878935058,0.850947092530639,-3.39070236240518));
#9631=CARTESIAN_POINT('Ctrl Pts',(2.74034426517797,0.86536563873708,-3.39220938888766));
#9632=CARTESIAN_POINT('Ctrl Pts',(2.7627972435383,0.885369836249182,-3.39433118696085));
#9633=CARTESIAN_POINT('Ctrl Pts',(2.76960473775599,0.891295952340837,-3.39496384952596));
#9634=CARTESIAN_POINT('Ctrl Pts',(2.78029962481323,0.900392176131148,-3.39594052828667));
#9635=CARTESIAN_POINT('Ctrl Pts',(2.78414012996974,0.903616564563787,-3.39628785884223));
#9636=CARTESIAN_POINT('Ctrl Pts',(2.79126113383715,0.909518047600413,-3.39692546873384));
#9637=CARTESIAN_POINT('Ctrl Pts',(2.79453568242073,0.912202154913365,-3.39721620712816));
#9638=CARTESIAN_POINT('Ctrl Pts',(2.80022265302385,0.916812646518107,-3.39771679463652));
#9639=CARTESIAN_POINT('Ctrl Pts',(2.80262829048344,0.918747299719223,-3.39792721768062));
#9640=CARTESIAN_POINT('Ctrl Pts',(2.80729077894539,0.922466855551421,-3.39833244482174));
#9641=CARTESIAN_POINT('Ctrl Pts',(2.80954659580869,0.924252972458334,-3.39852733901311));
#9642=CARTESIAN_POINT('Ctrl Pts',(2.81496816533031,0.92851344704474,-3.39899302334752));
#9643=CARTESIAN_POINT('Ctrl Pts',(2.81814010523731,0.930979927304475,-3.39926327017837));
#9644=CARTESIAN_POINT('Ctrl Pts',(2.82790120678969,0.938490257021382,-3.40008838864706));
#9645=CARTESIAN_POINT('Ctrl Pts',(2.83453126823213,0.943480871155306,-3.40063980073496));
#9646=CARTESIAN_POINT('Ctrl Pts',(2.90763503479563,0.997306983977838,-3.4066284380068));
#9647=CARTESIAN_POINT('Ctrl Pts',(2.97902060174175,1.03910742673274,-3.41166912353977));
#9648=CARTESIAN_POINT('Ctrl Pts',(3.10123846769282,1.09438135336674,-3.4199728001698));
#9649=CARTESIAN_POINT('Ctrl Pts',(3.14962369045581,1.11253828342649,-3.42318352732863));
#9650=CARTESIAN_POINT('Ctrl Pts',(3.21784750161664,1.13314095429153,-3.42773869212644));
#9651=CARTESIAN_POINT('Ctrl Pts',(3.23679244996208,1.13834860553179,-3.42900608058295));
#9652=CARTESIAN_POINT('Ctrl Pts',(3.27022835051705,1.14664589351153,-3.43125362133875));
#9653=CARTESIAN_POINT('Ctrl Pts',(3.28466411201686,1.14994052659722,-3.43222742007851));
#9654=CARTESIAN_POINT('Ctrl Pts',(3.30603801579209,1.15439640764161,-3.43367609065437));
#9655=CARTESIAN_POINT('Ctrl Pts',(3.31293096609522,1.15576913610115,-3.43414431497071));
#9656=CARTESIAN_POINT('Ctrl Pts',(3.32519731393573,1.158098026627,-3.43497957147724));
#9657=CARTESIAN_POINT('Ctrl Pts',(3.33056589324368,1.15907869551772,-3.43534582281302));
#9658=CARTESIAN_POINT('Ctrl Pts',(3.34188347381798,1.16106487403492,-3.43611945808568));
#9659=CARTESIAN_POINT('Ctrl Pts',(3.34783375762494,1.16206205042879,-3.43652709169396));
#9660=CARTESIAN_POINT('Ctrl Pts',(3.36363011478829,1.16458465337228,-3.43761173710072));
#9661=CARTESIAN_POINT('Ctrl Pts',(3.37348815336498,1.16603090147432,-3.43829119468062));
#9662=CARTESIAN_POINT('Ctrl Pts',(3.41761556187732,1.17193379821133,-3.44134485153878));
#9663=CARTESIAN_POINT('Ctrl Pts',(3.45204972888783,1.17500552514447,-3.44376126031426));
#9664=CARTESIAN_POINT('Ctrl Pts',(3.58652512176652,1.1810577911401,-3.45333293945063));
#9665=CARTESIAN_POINT('Ctrl Pts',(3.68664598253958,1.17279846589486,-3.46079293544927));
#9666=CARTESIAN_POINT('Ctrl Pts',(3.8055198273816,1.14751935047887,-3.46958092230525));
#9667=CARTESIAN_POINT('Ctrl Pts',(3.82641911900404,1.14247342892441,-3.4711211205662));
#9668=CARTESIAN_POINT('Ctrl Pts',(3.8602048948648,1.13333049433681,-3.47359165703966));
#9669=CARTESIAN_POINT('Ctrl Pts',(3.87317909609806,1.12957887422423,-3.47453563592933));
#9670=CARTESIAN_POINT('Ctrl Pts',(3.8906386238749,1.12420318145022,-3.47579695597588));
#9671=CARTESIAN_POINT('Ctrl Pts',(3.89518223264772,1.12277399810062,-3.4761243647073));
#9672=CARTESIAN_POINT('Ctrl Pts',(3.90274883539869,1.12034339618434,-3.4766680726243));
#9673=CARTESIAN_POINT('Ctrl Pts',(3.90577661956073,1.11935722441194,-3.47688522582315));
#9674=CARTESIAN_POINT('Ctrl Pts',(3.91150255241309,1.1174665249375,-3.47729506064139));
#9675=CARTESIAN_POINT('Ctrl Pts',(3.91420147754474,1.11656448060691,-3.4774878876229));
#9676=CARTESIAN_POINT('Ctrl Pts',(3.92058621018787,1.11440479566742,-3.47794328146209));
#9677=CARTESIAN_POINT('Ctrl Pts',(3.92426913014604,1.11313862841971,-3.47820535871792));
#9678=CARTESIAN_POINT('Ctrl Pts',(3.93715667858821,1.1086363581155,-3.47912052663344));
#9679=CARTESIAN_POINT('Ctrl Pts',(3.94632761619663,1.10530405944322,-3.47976834159575));
#9680=CARTESIAN_POINT('Ctrl Pts',(4.02239051631051,1.07659128237761,-3.4851209376526));
#9681=CARTESIAN_POINT('Ctrl Pts',(4.08689285267823,1.0452743320777,-3.48953402068664));
#9682=CARTESIAN_POINT('Ctrl Pts',(4.19831752385726,0.978014352344575,-3.49758451897788));
#9683=CARTESIAN_POINT('Ctrl Pts',(4.24614239186915,0.944039352222448,-3.50120603232571));
#9684=CARTESIAN_POINT('Ctrl Pts',(4.30752885282754,0.893142638380204,-3.50628920565357));
#9685=CARTESIAN_POINT('Ctrl Pts',(4.3234507657923,0.879200668164769,-3.50765123085441));
#9686=CARTESIAN_POINT('Ctrl Pts',(4.35050071100402,0.854195306666699,-3.51005100141468));
#9687=CARTESIAN_POINT('Ctrl Pts',(4.36179946879558,0.843324226921271,-3.51108109328746));
#9688=CARTESIAN_POINT('Ctrl Pts',(4.37795770085741,0.827144110758473,-3.51259753322676));
#9689=CARTESIAN_POINT('Ctrl Pts',(4.38299117517655,0.822010657738938,-3.51307628641409));
#9690=CARTESIAN_POINT('Ctrl Pts',(4.39177702375597,0.812884632511011,-3.51392346300255));
#9691=CARTESIAN_POINT('Ctrl Pts',(4.3955491619606,0.808911321032259,-3.51429102475715));
#9692=CARTESIAN_POINT('Ctrl Pts',(4.40336283157961,0.800565075090087,-3.51506054685705));
#9693=CARTESIAN_POINT('Ctrl Pts',(4.40739918751501,0.796187530104291,-3.51546271066298));
#9694=CARTESIAN_POINT('Ctrl Pts',(4.41785731088173,0.784671370521888,-3.51651707636438));
#9695=CARTESIAN_POINT('Ctrl Pts',(4.42422516864763,0.777484620048002,-3.51717148544111));
#9696=CARTESIAN_POINT('Ctrl Pts',(4.45084271923568,0.746693659173968,-3.51996092598244));
#9697=CARTESIAN_POINT('Ctrl Pts',(4.4702394930117,0.722372063160032,-3.52212970052603));
#9698=CARTESIAN_POINT('Ctrl Pts',(4.55013336105227,0.613626512228272,-3.53168765057077));
#9699=CARTESIAN_POINT('Ctrl Pts',(4.60027455324008,0.52217904213109,-3.53943164409005));
#9700=CARTESIAN_POINT('Ctrl Pts',(4.64562364763627,0.405093156114715,-3.54851395530527));
#9701=CARTESIAN_POINT('Ctrl Pts',(4.65291428079418,0.384602419888728,-3.55007251834525));
#9702=CARTESIAN_POINT('Ctrl Pts',(4.66384095467244,0.350971085714961,-3.55256903472033));
#9703=CARTESIAN_POINT('Ctrl Pts',(4.66782348788451,0.337949084417064,-3.55352096288756));
#9704=CARTESIAN_POINT('Ctrl Pts',(4.67289737548775,0.320267797861634,-3.55479109554313));
#9705=CARTESIAN_POINT('Ctrl Pts',(4.67418731869843,0.315667250467204,-3.55511954365551));
#9706=CARTESIAN_POINT('Ctrl Pts',(4.67629108917916,0.307984665029283,-3.55566450333985));
#9707=CARTESIAN_POINT('Ctrl Pts',(4.67712045267563,0.304906989583668,-3.5558818769536));
#9708=CARTESIAN_POINT('Ctrl Pts',(4.67866595069244,0.299077725075181,-3.55629176851676));
#9709=CARTESIAN_POINT('Ctrl Pts',(4.6793846314702,0.296326852665477,-3.55648443412707));
#9710=CARTESIAN_POINT('Ctrl Pts',(4.6810616094954,0.289811554436046,-3.55693900259209));
#9711=CARTESIAN_POINT('Ctrl Pts',(4.68201126613269,0.286044907946762,-3.55720042013527));
#9712=CARTESIAN_POINT('Ctrl Pts',(4.68529202025881,0.272755351458151,-3.5581181287895));
#9713=CARTESIAN_POINT('Ctrl Pts',(4.68752290779695,0.263207786684577,-3.55876907637804));
#9714=CARTESIAN_POINT('Ctrl Pts',(4.70493527424386,0.184250308769002,-3.56409204425701));
#9715=CARTESIAN_POINT('Ctrl Pts',(4.71392850734407,0.113615126710396,-3.56847656896941));
#9716=CARTESIAN_POINT('Ctrl Pts',(4.71862980099597,-0.0162999310916891,
-3.57651781406767));
#9717=CARTESIAN_POINT('Ctrl Pts',(4.71633782467676,-0.0752646307378745,
-3.58015950101522));
#9718=CARTESIAN_POINT('Ctrl Pts',(4.70723106756163,-0.154901470779693,-3.58526843745962));
#9719=CARTESIAN_POINT('Ctrl Pts',(4.70424912552254,-0.175924961958891,-3.58663486306575));
#9720=CARTESIAN_POINT('Ctrl Pts',(4.69807348634403,-0.212352899720643,-3.58904168435294));
#9721=CARTESIAN_POINT('Ctrl Pts',(4.69513632732219,-0.227795536579788,-3.59007436286857));
#9722=CARTESIAN_POINT('Ctrl Pts',(4.69040518364349,-0.250215833784624,-3.59159390961371));
#9723=CARTESIAN_POINT('Ctrl Pts',(4.68885477090343,-0.257243567266619,-3.59207313794342));
#9724=CARTESIAN_POINT('Ctrl Pts',(4.68601056251381,-0.269596555743125,-3.59292085723932));
#9725=CARTESIAN_POINT('Ctrl Pts',(4.68474381325762,-0.27492786513071,-3.59328848289595));
#9726=CARTESIAN_POINT('Ctrl Pts',(4.68202382649776,-0.286030269814525,-3.59405784293975));
#9727=CARTESIAN_POINT('Ctrl Pts',(4.68056396190131,-0.29179956537404,-3.59445977881113));
#9728=CARTESIAN_POINT('Ctrl Pts',(4.67663834910841,-0.306833294800882,-3.59551288213372));
#9729=CARTESIAN_POINT('Ctrl Pts',(4.67410313672481,-0.316078964705457,-3.59616624702305));
#9730=CARTESIAN_POINT('Ctrl Pts',(4.66290524382952,-0.355044833938312,-3.59894475683703));
#9731=CARTESIAN_POINT('Ctrl Pts',(4.65318613497871,-0.384445955186067,-3.6011033144089));
#9732=CARTESIAN_POINT('Ctrl Pts',(4.61315909462352,-0.491216437982374,-3.60917867050923));
#9733=CARTESIAN_POINT('Ctrl Pts',(4.57585118577394,-0.565693277627063,-3.61530191180339));
#9734=CARTESIAN_POINT('Ctrl Pts',(4.50288073557931,-0.679521450349702,-3.62519946191976));
#9735=CARTESIAN_POINT('Ctrl Pts',(4.47184481147958,-0.721515843933072,-3.62898326707604));
#9736=CARTESIAN_POINT('Ctrl Pts',(4.433626253769,-0.766626225089008,-3.63309545334704));
#9737=CARTESIAN_POINT('Ctrl Pts',(4.42908215366013,-0.771894391271796,-3.63357643603305));
#9738=CARTESIAN_POINT('Ctrl Pts',(4.42207594827429,-0.779872929591528,-3.63430561877818));
#9739=CARTESIAN_POINT('Ctrl Pts',(4.41964753900396,-0.782612489523834,-3.63455613127705));
#9740=CARTESIAN_POINT('Ctrl Pts',(4.41517824336473,-0.787607320299338,-3.63501304978695));
#9741=CARTESIAN_POINT('Ctrl Pts',(4.41314138754797,-0.789866017559552,-3.63521973166424));
#9742=CARTESIAN_POINT('Ctrl Pts',(4.40852305839145,-0.794947626180182,-3.63568487900524));
#9743=CARTESIAN_POINT('Ctrl Pts',(4.40593656766778,-0.797765868584669,-3.63594296643533));
#9744=CARTESIAN_POINT('Ctrl Pts',(4.39921561262334,-0.805017784434225,-3.6366075426417));
#9745=CARTESIAN_POINT('Ctrl Pts',(4.39506050377296,-0.80943229348126,-3.63701254791732));
#9746=CARTESIAN_POINT('Ctrl Pts',(4.36693300716531,-0.838857188146637,-3.63971679768988));
#9747=CARTESIAN_POINT('Ctrl Pts',(4.34189873955786,-0.86283403825283,-3.64194349424006));
#9748=CARTESIAN_POINT('Ctrl Pts',(4.29461691407231,-0.904278078606839,-3.64591638524916));
#9749=CARTESIAN_POINT('Ctrl Pts',(4.27273000453715,-0.922113574868906,-3.64767376245757));
#9750=CARTESIAN_POINT('Ctrl Pts',(4.21196687787682,-0.968096383986053,-3.65239835475215));
#9751=CARTESIAN_POINT('Ctrl Pts',(4.17197858776579,-0.994681622510907,-3.65534861435949));
#9752=CARTESIAN_POINT('Ctrl Pts',(4.11328239948327,-1.02873028431044,-3.65959207142446));
#9753=CARTESIAN_POINT('Ctrl Pts',(4.09583950175425,-1.03826655711673,-3.66084262547221));
#9754=CARTESIAN_POINT('Ctrl Pts',(4.07816923053759,-1.04735430775001,-3.66210420774532));
#9755=CARTESIAN_POINT('Origin',(3.53951905042299,8.32667268468867E-16,0.924367114736157));
#9756=CARTESIAN_POINT('',(4.07816926766421,-1.04735428865594,-4.2605248066102));
#9757=CARTESIAN_POINT('',(4.07816926526045,-1.04735428989218,-4.16229603312229));
#9758=CARTESIAN_POINT('',(4.07816926754759,-1.04735428871592,0.924367114736157));
#9759=CARTESIAN_POINT('',(2.36176953086107,0.00104804198854717,-3.92438851548543));
#9760=CARTESIAN_POINT('Ctrl Pts',(4.07816926766421,-1.04735428865594,-4.2605248066102));
#9761=CARTESIAN_POINT('Ctrl Pts',(4.08061053188268,-1.04609875600966,-4.2603336670524));
#9762=CARTESIAN_POINT('Ctrl Pts',(4.08304747073253,-1.04483465478307,-4.26014296728099));
#9763=CARTESIAN_POINT('Ctrl Pts',(4.09058011353672,-1.04089379733266,-4.25955387279466));
#9764=CARTESIAN_POINT('Ctrl Pts',(4.09566069109069,-1.03818816767703,-4.25915706029222));
#9765=CARTESIAN_POINT('Ctrl Pts',(4.10371247460442,-1.03382417148908,-4.25852925003506));
#9766=CARTESIAN_POINT('Ctrl Pts',(4.10669660193925,-1.03219003252469,-4.25829680768267));
#9767=CARTESIAN_POINT('Ctrl Pts',(4.11237478811221,-1.02904853904742,-4.25785502607278));
#9768=CARTESIAN_POINT('Ctrl Pts',(4.11506998269182,-1.02754353508609,-4.25764555868759));
#9769=CARTESIAN_POINT('Ctrl Pts',(4.12145446755203,-1.02394542027381,-4.25714984676672));
#9770=CARTESIAN_POINT('Ctrl Pts',(4.12513841664614,-1.02184294913762,-4.25686419382229));
#9771=CARTESIAN_POINT('Ctrl Pts',(4.1374993928772,-1.01469959644986,-4.25590673186276));
#9772=CARTESIAN_POINT('Ctrl Pts',(4.14612361904362,-1.00956756822577,-4.25524039136865));
#9773=CARTESIAN_POINT('Ctrl Pts',(4.16692687595816,-0.996825304375324,-4.25363450212652));
#9774=CARTESIAN_POINT('Ctrl Pts',(4.17903459791511,-0.989101193390206,-4.2527010839145));
#9775=CARTESIAN_POINT('Ctrl Pts',(4.22696655719119,-0.957274805137691,-4.24899812589751));
#9776=CARTESIAN_POINT('Ctrl Pts',(4.26159696136062,-0.931430723446777,-4.246304311219));
#9777=CARTESIAN_POINT('Ctrl Pts',(4.36809309949528,-0.842437036899015,-4.23769869052084));
#9778=CARTESIAN_POINT('Ctrl Pts',(4.43370864790271,-0.77243639778176,-4.23185193496188));
#9779=CARTESIAN_POINT('Ctrl Pts',(4.49867305956475,-0.683613570832528,-4.22466819902152));
#9780=CARTESIAN_POINT('Ctrl Pts',(4.50698906377458,-0.671792878114884,-4.22371727338928));
#9781=CARTESIAN_POINT('Ctrl Pts',(4.51898549233882,-0.654055822919525,-4.22229618232871));
#9782=CARTESIAN_POINT('Ctrl Pts',(4.52283453696928,-0.648254719046718,-4.22183229678599));
#9783=CARTESIAN_POINT('Ctrl Pts',(4.52960481301824,-0.637851825501089,-4.22100183696605));
#9784=CARTESIAN_POINT('Ctrl Pts',(4.53254598068112,-0.633263201731448,-4.22063601010524));
#9785=CARTESIAN_POINT('Ctrl Pts',(4.53869575680349,-0.623520513039784,-4.21986019915829));
#9786=CARTESIAN_POINT('Ctrl Pts',(4.54189656441925,-0.618361737018811,-4.2194499444115));
#9787=CARTESIAN_POINT('Ctrl Pts',(4.55033347188491,-0.604526234410318,-4.21835096284075));
#9788=CARTESIAN_POINT('Ctrl Pts',(4.55549760825921,-0.595806446434642,-4.21765967454887));
#9789=CARTESIAN_POINT('Ctrl Pts',(4.58109743404105,-0.551279658458068,-4.2141354960387));
#9790=CARTESIAN_POINT('Ctrl Pts',(4.59975315332767,-0.514487835870052,-4.21124090284159));
#9791=CARTESIAN_POINT('Ctrl Pts',(4.65758864327877,-0.383857388771443,-4.20102029895914));
#9792=CARTESIAN_POINT('Ctrl Pts',(4.68652801991301,-0.285994970160333,-4.19341781970315));
#9793=CARTESIAN_POINT('Ctrl Pts',(4.70631058953558,-0.162058183566401,-4.18441574865013));
#9794=CARTESIAN_POINT('Ctrl Pts',(4.70935693446314,-0.138364963283824,-4.1827247103124));
#9795=CARTESIAN_POINT('Ctrl Pts',(4.71226330031275,-0.108636171484832,-4.18065279521174));
#9796=CARTESIAN_POINT('Ctrl Pts',(4.71280030919271,-0.102674169125688,-4.18023978299348));
#9797=CARTESIAN_POINT('Ctrl Pts',(4.71357820507985,-0.0932326402845001,
-4.17958995557705));
#9798=CARTESIAN_POINT('Ctrl Pts',(4.71384912428019,-0.0897557924563585,
-4.17935156195845));
#9799=CARTESIAN_POINT('Ctrl Pts',(4.71430650257029,-0.0835290420166838,
-4.17892629997626));
#9800=CARTESIAN_POINT('Ctrl Pts',(4.71449875208627,-0.0807796971831158,
-4.17873912305569));
#9801=CARTESIAN_POINT('Ctrl Pts',(4.71493955105354,-0.0741410596285472,
-4.17828856083999));
#9802=CARTESIAN_POINT('Ctrl Pts',(4.71517844973885,-0.0702511773201224,
-4.17802570897476));
#9803=CARTESIAN_POINT('Ctrl Pts',(4.71585610857507,-0.0582432892694729,
-4.17721765704315));
#9804=CARTESIAN_POINT('Ctrl Pts',(4.71623013770644,-0.0501216641725522,
-4.17667586089719));
#9805=CARTESIAN_POINT('Ctrl Pts',(4.71690889531294,-0.0310987080354761,
-4.17541655246524));
#9806=CARTESIAN_POINT('Ctrl Pts',(4.71714638286752,-0.0201955690324883,
-4.17470223480156));
#9807=CARTESIAN_POINT('Ctrl Pts',(4.71745243816693,0.0186025334968413,-4.17218195649293));
#9808=CARTESIAN_POINT('Ctrl Pts',(4.71668149644096,0.0464963480844941,-4.1704095728507));
#9809=CARTESIAN_POINT('Ctrl Pts',(4.70965218591332,0.157640511496342,-4.16341498001619));
#9810=CARTESIAN_POINT('Ctrl Pts',(4.6955434647511,0.240146314751699,-4.15835744008072));
#9811=CARTESIAN_POINT('Ctrl Pts',(4.66184794563702,0.359307605937843,-4.15053677189155));
#9812=CARTESIAN_POINT('Ctrl Pts',(4.64887736267885,0.397552145251989,-4.14794645042967));
#9813=CARTESIAN_POINT('Ctrl Pts',(4.63010914142649,0.444766894451285,-4.14460448463226));
#9814=CARTESIAN_POINT('Ctrl Pts',(4.62611865738864,0.454428893920434,-4.14391283952734));
#9815=CARTESIAN_POINT('Ctrl Pts',(4.61958077249236,0.469680153178574,-4.14280810627163));
#9816=CARTESIAN_POINT('Ctrl Pts',(4.61711728888309,0.475304958764741,-4.1423978326367));
#9817=CARTESIAN_POINT('Ctrl Pts',(4.61261146766434,0.485377874547179,-4.14165787604038));
#9818=CARTESIAN_POINT('Ctrl Pts',(4.61058516105375,0.489833035289314,-4.14132874190786));
#9819=CARTESIAN_POINT('Ctrl Pts',(4.60576755941568,0.500252479086613,-4.14055454423502));
#9820=CARTESIAN_POINT('Ctrl Pts',(4.60295391815795,0.506206188033336,-4.14010872758931));
#9821=CARTESIAN_POINT('Ctrl Pts',(4.5946332940985,0.523437194382726,-4.13880825412039));
#9822=CARTESIAN_POINT('Ctrl Pts',(4.58899594478057,0.534650157361515,-4.1379491589722));
#9823=CARTESIAN_POINT('Ctrl Pts',(4.5758153398171,0.559855057269436,-4.13598807522075));
#9824=CARTESIAN_POINT('Ctrl Pts',(4.56816596785051,0.573788429698947,-4.13488257260118));
#9825=CARTESIAN_POINT('Ctrl Pts',(4.5417921325487,0.619605290264273,-4.13117457130428));
#9826=CARTESIAN_POINT('Ctrl Pts',(4.52185000024186,0.650759174847572,-4.1285326195553));
#9827=CARTESIAN_POINT('Ctrl Pts',(4.45689326441853,0.742430159928311,-4.12039866623981));
#9828=CARTESIAN_POINT('Ctrl Pts',(4.40750685952794,0.79960891318014,-4.11480499022491));
#9829=CARTESIAN_POINT('Ctrl Pts',(4.32905812099177,0.87453929033869,-4.10694970727554));
#9830=CARTESIAN_POINT('Ctrl Pts',(4.30416374763319,0.89638710557455,-4.10458452546581));
#9831=CARTESIAN_POINT('Ctrl Pts',(4.27371548301067,0.920916136791995,-4.10186754626579));
#9832=CARTESIAN_POINT('Ctrl Pts',(4.26902277500115,0.924637903284017,-4.10145351954349));
#9833=CARTESIAN_POINT('Ctrl Pts',(4.26130386123392,0.930664394469423,-4.10078043807841));
#9834=CARTESIAN_POINT('Ctrl Pts',(4.25829458963188,0.932990489505517,-4.10051997928127));
#9835=CARTESIAN_POINT('Ctrl Pts',(4.25285895846267,0.937150194238444,-4.10005308296787));
#9836=CARTESIAN_POINT('Ctrl Pts',(4.25043672856546,0.93898901297233,-4.09984629347443));
#9837=CARTESIAN_POINT('Ctrl Pts',(4.24506685150815,0.943032826812734,-4.09939065465233));
#9838=CARTESIAN_POINT('Ctrl Pts',(4.24211597575685,0.945233396309607,-4.09914210736358));
#9839=CARTESIAN_POINT('Ctrl Pts',(4.2334820615523,0.951609231768336,-4.09842006761506));
#9840=CARTESIAN_POINT('Ctrl Pts',(4.22777166141942,0.955747424930096,-4.09794901388681));
#9841=CARTESIAN_POINT('Ctrl Pts',(4.17440171399425,0.993696965989265,-4.09360291461117));
#9842=CARTESIAN_POINT('Ctrl Pts',(4.124317875001,1.02397359821846,-4.08993682324242));
#9843=CARTESIAN_POINT('Ctrl Pts',(3.98289042213369,1.09569211070334,-4.08009061752558));
#9844=CARTESIAN_POINT('Ctrl Pts',(3.88819542218631,1.12939903378864,-4.07398770888766));
#9845=CARTESIAN_POINT('Ctrl Pts',(3.776789809715,1.15368589955443,-4.06653731535964));
#9846=CARTESIAN_POINT('Ctrl Pts',(3.76314746784564,1.15640774488468,-4.06562140119996));
#9847=CARTESIAN_POINT('Ctrl Pts',(3.74271296501456,1.1601096155009,-4.06424268845803));
#9848=CARTESIAN_POINT('Ctrl Pts',(3.73595493440078,1.16127302003279,-4.06378562719153));
#9849=CARTESIAN_POINT('Ctrl Pts',(3.72381890119517,1.16325328882587,-4.06296269762399));
#9850=CARTESIAN_POINT('Ctrl Pts',(3.71844462952846,1.16409204292713,-4.06259752475349));
#9851=CARTESIAN_POINT('Ctrl Pts',(3.70699846376436,1.16579729199978,-4.06181809217536));
#9852=CARTESIAN_POINT('Ctrl Pts',(3.70092524502847,1.16665364089561,-4.06140352734916));
#9853=CARTESIAN_POINT('Ctrl Pts',(3.68451695183003,1.16883670494143,-4.06028062581848));
#9854=CARTESIAN_POINT('Ctrl Pts',(3.67417070814974,1.17007373836235,-4.05956952871269));
#9855=CARTESIAN_POINT('Ctrl Pts',(3.61847336120699,1.17598461349988,-4.05572402320733));
#9856=CARTESIAN_POINT('Ctrl Pts',(3.57290172212529,1.17815883924604,-4.05251340373268));
#9857=CARTESIAN_POINT('Ctrl Pts',(3.47384477911607,1.17713305972653,-4.04539803565048));
#9858=CARTESIAN_POINT('Ctrl Pts',(3.4204692722681,1.17293722866013,-4.04147650344936));
#9859=CARTESIAN_POINT('Ctrl Pts',(3.30773673850691,1.15630001922453,-4.03311378444394));
#9860=CARTESIAN_POINT('Ctrl Pts',(3.24866864476852,1.1428736919329,-4.02868339999732));
#9861=CARTESIAN_POINT('Ctrl Pts',(3.18132310991926,1.12200312644769,-4.0237393033503));
#9862=CARTESIAN_POINT('Ctrl Pts',(3.17179546633534,1.11891676626416,-4.02304254796327));
#9863=CARTESIAN_POINT('Ctrl Pts',(3.15857750680626,1.1144478946439,-4.02208079078059));
#9864=CARTESIAN_POINT('Ctrl Pts',(3.15485333033057,1.11316793630992,-4.02181035757952));
#9865=CARTESIAN_POINT('Ctrl Pts',(3.14843852575694,1.11092720164919,-4.02134556514466));
#9866=CARTESIAN_POINT('Ctrl Pts',(3.14574487404639,1.10997528017534,-4.02115070569896));
#9867=CARTESIAN_POINT('Ctrl Pts',(3.14006778549723,1.10794576182489,-4.02074072307446));
#9868=CARTESIAN_POINT('Ctrl Pts',(3.13708518946234,1.10686589620766,-4.02052574057102));
#9869=CARTESIAN_POINT('Ctrl Pts',(3.12987506350698,1.10422243353542,-4.02000695764937));
#9870=CARTESIAN_POINT('Ctrl Pts',(3.12565202410281,1.10264657298445,-4.01970386605013));
#9871=CARTESIAN_POINT('Ctrl Pts',(3.11012318943527,1.0967500818957,-4.01859180379022));
#9872=CARTESIAN_POINT('Ctrl Pts',(3.09887468398434,1.09227932231176,-4.01779108428916));
#9873=CARTESIAN_POINT('Ctrl Pts',(3.07047745353267,1.08048262726898,-4.01577707660513));
#9874=CARTESIAN_POINT('Ctrl Pts',(3.05342965181525,1.07292120034171,-4.01457497722258));
#9875=CARTESIAN_POINT('Ctrl Pts',(2.97629148858613,1.03649088568396,-4.00913638265606));
#9876=CARTESIAN_POINT('Ctrl Pts',(2.91853692779347,1.00295617033013,-4.00506060738765));
#9877=CARTESIAN_POINT('Ctrl Pts',(2.80701036876662,0.924853681040899,-3.99661694422729));
#9878=CARTESIAN_POINT('Ctrl Pts',(2.75374048136893,0.880041723597862,-3.99225762688552));
#9879=CARTESIAN_POINT('Ctrl Pts',(2.69736398445248,0.82339484354784,-3.98701313005524));
#9880=CARTESIAN_POINT('Ctrl Pts',(2.69009288619344,0.815891784284244,-3.98632349404621));
#9881=CARTESIAN_POINT('Ctrl Pts',(2.67829502354259,0.803388888367515,-3.98518177511804));
#9882=CARTESIAN_POINT('Ctrl Pts',(2.67370957558064,0.798445039140589,-3.98473219019675));
#9883=CARTESIAN_POINT('Ctrl Pts',(2.66550904555044,0.789449841766682,-3.98391736286575));
#9884=CARTESIAN_POINT('Ctrl Pts',(2.66187902113842,0.785412323938286,-3.98355275898036));
#9885=CARTESIAN_POINT('Ctrl Pts',(2.6541573973039,0.776703525461425,-3.98276864421313));
#9886=CARTESIAN_POINT('Ctrl Pts',(2.6500745810392,0.772024712435805,-3.98234878701259));
#9887=CARTESIAN_POINT('Ctrl Pts',(2.63959839958359,0.75982584105821,-3.98125759556522));
#9888=CARTESIAN_POINT('Ctrl Pts',(2.63326233934121,0.752257435910597,-3.98058397388087));
#9889=CARTESIAN_POINT('Ctrl Pts',(2.59972377305831,0.711156977530592,-3.9769428939996));
#9890=CARTESIAN_POINT('Ctrl Pts',(2.57428886130969,0.676231681490388,-3.97390713292723));
#9891=CARTESIAN_POINT('Ctrl Pts',(2.51893595613765,0.590720136221662,-3.96660612569285));
#9892=CARTESIAN_POINT('Ctrl Pts',(2.49077131701302,0.539135696131241,-3.96229869425451));
#9893=CARTESIAN_POINT('Ctrl Pts',(2.45498938701325,0.460086113927367,-3.95593211292864));
#9894=CARTESIAN_POINT('Ctrl Pts',(2.44432650274012,0.434093534690042,-3.95387480918752));
#9895=CARTESIAN_POINT('Ctrl Pts',(2.42242302430421,0.374738861009808,-3.94928575615794));
#9896=CARTESIAN_POINT('Ctrl Pts',(2.4117268983113,0.341200999528359,-3.94676744994914));
#9897=CARTESIAN_POINT('Ctrl Pts',(2.4009604870144,0.301357724900448,-3.94389859401908));
#9898=CARTESIAN_POINT('Ctrl Pts',(2.39941882629276,0.295471764326554,-3.94347789072222));
#9899=CARTESIAN_POINT('Ctrl Pts',(2.39698060395358,0.285859486389673,-3.94279618734842));
#9900=CARTESIAN_POINT('Ctrl Pts',(2.39605651733753,0.282140362398127,-3.94253372421479));
#9901=CARTESIAN_POINT('Ctrl Pts',(2.39443140962181,0.275460727757623,-3.94206473919431));
#9902=CARTESIAN_POINT('Ctrl Pts',(2.39372369319832,0.272501959004331,-3.94185785017745));
#9903=CARTESIAN_POINT('Ctrl Pts',(2.39219069751879,0.26598135243111,-3.94140377386248));
#9904=CARTESIAN_POINT('Ctrl Pts',(2.39137053436685,0.262418397229183,-3.94115687522502));
#9905=CARTESIAN_POINT('Ctrl Pts',(2.38970274045107,0.255015641548476,-3.94064630343271));
#9906=CARTESIAN_POINT('Ctrl Pts',(2.38885771991015,0.251175292656659,-3.94038277413045));
#9907=CARTESIAN_POINT('Ctrl Pts',(2.38671054185215,0.241178766979878,-3.9397001135755));
#9908=CARTESIAN_POINT('Ctrl Pts',(2.38543843811288,0.235016168386021,-3.93928252983237));
#9909=CARTESIAN_POINT('Ctrl Pts',(2.36935683554983,0.153829124494053,-3.93382045884806));
#9910=CARTESIAN_POINT('Ctrl Pts',(2.36183758556985,0.0775370159629636,-3.92912004385086));
#9911=CARTESIAN_POINT('Ctrl Pts',(2.36176951678359,0.00104809931671655,
-3.92438854089391));
#9912=CARTESIAN_POINT('Ctrl Pts',(2.36176951673139,0.00104804065385484,
-3.9243885372651));
#9913=CARTESIAN_POINT('Ctrl Pts',(2.36170039876251,-0.0766241902070196,
-3.91958383605501));
#9914=CARTESIAN_POINT('Ctrl Pts',(2.3693146407461,-0.154105831735525,-3.91476439767892));
#9915=CARTESIAN_POINT('Ctrl Pts',(2.38650654758807,-0.240338486056077,-3.90902709243526));
#9916=CARTESIAN_POINT('Ctrl Pts',(2.38864487921786,-0.250377816775807,-3.90835358176155));
#9917=CARTESIAN_POINT('Ctrl Pts',(2.39238328244189,-0.266868414827862,-3.90723738745212));
#9918=CARTESIAN_POINT('Ctrl Pts',(2.39390725830348,-0.273336495541825,-3.90679706293527));
#9919=CARTESIAN_POINT('Ctrl Pts',(2.39698832868437,-0.285934627436938,-3.90593430283839));
#9920=CARTESIAN_POINT('Ctrl Pts',(2.39854022868984,-0.292065723787995,-3.90551204336876));
#9921=CARTESIAN_POINT('Ctrl Pts',(2.40137619339858,-0.302902105357035,-3.90476136262689));
#9922=CARTESIAN_POINT('Ctrl Pts',(2.40264025681513,-0.307612509248537,-3.90443358675066));
#9923=CARTESIAN_POINT('Ctrl Pts',(2.40562100562091,-0.318450594679178,-3.9036759577904));
#9924=CARTESIAN_POINT('Ctrl Pts',(2.4073581581274,-0.324572439478732,-3.90324545733122));
#9925=CARTESIAN_POINT('Ctrl Pts',(2.4122829544837,-0.341407041688736,-3.90205439266956));
#9926=CARTESIAN_POINT('Ctrl Pts',(2.41557354704853,-0.352088731177394,-3.90129054517984));
#9927=CARTESIAN_POINT('Ctrl Pts',(2.43634133737977,-0.41624365759082,-3.89665232042659));
#9928=CARTESIAN_POINT('Ctrl Pts',(2.4574768928721,-0.468447343896776,-3.89265983053281));
#9929=CARTESIAN_POINT('Ctrl Pts',(2.50249411084264,-0.560163981593247,-3.8852571726978));
#9930=CARTESIAN_POINT('Ctrl Pts',(2.52512414925314,-0.600172528765996,-3.88188198609267));
#9931=CARTESIAN_POINT('Ctrl Pts',(2.57284611689614,-0.674097993457289,-3.87542768333664));
#9932=CARTESIAN_POINT('Ctrl Pts',(2.59753970553716,-0.708194906783507,-3.87235238995357));
#9933=CARTESIAN_POINT('Ctrl Pts',(2.63188899261136,-0.750639562423619,-3.86845176226482));
#9934=CARTESIAN_POINT('Ctrl Pts',(2.63992692770269,-0.760253979608165,-3.86756314440714));
#9935=CARTESIAN_POINT('Ctrl Pts',(2.65527860910518,-0.778032115592743,-3.86591309394098));
#9936=CARTESIAN_POINT('Ctrl Pts',(2.66255583779512,-0.786225588577091,-3.86514977972861));
#9937=CARTESIAN_POINT('Ctrl Pts',(2.6722640627135,-0.796853597043191,-3.86415720818341));
#9938=CARTESIAN_POINT('Ctrl Pts',(2.6745925738031,-0.799380422330187,-3.86392103715912));
#9939=CARTESIAN_POINT('Ctrl Pts',(2.67918713808672,-0.804322716273644,-3.86345880016781));
#9940=CARTESIAN_POINT('Ctrl Pts',(2.68145238734384,-0.806738888177693,-3.86323267942849));
#9941=CARTESIAN_POINT('Ctrl Pts',(2.68585148340174,-0.811391583793172,-3.86279702739081));
#9942=CARTESIAN_POINT('Ctrl Pts',(2.68798397528699,-0.813629297225322,-3.86258740518227));
#9943=CARTESIAN_POINT('Ctrl Pts',(2.6927227766992,-0.818562883000912,-3.86212496478452));
#9944=CARTESIAN_POINT('Ctrl Pts',(2.69533322523354,-0.821254781494435,-3.86187245860051));
#9945=CARTESIAN_POINT('Ctrl Pts',(2.70465371696756,-0.830774687812822,-3.86097860201256));
#9946=CARTESIAN_POINT('Ctrl Pts',(2.71143432135321,-0.837533523395143,-3.86034239227368));
#9947=CARTESIAN_POINT('Ctrl Pts',(2.77433497494493,-0.898721453754918,-3.85455920813305));
#9948=CARTESIAN_POINT('Ctrl Pts',(2.83567013750935,-0.947526894879376,-3.84976431458468));
#9949=CARTESIAN_POINT('Ctrl Pts',(2.9470042952222,-1.01929659580887,-3.84156873551229));
#9950=CARTESIAN_POINT('Ctrl Pts',(2.99458504989597,-1.04550733873365,-3.83820211639131));
#9951=CARTESIAN_POINT('Ctrl Pts',(3.06215856294847,-1.07686193613802,-3.83344580572473));
#9952=CARTESIAN_POINT('Ctrl Pts',(3.08073279744557,-1.08490541883781,-3.83214132927302));
#9953=CARTESIAN_POINT('Ctrl Pts',(3.11344332113403,-1.09808030328254,-3.82984201649596));
#9954=CARTESIAN_POINT('Ctrl Pts',(3.12748800353908,-1.10342705366624,-3.82885415929797));
#9955=CARTESIAN_POINT('Ctrl Pts',(3.14834887895483,-1.11091489742362,-3.82738407349395));
#9956=CARTESIAN_POINT('Ctrl Pts',(3.15508877454961,-1.11326518476249,-3.82690868594501));
#9957=CARTESIAN_POINT('Ctrl Pts',(3.16703280325044,-1.11730882220583,-3.82606529455302));
#9958=CARTESIAN_POINT('Ctrl Pts',(3.17222820212774,-1.11902745254394,-3.82569812615088));
#9959=CARTESIAN_POINT('Ctrl Pts',(3.18312552652671,-1.1225482069398,-3.82492725096427));
#9960=CARTESIAN_POINT('Ctrl Pts',(3.18882956372489,-1.1243432315911,-3.82452332607278));
#9961=CARTESIAN_POINT('Ctrl Pts',(3.20383649356018,-1.12894051128053,-3.82345939284191));
#9962=CARTESIAN_POINT('Ctrl Pts',(3.21316066174228,-1.13167117544022,-3.82279710355218));
#9963=CARTESIAN_POINT('Ctrl Pts',(3.25346538739096,-1.14293523677766,-3.81992824848856));
#9964=CARTESIAN_POINT('Ctrl Pts',(3.28475164447928,-1.15031338395358,-3.81768550808439));
#9965=CARTESIAN_POINT('Ctrl Pts',(3.42387585168212,-1.17716861087855,-3.80763731909785));
#9966=CARTESIAN_POINT('Ctrl Pts',(3.53380348514754,-1.18281891820952,-3.79943611846804));
#9967=CARTESIAN_POINT('Ctrl Pts',(3.66029971474918,-1.17167043377599,-3.79030886762797));
#9968=CARTESIAN_POINT('Ctrl Pts',(3.67764737986652,-1.16975219821265,-3.78906568128696));
#9969=CARTESIAN_POINT('Ctrl Pts',(3.70645186261257,-1.165917325074,-3.78702210444013));
#9970=CARTESIAN_POINT('Ctrl Pts',(3.71793410087469,-1.16421555900369,-3.78621298569804));
#9971=CARTESIAN_POINT('Ctrl Pts',(3.73382413508723,-1.16161989665838,-3.78510259201308));
#9972=CARTESIAN_POINT('Ctrl Pts',(3.73825434938933,-1.16087016192049,-3.7847940197792));
#9973=CARTESIAN_POINT('Ctrl Pts',(3.74576394291016,-1.15955504724416,-3.78427280188949));
#9974=CARTESIAN_POINT('Ctrl Pts',(3.74884552901996,-1.15900271333646,-3.78405944573402));
#9975=CARTESIAN_POINT('Ctrl Pts',(3.75517593532824,-1.15784199901858,-3.78362228530786));
#9976=CARTESIAN_POINT('Ctrl Pts',(3.75842444390212,-1.15723222219465,-3.7833985595264));
#9977=CARTESIAN_POINT('Ctrl Pts',(3.76689223287052,-1.1556058030122,-3.78281686364914));
#9978=CARTESIAN_POINT('Ctrl Pts',(3.77210734362133,-1.15456746211805,-3.78246008364174));
#9979=CARTESIAN_POINT('Ctrl Pts',(3.79348007828285,-1.1501614068025,-3.78100329897669));
#9980=CARTESIAN_POINT('Ctrl Pts',(3.80957395855438,-1.14648937147744,-3.77991897405437));
#9981=CARTESIAN_POINT('Ctrl Pts',(3.84436270214127,-1.13777856704782,-3.7775921483107));
#9982=CARTESIAN_POINT('Ctrl Pts',(3.86302134036225,-1.13261470280076,-3.77635501665119));
#9983=CARTESIAN_POINT('Ctrl Pts',(3.94934775508302,-1.10641588465514,-3.77064656442402));
#9984=CARTESIAN_POINT('Ctrl Pts',(4.01515567697647,-1.0797619320866,-3.76633114629972));
#9985=CARTESIAN_POINT('Ctrl Pts',(4.07816926790565,-1.04735428853177,-3.76191690485895));
#9986=CARTESIAN_POINT('Ctrl Pts',(4.07816923053759,-1.04735430775001,-3.66210420774532));
#9987=CARTESIAN_POINT('Ctrl Pts',(4.04844861985459,-1.06263950033389,-3.66422613304709));
#9988=CARTESIAN_POINT('Ctrl Pts',(4.01808480614548,-1.07665583766756,-3.66637966969037));
#9989=CARTESIAN_POINT('Ctrl Pts',(3.9771413196992,-1.09348027249041,-3.66928898261599));
#9990=CARTESIAN_POINT('Ctrl Pts',(3.9670678205978,-1.09745815102189,-3.67000513538608));
#9991=CARTESIAN_POINT('Ctrl Pts',(3.95112338361915,-1.10350153802698,-3.67113993062783));
#9992=CARTESIAN_POINT('Ctrl Pts',(3.94528831817094,-1.10566046794659,-3.67155548449973));
#9993=CARTESIAN_POINT('Ctrl Pts',(3.93433172578966,-1.10961591054872,-3.67233639632326));
#9994=CARTESIAN_POINT('Ctrl Pts',(3.9292143348106,-1.11142345719827,-3.67270138043947));
#9995=CARTESIAN_POINT('Ctrl Pts',(3.91772933681739,-1.11539107618947,-3.67352116899733));
#9996=CARTESIAN_POINT('Ctrl Pts',(3.91135539921351,-1.11753210247141,-3.67397658113456));
#9997=CARTESIAN_POINT('Ctrl Pts',(3.89508930371856,-1.12284137196217,-3.67514007839558));
#9998=CARTESIAN_POINT('Ctrl Pts',(3.88517309685208,-1.1259334881902,-3.67585059333827));
#9999=CARTESIAN_POINT('Ctrl Pts',(3.80299939013408,-1.15036943320402,-3.68174998840933));
#10000=CARTESIAN_POINT('Ctrl Pts',(3.72890066998285,-1.16486156269254,-3.68715976191397));
#10001=CARTESIAN_POINT('Ctrl Pts',(3.59597400316395,-1.17783693902623,-3.69692943800183));
#10002=CARTESIAN_POINT('Ctrl Pts',(3.53766849725277,-1.17918779262541,-3.70123136369423));
#10003=CARTESIAN_POINT('Ctrl Pts',(3.45922160018935,-1.17518497517152,-3.7069020253475));
#10004=CARTESIAN_POINT('Ctrl Pts',(3.43897064712184,-1.17362580168143,-3.70835474100237));
#10005=CARTESIAN_POINT('Ctrl Pts',(3.40587383062965,-1.17021454018066,-3.71070087284032));
#10006=CARTESIAN_POINT('Ctrl Pts',(3.39300078898572,-1.16867255833062,-3.71160638532605));
#10007=CARTESIAN_POINT('Ctrl Pts',(3.37550898727766,-1.16628373541297,-3.71282493220717));
#10008=CARTESIAN_POINT('Ctrl Pts',(3.37086651807613,-1.16562145549307,-3.71314720226167));
#10009=CARTESIAN_POINT('Ctrl Pts',(3.3630935162249,-1.16446517164721,-3.71368473403851));
#10010=CARTESIAN_POINT('Ctrl Pts',(3.35996083661272,-1.16398623434157,-3.71390081027675));
#10011=CARTESIAN_POINT('Ctrl Pts',(3.35400605052876,-1.16305122890294,-3.71431042739958));
#10012=CARTESIAN_POINT('Ctrl Pts',(3.35118362085546,-1.16259752304727,-3.71450410202761));
#10013=CARTESIAN_POINT('Ctrl Pts',(3.3444692137112,-1.16149308829024,-3.71496377401127));
#10014=CARTESIAN_POINT('Ctrl Pts',(3.3405787684138,-1.16083306218068,-3.71522925949236));
#10015=CARTESIAN_POINT('Ctrl Pts',(3.32677780327535,-1.15842026594744,-3.71616823560734));
#10016=CARTESIAN_POINT('Ctrl Pts',(3.31688617931598,-1.15655997338567,-3.7168360851204));
#10017=CARTESIAN_POINT('Ctrl Pts',(3.24861442522589,-1.14281188569118,-3.72141750979336));
#10018=CARTESIAN_POINT('Ctrl Pts',(3.19117834922134,-1.1266344066395,-3.72513186763262));
#10019=CARTESIAN_POINT('Ctrl Pts',(3.072179346441,-1.08313983084812,-3.73298225008632));
#10020=CARTESIAN_POINT('Ctrl Pts',(3.01123910751551,-1.054759687974,-3.73710183304628));
#10021=CARTESIAN_POINT('Ctrl Pts',(2.92322398438618,-1.00422021555506,-3.74355374607896));
#10022=CARTESIAN_POINT('Ctrl Pts',(2.89416644473011,-0.985797908113418,
-3.74577348102382));
#10023=CARTESIAN_POINT('Ctrl Pts',(2.85809108232158,-0.960647159867072,
-3.74867159772587));
#10024=CARTESIAN_POINT('Ctrl Pts',(2.85029123492305,-0.955066516465092,
-3.74930706235956));
#10025=CARTESIAN_POINT('Ctrl Pts',(2.83776269167216,-0.945869177634443,
-3.75034274759836));
#10026=CARTESIAN_POINT('Ctrl Pts',(2.8329916314314,-0.9423107195927,-3.75074074043638));
#10027=CARTESIAN_POINT('Ctrl Pts',(2.82388043338371,-0.935407107718452,
-3.75150782500438));
#10028=CARTESIAN_POINT('Ctrl Pts',(2.81953625700718,-0.932067520522219,
-3.75187669438017));
#10029=CARTESIAN_POINT('Ctrl Pts',(2.80963785389392,-0.92434762760609,-3.75272447564166));
#10030=CARTESIAN_POINT('Ctrl Pts',(2.8040995142685,-0.919947389676309,-3.75320416160331));
#10031=CARTESIAN_POINT('Ctrl Pts',(2.78658021839377,-0.905768916688391,
-3.75473889947827));
#10032=CARTESIAN_POINT('Ctrl Pts',(2.77475248973425,-0.895804824435225,
-3.75580129639469));
#10033=CARTESIAN_POINT('Ctrl Pts',(2.70327046541717,-0.833138235252452,
-3.76238907377542));
#10034=CARTESIAN_POINT('Ctrl Pts',(2.64890026058588,-0.774741861973427,
-3.76815310433015));
#10035=CARTESIAN_POINT('Ctrl Pts',(2.57282732747799,-0.674354202017694,
-3.77739103106325));
#10036=CARTESIAN_POINT('Ctrl Pts',(2.54702083012893,-0.635762553685175,
-3.78080459783862));
#10037=CARTESIAN_POINT('Ctrl Pts',(2.51287734126004,-0.577535816048185,
-3.78568297920743));
#10038=CARTESIAN_POINT('Ctrl Pts',(2.50268866524345,-0.559038171718371,
-3.7871950688076));
#10039=CARTESIAN_POINT('Ctrl Pts',(2.48688643539726,-0.52842916307065,-3.78962575089257));
#10040=CARTESIAN_POINT('Ctrl Pts',(2.48097187246806,-0.516479149832285,
-3.79055747924329));
#10041=CARTESIAN_POINT('Ctrl Pts',(2.47323115548551,-0.500147631308321,
-3.79180520057095));
#10042=CARTESIAN_POINT('Ctrl Pts',(2.47122693711902,-0.495852287053195,
-3.79213099258052));
#10043=CARTESIAN_POINT('Ctrl Pts',(2.46792169721483,-0.488655588196798,
-3.79267275505615));
#10044=CARTESIAN_POINT('Ctrl Pts',(2.46660641339628,-0.485760893170416,
-3.79288956707426));
#10045=CARTESIAN_POINT('Ctrl Pts',(2.46413455682944,-0.480261776050492,
-3.79329932190493));
#10046=CARTESIAN_POINT('Ctrl Pts',(2.4629756907694,-0.477658432169053,-3.79349240647044));
#10047=CARTESIAN_POINT('Ctrl Pts',(2.46024906773894,-0.471472858947253,
-3.79394911020788));
#10048=CARTESIAN_POINT('Ctrl Pts',(2.45868966710349,-0.467886949467087,
-3.79421223296509));
#10049=CARTESIAN_POINT('Ctrl Pts',(2.45326485745182,-0.455240511269034,
-3.79513466435501));
#10050=CARTESIAN_POINT('Ctrl Pts',(2.44949515812842,-0.446139019402175,
-3.79578858715235));
#10051=CARTESIAN_POINT('Ctrl Pts',(2.42015070718981,-0.372697193087162,
-3.80099414988089));
#10052=CARTESIAN_POINT('Ctrl Pts',(2.40017724275753,-0.30625409905891,-3.80527350177618));
#10053=CARTESIAN_POINT('Ctrl Pts',(2.36996520026676,-0.160110655326258,
-3.81450523120774));
#10054=CARTESIAN_POINT('Ctrl Pts',(2.36179525311326,-0.0803519521974262,
-3.81944418741669));
#10055=CARTESIAN_POINT('Ctrl Pts',(2.36176366402195,0.0162853768794864,
-3.82572603094372));
#10056=CARTESIAN_POINT('Ctrl Pts',(2.36211215340961,0.0329532537253749,
-3.82681939802594));
#10057=CARTESIAN_POINT('Ctrl Pts',(2.36310117832572,0.0564132401608757,
-3.8283747806013));
#10058=CARTESIAN_POINT('Ctrl Pts',(2.3634471299522,0.063216280260236,-3.82882776666044));
#10059=CARTESIAN_POINT('Ctrl Pts',(2.36415372310044,0.0750810022526736,
-3.82962136498457));
#10060=CARTESIAN_POINT('Ctrl Pts',(2.36448810225051,0.0801441141953606,
-3.82996116002476));
#10061=CARTESIAN_POINT('Ctrl Pts',(2.36525846034585,0.0907645415065579,
-3.83067638137945));
#10062=CARTESIAN_POINT('Ctrl Pts',(2.36570119609865,0.0963212252669191,
-3.8310520083426));
#10063=CARTESIAN_POINT('Ctrl Pts',(2.36685535434355,0.109614202312183,-3.83195409902611));
#10064=CARTESIAN_POINT('Ctrl Pts',(2.3676039034977,0.117346925179376,-3.83248169915888));
#10065=CARTESIAN_POINT('Ctrl Pts',(2.37045749641022,0.144066154517063,-3.83431489834426));
#10066=CARTESIAN_POINT('Ctrl Pts',(2.3729478252546,0.16300759709244,-3.83563230288415));
#10067=CARTESIAN_POINT('Ctrl Pts',(2.38014251869302,0.209037603783719,-3.83887928813729));
#10068=CARTESIAN_POINT('Ctrl Pts',(2.38533668375326,0.236037128911488,-3.84082281696858));
#10069=CARTESIAN_POINT('Ctrl Pts',(2.41473604672644,0.36445509295537,-3.85025063472687));
#10070=CARTESIAN_POINT('Ctrl Pts',(2.45138854482873,0.462528755992019,-3.85805991057015));
#10071=CARTESIAN_POINT('Ctrl Pts',(2.51050737087764,0.573310564704789,-3.86703725347443));
#10072=CARTESIAN_POINT('Ctrl Pts',(2.52105993057718,0.591854035582738,-3.86854355169125));
#10073=CARTESIAN_POINT('Ctrl Pts',(2.53513277427362,0.61509128959281,-3.87042653631821));
#10074=CARTESIAN_POINT('Ctrl Pts',(2.53819150074025,0.620058245661271,-3.87082874587661));
#10075=CARTESIAN_POINT('Ctrl Pts',(2.54310139283704,0.627900153576863,-3.8714630698678));
#10076=CARTESIAN_POINT('Ctrl Pts',(2.54492834297265,0.630790041628274,-3.87169667964179));
#10077=CARTESIAN_POINT('Ctrl Pts',(2.54842546247159,0.636268853358129,-3.87213922288277));
#10078=CARTESIAN_POINT('Ctrl Pts',(2.5500931929083,0.638859160167936,-3.87234829483588));
#10079=CARTESIAN_POINT('Ctrl Pts',(2.55406060805322,0.644968520217937,-3.87284108596375));
#10080=CARTESIAN_POINT('Ctrl Pts',(2.55636899742934,0.648481848907288,-3.87312423286438));
#10081=CARTESIAN_POINT('Ctrl Pts',(2.56412947459199,0.660156471728367,-3.87406456868759));
#10082=CARTESIAN_POINT('Ctrl Pts',(2.56966493571705,0.668262226576556,-3.87471655080822));
#10083=CARTESIAN_POINT('Ctrl Pts',(2.58330905339852,0.687715037914072,-3.87628151526722));
#10084=CARTESIAN_POINT('Ctrl Pts',(2.59151932480689,0.698989333478457,-3.87718876918013));
#10085=CARTESIAN_POINT('Ctrl Pts',(2.62472078783833,0.742919907260766,-3.88073637672632));
#10086=CARTESIAN_POINT('Ctrl Pts',(2.65121623596041,0.774405887494549,-3.88330745514829));
#10087=CARTESIAN_POINT('Ctrl Pts',(2.746945496837,0.876771730365237,-3.89200681350264));
#10088=CARTESIAN_POINT('Ctrl Pts',(2.82342800962459,0.940272890584698,-3.89804785574503));
#10089=CARTESIAN_POINT('Ctrl Pts',(2.918802157243,1.00100099562416,-3.90543403210144));
#10090=CARTESIAN_POINT('Ctrl Pts',(2.93078694217764,1.00833409532424,-3.90635893675167));
#10091=CARTESIAN_POINT('Ctrl Pts',(2.94883483682975,1.01893798109636,-3.90774850056985));
#10092=CARTESIAN_POINT('Ctrl Pts',(2.95480038857649,1.0223729909505,-3.90820728502022));
#10093=CARTESIAN_POINT('Ctrl Pts',(2.96553460067299,1.0284291520166,-3.9090320542742));
#10094=CARTESIAN_POINT('Ctrl Pts',(2.97029199832814,1.03106994463999,-3.90939733020954));
#10095=CARTESIAN_POINT('Ctrl Pts',(2.98043470030214,1.03660848400049,-3.91017563074714));
#10096=CARTESIAN_POINT('Ctrl Pts',(2.98582459984016,1.03949743271071,-3.91058895103993));
#10097=CARTESIAN_POINT('Ctrl Pts',(3.00038775807169,1.04715778414305,-3.91170512191986));
#10098=CARTESIAN_POINT('Ctrl Pts',(3.00960157928965,1.05185048236449,-3.9124106769385));
#10099=CARTESIAN_POINT('Ctrl Pts',(3.0586297217767,1.07601335970198,-3.91616278125679));
#10100=CARTESIAN_POINT('Ctrl Pts',(3.09945292736343,1.09334360389462,-3.91928115218655));
#10101=CARTESIAN_POINT('Ctrl Pts',(3.19234256433788,1.12673096456194,-3.92636308364059));
#10102=CARTESIAN_POINT('Ctrl Pts',(3.24474379307409,1.14156073096066,-3.93035049972805));
#10103=CARTESIAN_POINT('Ctrl Pts',(3.35768298020661,1.16522612653446,-3.93881898603055));
#10104=CARTESIAN_POINT('Ctrl Pts',(3.41827597922547,1.17308050887551,-3.94328910720124));
#10105=CARTESIAN_POINT('Ctrl Pts',(3.48919871205546,1.17671702860564,-3.94826886702782));
#10106=CARTESIAN_POINT('Ctrl Pts',(3.49919409521934,1.17710195665604,-3.94896475364315));
#10107=CARTESIAN_POINT('Ctrl Pts',(3.51312777543832,1.17746084917022,-3.94992548963286));
#10108=CARTESIAN_POINT('Ctrl Pts',(3.5170625328425,1.17754246490458,-3.95019575639631));
#10109=CARTESIAN_POINT('Ctrl Pts',(3.52385330335688,1.17764927010658,-3.95066032095821));
#10110=CARTESIAN_POINT('Ctrl Pts',(3.52670910415554,1.177683796583,-3.95085511806132));
#10111=CARTESIAN_POINT('Ctrl Pts',(3.53273693236199,1.17773474389974,-3.95126503668306));
#10112=CARTESIAN_POINT('Ctrl Pts',(3.5359089525109,1.17774873880127,-3.9514800172152));
#10113=CARTESIAN_POINT('Ctrl Pts',(3.54378482283516,1.17775166796254,-3.95201206725485));
#10114=CARTESIAN_POINT('Ctrl Pts',(3.54848868684836,1.17772523777653,-3.95232830297985));
#10115=CARTESIAN_POINT('Ctrl Pts',(3.56625975665319,1.17751890722221,-3.95351767410306));
#10116=CARTESIAN_POINT('Ctrl Pts',(3.57932438955163,1.17714969826929,-3.95438110964296));
#10117=CARTESIAN_POINT('Ctrl Pts',(3.61289435699904,1.17564143396813,-3.95657778478632));
#10118=CARTESIAN_POINT('Ctrl Pts',(3.63338151890948,1.1741833988167,-3.95789731202981));
#10119=CARTESIAN_POINT('Ctrl Pts',(3.71131820664477,1.16658366532871,-3.96287157829586));
#10120=CARTESIAN_POINT('Ctrl Pts',(3.76832811670062,1.15675390984114,-3.96641880997522));
#10121=CARTESIAN_POINT('Ctrl Pts',(3.89759001960959,1.12453171523331,-3.97466756075121));
#10122=CARTESIAN_POINT('Ctrl Pts',(3.9688580014888,1.09929625483355,-3.97937923449006));
#10123=CARTESIAN_POINT('Ctrl Pts',(4.04663302212342,1.06303263432097,-3.98501124989341));
#10124=CARTESIAN_POINT('Ctrl Pts',(4.05598868487624,1.05851880825231,-3.98569695866126));
#10125=CARTESIAN_POINT('Ctrl Pts',(4.07130005923392,1.05088021881746,-3.98683347443966));
#10126=CARTESIAN_POINT('Ctrl Pts',(4.07729101248484,1.04782707986891,-3.98728182259133));
#10127=CARTESIAN_POINT('Ctrl Pts',(4.08806964381035,1.04221723464326,-3.98809527369389));
#10128=CARTESIAN_POINT('Ctrl Pts',(4.09286644973831,1.03967839819818,-3.98845974720784));
#10129=CARTESIAN_POINT('Ctrl Pts',(4.10312405748324,1.03415819204342,-3.98924454397651));
#10130=CARTESIAN_POINT('Ctrl Pts',(4.10857910494799,1.0311665345298,-3.9896652202357));
#10131=CARTESIAN_POINT('Ctrl Pts',(4.12346407029455,1.02284923605826,-3.99082238133443));
#10132=CARTESIAN_POINT('Ctrl Pts',(4.13284443960847,1.01743663925843,-3.99156192302487));
#10133=CARTESIAN_POINT('Ctrl Pts',(4.18795513940158,0.984615729432178,-3.99596961974173));
#10134=CARTESIAN_POINT('Ctrl Pts',(4.2318497925435,0.954261059497406,-3.99974361111364));
#10135=CARTESIAN_POINT('Ctrl Pts',(4.31105842730863,0.89113667168131,-4.0070639731912));
#10136=CARTESIAN_POINT('Ctrl Pts',(4.34671963136999,0.858967033756197,-4.01058800950391));
#10137=CARTESIAN_POINT('Ctrl Pts',(4.40008695209897,0.804558893169404,-4.01617962053957));
#10138=CARTESIAN_POINT('Ctrl Pts',(4.41912598661287,0.783698831287555,-4.0182473517035));
#10139=CARTESIAN_POINT('Ctrl Pts',(4.45981447821357,0.735765800171875,-4.02280590525872));
#10140=CARTESIAN_POINT('Ctrl Pts',(4.48105793276918,0.708378440831675,-4.02528430910809));
#10141=CARTESIAN_POINT('Ctrl Pts',(4.5045653934219,0.675142478559903,-4.02811381200472));
#10142=CARTESIAN_POINT('Ctrl Pts',(4.50802773161558,0.670166209841275,-4.02853295335212));
#10143=CARTESIAN_POINT('Ctrl Pts',(4.51361190163298,0.662006654884104,-4.02921261948849));
#10144=CARTESIAN_POINT('Ctrl Pts',(4.51575686841944,0.658839447545405,-4.02947459359533));
#10145=CARTESIAN_POINT('Ctrl Pts',(4.51957961162135,0.653135215262649,-4.02994303597782));
#10146=CARTESIAN_POINT('Ctrl Pts',(4.52126302077772,0.65060209832433,-4.03014986789553));
#10147=CARTESIAN_POINT('Ctrl Pts',(4.52495107670906,0.645005570601507,-4.03060420868494));
#10148=CARTESIAN_POINT('Ctrl Pts',(4.52695126317326,0.64193932008488,-4.03085142607382));
#10149=CARTESIAN_POINT('Ctrl Pts',(4.53271095042371,0.633019203839182,-4.03156582615065));
#10150=CARTESIAN_POINT('Ctrl Pts',(4.5364329998611,0.627141168991839,-4.03203064783547));
#10151=CARTESIAN_POINT('Ctrl Pts',(4.56761767406544,0.576913614461229,-4.03595541886596));
#10152=CARTESIAN_POINT('Ctrl Pts',(4.5921617246552,0.53081160626499,-4.03924908255017));
#10153=CARTESIAN_POINT('Ctrl Pts',(4.64766320971026,0.407450785301738,-4.04767541787365));
#10154=CARTESIAN_POINT('Ctrl Pts',(4.67363991946275,0.3282820287332,-4.0527318918661));
#10155=CARTESIAN_POINT('Ctrl Pts',(4.69755572356987,0.216800752261754,-4.0600032591527));
#10156=CARTESIAN_POINT('Ctrl Pts',(4.70284865187255,0.186320911727268,-4.06200379042932));
#10157=CARTESIAN_POINT('Ctrl Pts',(4.70820254723277,0.146170427590695,-4.06467318821915));
#10158=CARTESIAN_POINT('Ctrl Pts',(4.7093532485695,0.136655953194657,-4.06530820480776));
#10159=CARTESIAN_POINT('Ctrl Pts',(4.71102998547545,0.121213033422497,-4.06634334019044));
#10160=CARTESIAN_POINT('Ctrl Pts',(4.71162743772298,0.115292656495342,-4.06674123567543));
#10161=CARTESIAN_POINT('Ctrl Pts',(4.71268887130824,0.103911808323198,-4.0675082561521));
#10162=CARTESIAN_POINT('Ctrl Pts',(4.71315965632523,0.0984521151681194,
-4.06787715969394));
#10163=CARTESIAN_POINT('Ctrl Pts',(4.71416065330249,0.0858136464931614,
-4.06873339917269));
#10164=CARTESIAN_POINT('Ctrl Pts',(4.71466318223655,0.0786329614264221,
-4.06922157859461));
#10165=CARTESIAN_POINT('Ctrl Pts',(4.71605392715649,0.0557502054716263,
-4.07078291415765));
#10166=CARTESIAN_POINT('Ctrl Pts',(4.7166934359112,0.0400353133819916,-4.07186366221968));
#10167=CARTESIAN_POINT('Ctrl Pts',(4.71745666545541,0.00307141003010868,
-4.07442690568669));
#10168=CARTESIAN_POINT('Ctrl Pts',(4.71732037574729,-0.0181769021506357,
-4.07591682543126));
#10169=CARTESIAN_POINT('Ctrl Pts',(4.71463514345411,-0.0983813380987575,
-4.08160331385886));
#10170=CARTESIAN_POINT('Ctrl Pts',(4.70823197613073,-0.157115915930673,
-4.08590110161006));
#10171=CARTESIAN_POINT('Ctrl Pts',(4.6844977053795,-0.284873298397203,-4.09543305152185));
#10172=CARTESIAN_POINT('Ctrl Pts',(4.66526075372894,-0.353321853443469,
-4.10066342150063));
#10173=CARTESIAN_POINT('Ctrl Pts',(4.63649494189315,-0.428759229392006,
-4.10632182334878));
#10174=CARTESIAN_POINT('Ctrl Pts',(4.63289901592379,-0.437847975619643,
-4.10700154852122));
#10175=CARTESIAN_POINT('Ctrl Pts',(4.62771144039552,-0.450497029118683,
-4.10794371151065));
#10176=CARTESIAN_POINT('Ctrl Pts',(4.62621474454141,-0.454095496898909,
-4.10821130522183));
#10177=CARTESIAN_POINT('Ctrl Pts',(4.62359407183916,-0.460309148342149,
-4.10867253232959));
#10178=CARTESIAN_POINT('Ctrl Pts',(4.62247843733562,-0.462927781455639,
-4.10886664879161));
#10179=CARTESIAN_POINT('Ctrl Pts',(4.62009496224947,-0.468466536049767,
-4.10927664100431));
#10180=CARTESIAN_POINT('Ctrl Pts',(4.6188247532074,-0.471385613965797,-4.10949236776013));
#10181=CARTESIAN_POINT('Ctrl Pts',(4.6156262748807,-0.478655355971944,-4.11002882959558));
#10182=CARTESIAN_POINT('Ctrl Pts',(4.6136834183443,-0.482999607611767,-4.11034870036592));
#10183=CARTESIAN_POINT('Ctrl Pts',(4.60613941028242,-0.499597426427108,
-4.11156853933936));
#10184=CARTESIAN_POINT('Ctrl Pts',(4.60035423009635,-0.511766880711835,
-4.11245815606025));
#10185=CARTESIAN_POINT('Ctrl Pts',(4.58483179596218,-0.543024275717131,
-4.11473756001972));
#10186=CARTESIAN_POINT('Ctrl Pts',(4.57477995345353,-0.561951131570074,
-4.11611230060897));
#10187=CARTESIAN_POINT('Ctrl Pts',(4.5362337869681,-0.629981713175678,-4.12107138806634));
#10188=CARTESIAN_POINT('Ctrl Pts',(4.5047154462433,-0.677284183241362,-4.12455703420347));
#10189=CARTESIAN_POINT('Ctrl Pts',(4.42391368575104,-0.781388509308156,
-4.13271764382273));
#10190=CARTESIAN_POINT('Ctrl Pts',(4.37237127889971,-0.836108158790844,
-4.13740404485252));
#10191=CARTESIAN_POINT('Ctrl Pts',(4.30816407226216,-0.892405715595032,
-4.14300835080058));
#10192=CARTESIAN_POINT('Ctrl Pts',(4.30025742242843,-0.899155297470207,
-4.14369458669386));
#10193=CARTESIAN_POINT('Ctrl Pts',(4.28708932886012,-0.910098339529067,
-4.1448317960199));
#10194=CARTESIAN_POINT('Ctrl Pts',(4.28187935224092,-0.914353043386512,
-4.14528030531816));
#10195=CARTESIAN_POINT('Ctrl Pts',(4.272400278373,-0.921959665791854,-4.14609392861899));
#10196=CARTESIAN_POINT('Ctrl Pts',(4.26814388388235,-0.925327169173477,
-4.14645841195714));
#10197=CARTESIAN_POINT('Ctrl Pts',(4.25896009315414,-0.932490393514595,
-4.14724309603075));
#10198=CARTESIAN_POINT('Ctrl Pts',(4.25402561818826,-0.936276727267058,
-4.1476636488251));
#10199=CARTESIAN_POINT('Ctrl Pts',(4.24042427079647,-0.946543205108173,
-4.14882011922744));
#10200=CARTESIAN_POINT('Ctrl Pts',(4.23169789337818,-0.952943126791585,
-4.14955908759421));
#10201=CARTESIAN_POINT('Ctrl Pts',(4.17960771115787,-0.990053053102572,
-4.15395390652374));
#10202=CARTESIAN_POINT('Ctrl Pts',(4.13430009814544,-1.01791580728556,-4.15771485253991));
#10203=CARTESIAN_POINT('Ctrl Pts',(4.08424467547647,-1.04421298248778,-4.16180092982385));
#10204=CARTESIAN_POINT('Ctrl Pts',(4.08121028447338,-1.04579030560513,-4.16204835369644));
#10205=CARTESIAN_POINT('Ctrl Pts',(4.07816926526045,-1.04735428989218,-4.16229603312229));
#10206=CARTESIAN_POINT('Origin',(3.53951905042299,8.32667268468867E-16,
0.924367114736157));
#10207=CARTESIAN_POINT('',(4.07816946571175,-1.04735418680084,-4.76238152739268));
#10208=CARTESIAN_POINT('',(4.07816926754731,-1.04735428871606,-4.66391540717653));
#10209=CARTESIAN_POINT('',(4.07816926754759,-1.04735428871592,0.924367114736157));
#10210=CARTESIAN_POINT('Ctrl Pts',(4.07816946571175,-1.04735418680084,-4.76238152739268));
#10211=CARTESIAN_POINT('Ctrl Pts',(4.1238246947715,-1.02387387001492,-4.75872475031135));
#10212=CARTESIAN_POINT('Ctrl Pts',(4.16791639040916,-0.997422887860836,
-4.75498284712457));
#10213=CARTESIAN_POINT('Ctrl Pts',(4.2352999419459,-0.950746764474624,-4.74897178872223));
#10214=CARTESIAN_POINT('Ctrl Pts',(4.25975379432268,-0.932358515856194,
-4.74672343589551));
#10215=CARTESIAN_POINT('Ctrl Pts',(4.32002382529312,-0.883250431994198,
-4.74104387231585));
#10216=CARTESIAN_POINT('Ctrl Pts',(4.35476568563751,-0.851289022416631,
-4.73763586798109));
#10217=CARTESIAN_POINT('Ctrl Pts',(4.39225537096927,-0.81239324041436,-4.73387966196873));
#10218=CARTESIAN_POINT('Ctrl Pts',(4.3969673253232,-0.807418398921939,-4.733406051962));
#10219=CARTESIAN_POINT('Ctrl Pts',(4.4041150996941,-0.799738693321236,-4.73268567264392));
#10220=CARTESIAN_POINT('Ctrl Pts',(4.4065821485723,-0.797063291551279,-4.73243667380822));
#10221=CARTESIAN_POINT('Ctrl Pts',(4.41108942919161,-0.792129660296022,
-4.73198115996995));
#10222=CARTESIAN_POINT('Ctrl Pts',(4.41313331394922,-0.789874953933117,
-4.73177438116093));
#10223=CARTESIAN_POINT('Ctrl Pts',(4.4177448111186,-0.784747995926978,-4.73130731525029));
#10224=CARTESIAN_POINT('Ctrl Pts',(4.4203070864187,-0.781871051108427,-4.73104742012281));
#10225=CARTESIAN_POINT('Ctrl Pts',(4.42692415251358,-0.774367543361832,
-4.73037508745562));
#10226=CARTESIAN_POINT('Ctrl Pts',(4.43095695452565,-0.769721621456751,
-4.72996419124905));
#10227=CARTESIAN_POINT('Ctrl Pts',(4.4381340580166,-0.76132129092274,-4.72923040728557));
#10228=CARTESIAN_POINT('Ctrl Pts',(4.44129165541683,-0.757578517782859,
-4.72890667901163));
#10229=CARTESIAN_POINT('Ctrl Pts',(4.48956575480433,-0.699628624190789,
-4.7239415697203));
#10230=CARTESIAN_POINT('Ctrl Pts',(4.52975368333266,-0.641488184859085,
-4.71958737884043));
#10231=CARTESIAN_POINT('Ctrl Pts',(4.59370219690835,-0.528495972568149,
-4.71155631277819));
#10232=CARTESIAN_POINT('Ctrl Pts',(4.61896435276189,-0.474770765827193,
-4.70789364112963));
#10233=CARTESIAN_POINT('Ctrl Pts',(4.64765982860039,-0.399465858020155,
-4.70275788393481));
#10234=CARTESIAN_POINT('Ctrl Pts',(4.6547040933971,-0.379356289809559,-4.70138686441829));
#10235=CARTESIAN_POINT('Ctrl Pts',(4.66600392484798,-0.344057108959871,
-4.69897265587932));
#10236=CARTESIAN_POINT('Ctrl Pts',(4.6705070366421,-0.328952281353088,-4.69793725027693));
#10237=CARTESIAN_POINT('Ctrl Pts',(4.67662500865674,-0.306817559307883,
-4.69641438477839));
#10238=CARTESIAN_POINT('Ctrl Pts',(4.67848068322941,-0.299855582053656,
-4.69593461202283));
#10239=CARTESIAN_POINT('Ctrl Pts',(4.68163547460494,-0.28756770408172,-4.69508622319637));
#10240=CARTESIAN_POINT('Ctrl Pts',(4.68296151637903,-0.282248890403064,
-4.69471847633296));
#10241=CARTESIAN_POINT('Ctrl Pts',(4.68564910064335,-0.271139003953795,
-4.69394915286868));
#10242=CARTESIAN_POINT('Ctrl Pts',(4.68700398954536,-0.265346497493998,
-4.69354737666264));
#10243=CARTESIAN_POINT('Ctrl Pts',(4.69042468190771,-0.250205803618211,
-4.6924953408747));
#10244=CARTESIAN_POINT('Ctrl Pts',(4.69242045126806,-0.240842411741294,
-4.69184289267613));
#10245=CARTESIAN_POINT('Ctrl Pts',(4.70035920076625,-0.201234311809141,
-4.6890745483797));
#10246=CARTESIAN_POINT('Ctrl Pts',(4.70522735884054,-0.170789169666245,
-4.68692554824044));
#10247=CARTESIAN_POINT('Ctrl Pts',(4.71879790977702,-0.0575925486884402,
-4.67885281023103));
#10248=CARTESIAN_POINT('Ctrl Pts',(4.71991974477076,0.0258138003403826,
-4.67272135094934));
#10249=CARTESIAN_POINT('Ctrl Pts',(4.70743430651301,0.160604102838441,-4.66281207693023));
#10250=CARTESIAN_POINT('Ctrl Pts',(4.69916917891795,0.212208870744189,-4.6590249514404));
#10251=CARTESIAN_POINT('Ctrl Pts',(4.685951249501,0.269882742669623,-4.65490958087788));
#10252=CARTESIAN_POINT('Ctrl Pts',(4.68433667025753,0.276651595047297,-4.65442848822193));
#10253=CARTESIAN_POINT('Ctrl Pts',(4.68178106355983,0.286959862182702,-4.65369915039173));
#10254=CARTESIAN_POINT('Ctrl Pts',(4.68088339844669,0.290509716078846,-4.65344859169957));
#10255=CARTESIAN_POINT('Ctrl Pts',(4.6792096715083,0.297001017343397,-4.65299159445252));
#10256=CARTESIAN_POINT('Ctrl Pts',(4.67843876660333,0.299943655767906,-4.65278487989882));
#10257=CARTESIAN_POINT('Ctrl Pts',(4.67667258082573,0.306580408305435,-4.65231966270194));
#10258=CARTESIAN_POINT('Ctrl Pts',(4.67567069636531,0.310272681555549,-4.65206153818263));
#10259=CARTESIAN_POINT('Ctrl Pts',(4.67303457660165,0.319803649209355,-4.65139687125989));
#10260=CARTESIAN_POINT('Ctrl Pts',(4.67137319128884,0.325634810421166,-4.65099181272067));
#10261=CARTESIAN_POINT('Ctrl Pts',(4.65991569380577,0.364701175228601,-4.64828718311037));
#10262=CARTESIAN_POINT('Ctrl Pts',(4.64870106091063,0.397506425981322,-4.64606017966695));
#10263=CARTESIAN_POINT('Ctrl Pts',(4.62576276797231,0.45603194171076,-4.64208820862212));
#10264=CARTESIAN_POINT('Ctrl Pts',(4.61453037715098,0.48191421850553,-4.64033201442321));
#10265=CARTESIAN_POINT('Ctrl Pts',(4.58172188548151,0.550642952029911,-4.63561006395663));
#10266=CARTESIAN_POINT('Ctrl Pts',(4.55844147314865,0.592614051619709,-4.63266126320182));
#10267=CARTESIAN_POINT('Ctrl Pts',(4.50398848110103,0.678041773187614,-4.62632615764673));
#10268=CARTESIAN_POINT('Ctrl Pts',(4.47228843409243,0.721028515699199,-4.62293442276487));
#10269=CARTESIAN_POINT('Ctrl Pts',(4.43078056935493,0.769977478529743,-4.61871635005542));
#10270=CARTESIAN_POINT('Ctrl Pts',(4.42366093030718,0.778142362314284,-4.61800003007169));
#10271=CARTESIAN_POINT('Ctrl Pts',(4.41227582210453,0.790840946984347,-4.6168649893465));
#10272=CARTESIAN_POINT('Ctrl Pts',(4.40808519070023,0.795441162752092,-4.61644935882164));
#10273=CARTESIAN_POINT('Ctrl Pts',(4.40017123992361,0.803991502048321,-4.61566831401971));
#10274=CARTESIAN_POINT('Ctrl Pts',(4.39645667032949,0.807949528471788,-4.61530327379224));
#10275=CARTESIAN_POINT('Ctrl Pts',(4.38807922392196,0.816753277707682,-4.61448337298019));
#10276=CARTESIAN_POINT('Ctrl Pts',(4.38340196886911,0.821584993416335,-4.61402790462501));
#10277=CARTESIAN_POINT('Ctrl Pts',(4.37139495021376,0.833777822828424,-4.61286428822969));
#10278=CARTESIAN_POINT('Ctrl Pts',(4.36400883136035,0.841082373874477,-4.61215371007682));
#10279=CARTESIAN_POINT('Ctrl Pts',(4.30215082478109,0.900659421815302,-4.60624379587351));
#10280=CARTESIAN_POINT('Ctrl Pts',(4.24287507936599,0.947671371370007,-4.60082261416592));
#10281=CARTESIAN_POINT('Ctrl Pts',(4.13093969741506,1.02013027262249,-4.59106833800458));
#10282=CARTESIAN_POINT('Ctrl Pts',(4.08010624888138,1.04795509911427,-4.58679405682858));
#10283=CARTESIAN_POINT('Ctrl Pts',(4.00882890120997,1.08039859683487,-4.58113930347216));
#10284=CARTESIAN_POINT('Ctrl Pts',(3.99000679871422,1.08838125292876,-4.57967673296068));
#10285=CARTESIAN_POINT('Ctrl Pts',(3.95886544462656,1.10064223438424,-4.57731650350475));
#10286=CARTESIAN_POINT('Ctrl Pts',(3.94666652491785,1.10521296392672,-4.57640657905525));
#10287=CARTESIAN_POINT('Ctrl Pts',(3.92996727155447,1.11115585025934,-4.5751830844287));
#10288=CARTESIAN_POINT('Ctrl Pts',(3.92553138983615,1.11270463855083,-4.57486018521342));
#10289=CARTESIAN_POINT('Ctrl Pts',(3.91808610542428,1.11525427768112,-4.57432187502797));
#10290=CARTESIAN_POINT('Ctrl Pts',(3.91508175158232,1.11626958092452,-4.57410564486279));
#10291=CARTESIAN_POINT('Ctrl Pts',(3.9093624494946,1.11817668027466,-4.5736959431407));
#10292=CARTESIAN_POINT('Ctrl Pts',(3.90664830748703,1.11907074718166,-4.57350233647787));
#10293=CARTESIAN_POINT('Ctrl Pts',(3.90018362210851,1.12117423178074,-4.57304308390726));
#10294=CARTESIAN_POINT('Ctrl Pts',(3.89643018005682,1.12237473150809,-4.57277794747231));
#10295=CARTESIAN_POINT('Ctrl Pts',(3.8831013744508,1.12656418737,-4.57184153023339));
#10296=CARTESIAN_POINT('Ctrl Pts',(3.87349360583694,1.12944973078449,-4.57117585026772));
#10297=CARTESIAN_POINT('Ctrl Pts',(3.80607251562621,1.14876300806629,-4.56656177230268));
#10298=CARTESIAN_POINT('Ctrl Pts',(3.74710528944598,1.1608690782246,-4.56281639306572));
#10299=CARTESIAN_POINT('Ctrl Pts',(3.62350441213244,1.1765194676904,-4.55509780781357));
#10300=CARTESIAN_POINT('Ctrl Pts',(3.55899030526028,1.17935234291728,-4.55113797056606));
#10301=CARTESIAN_POINT('Ctrl Pts',(3.45836278618677,1.17550908349376,-4.54474872733253));
#10302=CARTESIAN_POINT('Ctrl Pts',(3.42224176952475,1.172456217751,-4.54241368065164));
#10303=CARTESIAN_POINT('Ctrl Pts',(3.3766537614248,1.16647547415376,-4.53938475671786));
#10304=CARTESIAN_POINT('Ctrl Pts',(3.36700250241469,1.16508719220557,-4.53873887477249));
#10305=CARTESIAN_POINT('Ctrl Pts',(3.3514544565316,1.16265326736094,-4.53769036111547));
#10306=CARTESIAN_POINT('Ctrl Pts',(3.34554632888212,1.16168218228574,-4.53729006153443));
#10307=CARTESIAN_POINT('Ctrl Pts',(3.3342551365963,1.15973777677597,-4.53652133093436));
#10308=CARTESIAN_POINT('Ctrl Pts',(3.32887093221674,1.15877191619635,-4.53615314293425));
#10309=CARTESIAN_POINT('Ctrl Pts',(3.31660915876159,1.1564840207008,-4.53531085702529));
#10310=CARTESIAN_POINT('Ctrl Pts',(3.30973631576003,1.15513808746904,-4.53483601966663));
#10311=CARTESIAN_POINT('Ctrl Pts',(3.28810787555828,1.15070185408713,-4.53333289264715));
#10312=CARTESIAN_POINT('Ctrl Pts',(3.27339988648215,1.14738959814153,-4.53229767962789));
#10313=CARTESIAN_POINT('Ctrl Pts',(3.17272848711102,1.12267855276493,-4.52511871423584));
#10314=CARTESIAN_POINT('Ctrl Pts',(3.0893694931513,1.09192588335594,-4.51867178672263));
#10315=CARTESIAN_POINT('Ctrl Pts',(2.99292161076762,1.04340933630333,-4.51074810682237));
#10316=CARTESIAN_POINT('Ctrl Pts',(2.97580012812239,1.03425953956536,-4.50932368888764));
#10317=CARTESIAN_POINT('Ctrl Pts',(2.92974969565556,1.00816660771333,-4.5054538473849));
#10318=CARTESIAN_POINT('Ctrl Pts',(2.9013035857772,0.990403907151046,-4.50302019637042));
#10319=CARTESIAN_POINT('Ctrl Pts',(2.85855157627035,0.961100165392884,-4.4993323716793));
#10320=CARTESIAN_POINT('Ctrl Pts',(2.84369318876685,0.950398174632091,-4.49804477577549));
#10321=CARTESIAN_POINT('Ctrl Pts',(2.82484564468024,0.936143843841808,-4.49640974199378));
#10322=CARTESIAN_POINT('Ctrl Pts',(2.82062357492806,0.932905499634276,-4.49604336134894));
#10323=CARTESIAN_POINT('Ctrl Pts',(2.81381399739052,0.927608844184126,-4.49545245028938));
#10324=CARTESIAN_POINT('Ctrl Pts',(2.81121301411879,0.925568101207468,-4.49522674788133));
#10325=CARTESIAN_POINT('Ctrl Pts',(2.80619428324002,0.921596127860086,-4.49479130272333));
#10326=CARTESIAN_POINT('Ctrl Pts',(2.80377551499016,0.919666291316708,-4.49458147296478));
#10327=CARTESIAN_POINT('Ctrl Pts',(2.79843241332152,0.915368677880096,-4.49411796106471));
#10328=CARTESIAN_POINT('Ctrl Pts',(2.79551173693431,0.912996351897627,-4.49386459628896));
#10329=CARTESIAN_POINT('Ctrl Pts',(2.78543378269944,0.904730034509634,-4.49299015633349));
#10330=CARTESIAN_POINT('Ctrl Pts',(2.77833454508543,0.898765368877215,-4.49237383639267));
#10331=CARTESIAN_POINT('Ctrl Pts',(2.70974674604248,0.839743291540491,-4.48640764485951));
#10332=CARTESIAN_POINT('Ctrl Pts',(2.65382227632774,0.780535743997938,-4.4814396272649));
#10333=CARTESIAN_POINT('Ctrl Pts',(2.57262647582614,0.674500209030629,-4.47317347145686));
#10334=CARTESIAN_POINT('Ctrl Pts',(2.54362590630552,0.630894624230979,-4.46992205464854));
#10335=CARTESIAN_POINT('Ctrl Pts',(2.50777661473052,0.568326282383951,-4.46531426749584));
#10336=CARTESIAN_POINT('Ctrl Pts',(2.49836714992258,0.550899147073555,-4.46403703316848));
#10337=CARTESIAN_POINT('Ctrl Pts',(2.48265645345692,0.519960067433883,-4.4617735734591));
#10338=CARTESIAN_POINT('Ctrl Pts',(2.47616396689979,0.506550051363631,-4.46079383024674));
#10339=CARTESIAN_POINT('Ctrl Pts',(2.46697818280256,0.486621823556924,-4.45933794604063));
#10340=CARTESIAN_POINT('Ctrl Pts',(2.46408608317694,0.480196461072343,-4.45886854933517));
#10341=CARTESIAN_POINT('Ctrl Pts',(2.45905545460417,0.468746515894298,-4.45803192760792));
#10342=CARTESIAN_POINT('Ctrl Pts',(2.45689386858019,0.463732241686929,-4.45766549209573));
#10343=CARTESIAN_POINT('Ctrl Pts',(2.45242051552263,0.453153554073311,-4.45689221362561));
#10344=CARTESIAN_POINT('Ctrl Pts',(2.45011643246739,0.447586083135522,-4.45648512597225));
#10345=CARTESIAN_POINT('Ctrl Pts',(2.44413054367867,0.432802011534879,-4.45540368601457));
#10346=CARTESIAN_POINT('Ctrl Pts',(2.44052241073127,0.423556297778087,-4.45472691424769));
#10347=CARTESIAN_POINT('Ctrl Pts',(2.42502190391518,0.382304783248453,-4.45170457801411));
#10348=CARTESIAN_POINT('Ctrl Pts',(2.41440885336671,0.349839212051453,-4.44931787050946));
#10349=CARTESIAN_POINT('Ctrl Pts',(2.37633410099366,0.213582501721775,-4.43926254119206));
#10350=CARTESIAN_POINT('Ctrl Pts',(2.36171861433284,0.106759320706611,-4.43123006619689));
#10351=CARTESIAN_POINT('Ctrl Pts',(2.36178118377105,-0.0260274178282911,
-4.42168786245795));
#10352=CARTESIAN_POINT('Ctrl Pts',(2.36261956795491,-0.0514950397899183,
-4.41988115543017));
#10353=CARTESIAN_POINT('Ctrl Pts',(2.36468223135748,-0.0830108380322754,
-4.41768959195174));
#10354=CARTESIAN_POINT('Ctrl Pts',(2.3651284275498,-0.089101176061268,-4.41726813729475));
#10355=CARTESIAN_POINT('Ctrl Pts',(2.36590606748946,-0.0986913546338751,
-4.41660801986475));
#10356=CARTESIAN_POINT('Ctrl Pts',(2.36620583704834,-0.102193548353958,
-4.41636769692345));
#10357=CARTESIAN_POINT('Ctrl Pts',(2.36676819616081,-0.108434616480967,
-4.41594081626785));
#10358=CARTESIAN_POINT('Ctrl Pts',(2.36702470305547,-0.111173908155267,
-4.41575393459828));
#10359=CARTESIAN_POINT('Ctrl Pts',(2.36766375870601,-0.117750183481974,
-4.41530641647577));
#10360=CARTESIAN_POINT('Ctrl Pts',(2.36805555386257,-0.121586215164551,
-4.41504629315816));
#10361=CARTESIAN_POINT('Ctrl Pts',(2.36930938676032,-0.133293286129065,
-4.41425505170988));
#10362=CARTESIAN_POINT('Ctrl Pts',(2.37023198647703,-0.141157810678305,
-4.41372713633098));
#10363=CARTESIAN_POINT('Ctrl Pts',(2.37256737398493,-0.159467651165253,
-4.41250526373565));
#10364=CARTESIAN_POINT('Ctrl Pts',(2.37404121832908,-0.169904640266484,
-4.41181424663582));
#10365=CARTESIAN_POINT('Ctrl Pts',(2.37971133060692,-0.206501852524029,
-4.40940604086706));
#10366=CARTESIAN_POINT('Ctrl Pts',(2.38465017131869,-0.232540369503318,
-4.40771928913578));
#10367=CARTESIAN_POINT('Ctrl Pts',(2.40761636396558,-0.334669910104225,
-4.40113243263604));
#10368=CARTESIAN_POINT('Ctrl Pts',(2.43232199428828,-0.409051428995215,
-4.3963869447157));
#10369=CARTESIAN_POINT('Ctrl Pts',(2.48337198574969,-0.523310008623693,
-4.38852799588136));
#10370=CARTESIAN_POINT('Ctrl Pts',(2.50507159987843,-0.564993516413902,
-4.38553011154634));
#10371=CARTESIAN_POINT('Ctrl Pts',(2.53472338837958,-0.614488637085034,
-4.38173836041264));
#10372=CARTESIAN_POINT('Ctrl Pts',(2.5403734212286,-0.623633391305754,-4.38102767055524));
#10373=CARTESIAN_POINT('Ctrl Pts',(2.54951440475064,-0.637985219207013,
-4.37989546916092));
#10374=CARTESIAN_POINT('Ctrl Pts',(2.55292320773736,-0.64324410530969,-4.37947695451095));
#10375=CARTESIAN_POINT('Ctrl Pts',(2.55906168205516,-0.652550567225135,
-4.37872967607215));
#10376=CARTESIAN_POINT('Ctrl Pts',(2.56177487480144,-0.656608878848639,
-4.37840152752093));
#10377=CARTESIAN_POINT('Ctrl Pts',(2.56811813037439,-0.665970431790652,
-4.3776391963065));
#10378=CARTESIAN_POINT('Ctrl Pts',(2.57176649839303,-0.671261021289354,
-4.37720433647599));
#10379=CARTESIAN_POINT('Ctrl Pts',(2.58222903663871,-0.686170418788252,
-4.37596719106977));
#10380=CARTESIAN_POINT('Ctrl Pts',(2.58914440931673,-0.695716923862671,
-4.37516110731957));
#10381=CARTESIAN_POINT('Ctrl Pts',(2.64607921557227,-0.771880863593361,
-4.36861424258325));
#10382=CARTESIAN_POINT('Ctrl Pts',(2.70288536552584,-0.833110917589799,
-4.3626008455239));
#10383=CARTESIAN_POINT('Ctrl Pts',(2.821787717027,-0.936749928707592,-4.35103695183046));
#10384=CARTESIAN_POINT('Ctrl Pts',(2.88243204106732,-0.980243454152859,
-4.34553716821826));
#10385=CARTESIAN_POINT('Ctrl Pts',(2.95509337063497,-1.02256256739274,-4.33964601278877));
#10386=CARTESIAN_POINT('Ctrl Pts',(2.96346433341195,-1.02730159018917,-4.33897723883132));
#10387=CARTESIAN_POINT('Ctrl Pts',(2.97528465929047,-1.03380346318538,-4.33804767069479));
#10388=CARTESIAN_POINT('Ctrl Pts',(2.97868581417824,-1.03565251451142,-4.33778189455228));
#10389=CARTESIAN_POINT('Ctrl Pts',(2.98484650193509,-1.03896254745117,-4.33730361903064));
#10390=CARTESIAN_POINT('Ctrl Pts',(2.98760283921663,-1.04042938619351,-4.33709076235831));
#10391=CARTESIAN_POINT('Ctrl Pts',(2.99324952702244,-1.0434056268094,-4.33665704795359));
#10392=CARTESIAN_POINT('Ctrl Pts',(2.99614036412811,-1.0449140147353,-4.33643625278272));
#10393=CARTESIAN_POINT('Ctrl Pts',(3.00358211682221,-1.04875775542582,-4.33587096709932));
#10394=CARTESIAN_POINT('Ctrl Pts',(3.00814210817067,-1.0510755320086,-4.3355275448279));
#10395=CARTESIAN_POINT('Ctrl Pts',(3.02735982112843,-1.06068657965286,-4.33409200649674));
#10396=CARTESIAN_POINT('Ctrl Pts',(3.04215449354165,-1.06770391955412,-4.33301550847004));
#10397=CARTESIAN_POINT('Ctrl Pts',(3.08293610833501,-1.08601550943427,-4.3301126263949));
#10398=CARTESIAN_POINT('Ctrl Pts',(3.10919280319622,-1.09668464625338,-4.3283135884314));
#10399=CARTESIAN_POINT('Ctrl Pts',(3.21661103250613,-1.1358800355342,-4.32113582233972));
#10400=CARTESIAN_POINT('Ctrl Pts',(3.30039712128703,-1.15642306316942,-4.31592820504046));
#10401=CARTESIAN_POINT('Ctrl Pts',(3.42293373409073,-1.17256780104991,-4.30810182028285));
#10402=CARTESIAN_POINT('Ctrl Pts',(3.46040283498772,-1.17569025205965,-4.30568450785861));
#10403=CARTESIAN_POINT('Ctrl Pts',(3.50818498931754,-1.17737760879424,-4.30253817323958));
#10404=CARTESIAN_POINT('Ctrl Pts',(3.51841953553587,-1.17760547583808,-4.30186061783616));
#10405=CARTESIAN_POINT('Ctrl Pts',(3.53474874289516,-1.17775610272775,-4.30077319581822));
#10406=CARTESIAN_POINT('Ctrl Pts',(3.54084223776515,-1.17776501907845,-4.30036599122266));
#10407=CARTESIAN_POINT('Ctrl Pts',(3.55238136229922,-1.17769235488938,-4.29959207029288));
#10408=CARTESIAN_POINT('Ctrl Pts',(3.55782690913985,-1.1776202878829,-4.29922565772469));
#10409=CARTESIAN_POINT('Ctrl Pts',(3.57019323854404,-1.17737083542516,-4.29839078810382));
#10410=CARTESIAN_POINT('Ctrl Pts',(3.57711329750726,-1.17717019116737,-4.29792162507653));
#10411=CARTESIAN_POINT('Ctrl Pts',(3.59826989956933,-1.17637002461012,-4.29648098961761));
#10412=CARTESIAN_POINT('Ctrl Pts',(3.61249722485612,-1.17557315905028,-4.29550349020484));
#10413=CARTESIAN_POINT('Ctrl Pts',(3.68125472776603,-1.17046914231167,-4.29073529620166));
#10414=CARTESIAN_POINT('Ctrl Pts',(3.73544722109135,-1.1626253247207,-4.28683795613902));
#10415=CARTESIAN_POINT('Ctrl Pts',(3.87200461050891,-1.13304029791378,-4.27669384363175));
#10416=CARTESIAN_POINT('Ctrl Pts',(3.95291985471189,-1.10608616546657,-4.2703599530123));
#10417=CARTESIAN_POINT('Ctrl Pts',(4.04638062721946,-1.06325075396286,-4.26301792008229));
#10418=CARTESIAN_POINT('Ctrl Pts',(4.06236558022085,-1.05548206334191,-4.26176216134083));
#10419=CARTESIAN_POINT('Ctrl Pts',(4.07816926766421,-1.04735428865594,-4.2605248066102));
#10420=CARTESIAN_POINT('',(2.36176954983345,0.00105548582028932,-4.32555179375738));
#10421=CARTESIAN_POINT('Ctrl Pts',(4.07816926526045,-1.04735428989218,-4.16229603312229));
#10422=CARTESIAN_POINT('Ctrl Pts',(4.03842873019156,-1.06779269164334,-4.16553274825607));
#10423=CARTESIAN_POINT('Ctrl Pts',(3.99755637743545,-1.08595305923346,-4.16881511342479));
#10424=CARTESIAN_POINT('Ctrl Pts',(3.9292887858117,-1.11174402647986,-4.17416938912811));
#10425=CARTESIAN_POINT('Ctrl Pts',(3.9024746683188,-1.12078478808358,-4.1762411837762));
#10426=CARTESIAN_POINT('Ctrl Pts',(3.8421510273945,-1.13873149645923,-4.18080431744579));
#10427=CARTESIAN_POINT('Ctrl Pts',(3.80851831929176,-1.14714228561079,-4.18328330394645));
#10428=CARTESIAN_POINT('Ctrl Pts',(3.76862008123459,-1.15526816455367,-4.18611338118691));
#10429=CARTESIAN_POINT('Ctrl Pts',(3.76267029062669,-1.15643216066189,-4.18653254488164));
#10430=CARTESIAN_POINT('Ctrl Pts',(3.75295203356498,-1.15825560923789,-4.1872122398664));
#10431=CARTESIAN_POINT('Ctrl Pts',(3.74918896285268,-1.15894271794807,-4.18747422067267));
#10432=CARTESIAN_POINT('Ctrl Pts',(3.7424279137746,-1.16014322660198,-4.1879426700595));
#10433=CARTESIAN_POINT('Ctrl Pts',(3.73943124288457,-1.1606633573098,-4.18814950233272));
#10434=CARTESIAN_POINT('Ctrl Pts',(3.73282321093215,-1.16178395817205,-4.18860383800169));
#10435=CARTESIAN_POINT('Ctrl Pts',(3.72921104802691,-1.16237920270958,-4.1888510499588));
#10436=CARTESIAN_POINT('Ctrl Pts',(3.71872685249991,-1.16405670861132,-4.1895654184471));
#10437=CARTESIAN_POINT('Ctrl Pts',(3.71184778945889,-1.16509496122081,-4.1900302142957));
#10438=CARTESIAN_POINT('Ctrl Pts',(3.65333467248538,-1.17339671938536,-4.1939535373333));
#10439=CARTESIAN_POINT('Ctrl Pts',(3.60127289576342,-1.17728576838526,-4.19724591676357));
#10440=CARTESIAN_POINT('Ctrl Pts',(3.46609504889203,-1.17838760177226,-4.20566682200954));
#10441=CARTESIAN_POINT('Ctrl Pts',(3.38323679052929,-1.17028368310989,-4.21071921608285));
#10442=CARTESIAN_POINT('Ctrl Pts',(3.27155694966704,-1.1472804337431,-4.2179903911338));
#10443=CARTESIAN_POINT('Ctrl Pts',(3.24145512439798,-1.13983056486589,-4.21999557709433));
#10444=CARTESIAN_POINT('Ctrl Pts',(3.20247165595037,-1.12853272570261,-4.22267031257472));
#10445=CARTESIAN_POINT('Ctrl Pts',(3.19329243811487,-1.12575049770806,-4.22330583709509));
#10446=CARTESIAN_POINT('Ctrl Pts',(3.17847371302215,-1.12106054919905,-4.22434159583032));
#10447=CARTESIAN_POINT('Ctrl Pts',(3.1728127686685,-1.11922160064533,-4.22473960168163));
#10448=CARTESIAN_POINT('Ctrl Pts',(3.1619677169476,-1.11560749247629,-4.22550669483037));
#10449=CARTESIAN_POINT('Ctrl Pts',(3.15678157008866,-1.1138389049072,-4.22587555965276));
#10450=CARTESIAN_POINT('Ctrl Pts',(3.14521420798989,-1.109803860669,-4.22670294700959));
#10451=CARTESIAN_POINT('Ctrl Pts',(3.13883986130714,-1.10751844319511,-4.2271620801068));
#10452=CARTESIAN_POINT('Ctrl Pts',(3.11885634526022,-1.10015858259009,-4.22861172611622));
#10453=CARTESIAN_POINT('Ctrl Pts',(3.10532157626562,-1.0948874550087,-4.22960865465041));
#10454=CARTESIAN_POINT('Ctrl Pts',(3.07396924328436,-1.08200450339694,-4.23195442351519));
#10455=CARTESIAN_POINT('Ctrl Pts',(3.05623557979995,-1.07420081041973,-4.23330928520239));
#10456=CARTESIAN_POINT('Ctrl Pts',(2.99304099547762,-1.04451045178818,-4.2382402260481));
#10457=CARTESIAN_POINT('Ctrl Pts',(2.94880912494815,-1.02014761218482,-4.2418902519446));
#10458=CARTESIAN_POINT('Ctrl Pts',(2.83619086249014,-0.948332497442498,
-4.25165923718373));
#10459=CARTESIAN_POINT('Ctrl Pts',(2.77102725109173,-0.896341015665466,
-4.25783057899671));
#10460=CARTESIAN_POINT('Ctrl Pts',(2.7049714878899,-0.831095472775577,-4.26433674777524));
#10461=CARTESIAN_POINT('Ctrl Pts',(2.69814859850046,-0.824187537393891,
-4.26501188448792));
#10462=CARTESIAN_POINT('Ctrl Pts',(2.68871514924872,-0.814397253743633,
-4.26594876362327));
#10463=CARTESIAN_POINT('Ctrl Pts',(2.68603247353762,-0.811585380170657,
-4.26621558880821));
#10464=CARTESIAN_POINT('Ctrl Pts',(2.68141102118401,-0.806693100691683,
-4.26667585860686));
#10465=CARTESIAN_POINT('Ctrl Pts',(2.67946579057232,-0.804618878231609,
-4.26686978163389));
#10466=CARTESIAN_POINT('Ctrl Pts',(2.6753564976189,-0.800205161704783,-4.26727980749679));
#10467=CARTESIAN_POINT('Ctrl Pts',(2.67319437850884,-0.797863886786371,
-4.26749575899937));
#10468=CARTESIAN_POINT('Ctrl Pts',(2.66884822288553,-0.793119107640423,
-4.2679303576441));
#10469=CARTESIAN_POINT('Ctrl Pts',(2.66666456611978,-0.790715282944737,
-4.26814897653004));
#10470=CARTESIAN_POINT('Ctrl Pts',(2.65847382333725,-0.781623428425936,
-4.26897013137225));
#10471=CARTESIAN_POINT('Ctrl Pts',(2.65253324175446,-0.774875514687234,
-4.26956800864679));
#10472=CARTESIAN_POINT('Ctrl Pts',(2.6198939868497,-0.736933272474278,-4.27287033166498));
#10473=CARTESIAN_POINT('Ctrl Pts',(2.59476068760359,-0.704424075175968,
-4.27547977097146));
#10474=CARTESIAN_POINT('Ctrl Pts',(2.53827653098532,-0.622885875337787,
-4.28169076046831));
#10475=CARTESIAN_POINT('Ctrl Pts',(2.50876018827381,-0.572721454260407,
-4.28524823622344));
#10476=CARTESIAN_POINT('Ctrl Pts',(2.45648478836044,-0.466635527591634,
-4.29261140101451));
#10477=CARTESIAN_POINT('Ctrl Pts',(2.43407624211017,-0.410739224321567,
-4.29641172537716));
#10478=CARTESIAN_POINT('Ctrl Pts',(2.41294152163777,-0.343546816669302,
-4.30103540528726));
#10479=CARTESIAN_POINT('Ctrl Pts',(2.40997758911924,-0.333672623777673,
-4.30171604188615));
#10480=CARTESIAN_POINT('Ctrl Pts',(2.40530183598868,-0.317318872946005,
-4.30284588286288));
#10481=CARTESIAN_POINT('Ctrl Pts',(2.40351497600178,-0.310861217314879,
-4.30329267889362));
#10482=CARTESIAN_POINT('Ctrl Pts',(2.40038109898855,-0.299147501021571,
-4.30410447596302));
#10483=CARTESIAN_POINT('Ctrl Pts',(2.39901510796192,-0.293896674553662,
-4.3044688593917));
#10484=CARTESIAN_POINT('Ctrl Pts',(2.39615645014559,-0.282587953844677,
-4.30525476346907));
#10485=CARTESIAN_POINT('Ctrl Pts',(2.39467554785014,-0.276527285095791,
-4.30567664633791));
#10486=CARTESIAN_POINT('Ctrl Pts',(2.39174467597918,-0.264105308721656,
-4.30654286851939));
#10487=CARTESIAN_POINT('Ctrl Pts',(2.39029927535561,-0.257743155773501,
-4.30698733670704));
#10488=CARTESIAN_POINT('Ctrl Pts',(2.38677856568495,-0.241627546435829,
-4.30811538131316));
#10489=CARTESIAN_POINT('Ctrl Pts',(2.38477416347312,-0.231859293229989,
-4.30880115038773));
#10490=CARTESIAN_POINT('Ctrl Pts',(2.36877311963858,-0.148518657131392,
-4.31467022141069));
#10491=CARTESIAN_POINT('Ctrl Pts',(2.36170241876881,-0.0738064342619328,
-4.32006890540583));
#10492=CARTESIAN_POINT('Ctrl Pts',(2.36176952358042,0.00105570928602091,
-4.32555176752495));
#10493=CARTESIAN_POINT('Ctrl Pts',(2.36176952338293,0.00105548894706701,
-4.32555175138744));
#10494=CARTESIAN_POINT('Ctrl Pts',(2.36183394678726,0.0729412573325759,
-4.3308166253243));
#10495=CARTESIAN_POINT('Ctrl Pts',(2.36847963152645,0.14467607557027,-4.33613413493838));
#10496=CARTESIAN_POINT('Ctrl Pts',(2.38348249949644,0.225338683748339,-4.34194114727436));
#10497=CARTESIAN_POINT('Ctrl Pts',(2.38546694400475,0.235290842856999,-4.34265435503951));
#10498=CARTESIAN_POINT('Ctrl Pts',(2.38871217779652,0.250535789214435,-4.34374062493111));
#10499=CARTESIAN_POINT('Ctrl Pts',(2.38988137145093,0.255847316902987,-4.34411792458011));
#10500=CARTESIAN_POINT('Ctrl Pts',(2.39213032186502,0.265737262467958,-4.34481802849396));
#10501=CARTESIAN_POINT('Ctrl Pts',(2.39320079076264,0.270317658584731,-4.3451413002702));
#10502=CARTESIAN_POINT('Ctrl Pts',(2.39503904195511,0.277975959409702,-4.34568003428197));
#10503=CARTESIAN_POINT('Ctrl Pts',(2.39579186011124,0.281057358398529,-4.34589631870806));
#10504=CARTESIAN_POINT('Ctrl Pts',(2.39724614751359,0.286907362079868,-4.34630596974061));
#10505=CARTESIAN_POINT('Ctrl Pts',(2.39794525055704,0.289676507571524,-4.34649947238966));
#10506=CARTESIAN_POINT('Ctrl Pts',(2.39963166297419,0.296255456198783,-4.34695828366771));
#10507=CARTESIAN_POINT('Ctrl Pts',(2.40062801707942,0.300062937838093,-4.34722308490851));
#10508=CARTESIAN_POINT('Ctrl Pts',(2.40422414701941,0.313529256182683,-4.34815728113886));
#10509=CARTESIAN_POINT('Ctrl Pts',(2.40692794912355,0.323160216744212,-4.34882110926691));
#10510=CARTESIAN_POINT('Ctrl Pts',(2.42696954402347,0.391204947348311,-4.35348828969844));
#10511=CARTESIAN_POINT('Ctrl Pts',(2.44869711854392,0.448237836797384,-4.35728266093201));
#10512=CARTESIAN_POINT('Ctrl Pts',(2.50193984352266,0.560868728473025,-4.36499926713142));
#10513=CARTESIAN_POINT('Ctrl Pts',(2.53375147688438,0.616096914193811,-4.36890952225803));
#10514=CARTESIAN_POINT('Ctrl Pts',(2.59043626803981,0.698319538448475,-4.37524568888485));
#10515=CARTESIAN_POINT('Ctrl Pts',(2.61236937664674,0.72718731189892,-4.37758094089741));
#10516=CARTESIAN_POINT('Ctrl Pts',(2.64159123071168,0.762173299544365,-4.38058374496643));
#10517=CARTESIAN_POINT('Ctrl Pts',(2.64767095008627,0.769278535775692,-4.38120301094996));
#10518=CARTESIAN_POINT('Ctrl Pts',(2.65784986421826,0.780891553448013,-4.38223134897906));
#10519=CARTESIAN_POINT('Ctrl Pts',(2.66190065301687,0.785441352571194,-4.38263843901499));
#10520=CARTESIAN_POINT('Ctrl Pts',(2.66963886772805,0.79399822531299,-4.38341219774291));
#10521=CARTESIAN_POINT('Ctrl Pts',(2.67331915499885,0.798011562263318,-4.38377856320098));
#10522=CARTESIAN_POINT('Ctrl Pts',(2.68174149435467,0.807069177541713,-4.38461340160357));
#10523=CARTESIAN_POINT('Ctrl Pts',(2.68650042352199,0.812097415124681,-4.38508258095322));
#10524=CARTESIAN_POINT('Ctrl Pts',(2.70119193678458,0.827348702789837,-4.38652354180177));
#10525=CARTESIAN_POINT('Ctrl Pts',(2.71126569473357,0.837433324734496,-4.38750135514587));
#10526=CARTESIAN_POINT('Ctrl Pts',(2.78884448683518,0.912326504248746,-4.39495873255046));
#10527=CARTESIAN_POINT('Ctrl Pts',(2.86366331523872,0.969053290894656,-4.40178300698536));
#10528=CARTESIAN_POINT('Ctrl Pts',(2.98314851466393,1.0390210823148,-4.41194389047282));
#10529=CARTESIAN_POINT('Ctrl Pts',(3.02318197688122,1.05948548559944,-4.4152342799495));
#10530=CARTESIAN_POINT('Ctrl Pts',(3.07773889826031,1.08354521867975,-4.41949861387452));
#10531=CARTESIAN_POINT('Ctrl Pts',(3.09129951992364,1.08922469892963,-4.42054113177716));
#10532=CARTESIAN_POINT('Ctrl Pts',(3.11436202435343,1.09838008782103,-4.42228101421727));
#10533=CARTESIAN_POINT('Ctrl Pts',(3.12380854868405,1.10199006799592,-4.42298446086923));
#10534=CARTESIAN_POINT('Ctrl Pts',(3.13734845472276,1.10696543321352,-4.42397849635867));
#10535=CARTESIAN_POINT('Ctrl Pts',(3.14140434561515,1.10843057593146,-4.42427445501353));
#10536=CARTESIAN_POINT('Ctrl Pts',(3.1483876930897,1.1109099518838,-4.42478082434258));
#10537=CARTESIAN_POINT('Ctrl Pts',(3.15131124679629,1.11193496303143,-4.42499185142925));
#10538=CARTESIAN_POINT('Ctrl Pts',(3.15742425779173,1.11405116328907,-4.42543105323434));
#10539=CARTESIAN_POINT('Ctrl Pts',(3.16061438774708,1.11514020746468,-4.42565910479114));
#10540=CARTESIAN_POINT('Ctrl Pts',(3.16913127398431,1.11800692799571,-4.42626499779542));
#10541=CARTESIAN_POINT('Ctrl Pts',(3.17446622338382,1.11976025673737,-4.42664146055877));
#10542=CARTESIAN_POINT('Ctrl Pts',(3.19803340228195,1.12731926491622,-4.42829185018616));
#10543=CARTESIAN_POINT('Ctrl Pts',(3.21639414205139,1.13271866213725,-4.42954443600009));
#10544=CARTESIAN_POINT('Ctrl Pts',(3.31806433321148,1.15994342534524,-4.43634070379639));
#10545=CARTESIAN_POINT('Ctrl Pts',(3.4034492200047,1.17302985393893,-4.44155319599446));
#10546=CARTESIAN_POINT('Ctrl Pts',(3.54462475894067,1.17903039484465,-4.45035176304717));
#10547=CARTESIAN_POINT('Ctrl Pts',(3.59983477587177,1.17749720922757,-4.45383414458074));
#10548=CARTESIAN_POINT('Ctrl Pts',(3.66896987633567,1.17070161835792,-4.45837016550041));
#10549=CARTESIAN_POINT('Ctrl Pts',(3.68318252799158,1.16904258774411,-4.45931180626223));
#10550=CARTESIAN_POINT('Ctrl Pts',(3.70423214420707,1.16619583953559,-4.46072162768333));
#10551=CARTESIAN_POINT('Ctrl Pts',(3.7110948776815,1.16520593521907,-4.46118367431222));
#10552=CARTESIAN_POINT('Ctrl Pts',(3.72333194978885,1.16333036775391,-4.46201204362349));
#10553=CARTESIAN_POINT('Ctrl Pts',(3.72870968307208,1.16246790464474,-4.46237763259274));
#10554=CARTESIAN_POINT('Ctrl Pts',(3.74008315845333,1.16056285296851,-4.46315420382506));
#10555=CARTESIAN_POINT('Ctrl Pts',(3.74607717074026,1.15951103386453,-4.46356546531935));
#10556=CARTESIAN_POINT('Ctrl Pts',(3.76209856411653,1.15657145584035,-4.46467021137427));
#10557=CARTESIAN_POINT('Ctrl Pts',(3.77210982485208,1.15459979762217,-4.46536630540517));
#10558=CARTESIAN_POINT('Ctrl Pts',(3.81845848590619,1.14484445084483,-4.46861670435287));
#10559=CARTESIAN_POINT('Ctrl Pts',(3.85443657842567,1.13547455074788,-4.47122023140523));
#10560=CARTESIAN_POINT('Ctrl Pts',(3.97241210693093,1.0987112855891,-4.4800309491002));
#10561=CARTESIAN_POINT('Ctrl Pts',(4.05183033175571,1.06400050138129,-4.48643607373497));
#10562=CARTESIAN_POINT('Ctrl Pts',(4.15133465569593,1.00676845573574,-4.49479825325177));
#10563=CARTESIAN_POINT('Ctrl Pts',(4.17542621254354,0.991727459659717,-4.49684922187467));
#10564=CARTESIAN_POINT('Ctrl Pts',(4.21253583813431,0.966650013184072,-4.50002644874795));
#10565=CARTESIAN_POINT('Ctrl Pts',(4.22592734503419,0.957187319596748,-4.50117683386415));
#10566=CARTESIAN_POINT('Ctrl Pts',(4.24323420439615,0.944407872488963,-4.50266427535948));
#10567=CARTESIAN_POINT('Ctrl Pts',(4.24733095185915,0.941341363238803,-4.5030164231688));
#10568=CARTESIAN_POINT('Ctrl Pts',(4.25400534076225,0.936277221744721,-4.50359005184909));
#10569=CARTESIAN_POINT('Ctrl Pts',(4.2565948496467,0.934295453198158,-4.50381258463187));
#10570=CARTESIAN_POINT('Ctrl Pts',(4.26164698475302,0.930395642610353,-4.50424664910969));
#10571=CARTESIAN_POINT('Ctrl Pts',(4.26411026411439,0.928478528956926,-4.50445823753851));
#10572=CARTESIAN_POINT('Ctrl Pts',(4.26960959880018,0.924163309009259,-4.50493057557591));
#10573=CARTESIAN_POINT('Ctrl Pts',(4.27264154617054,0.921759967576544,-4.50519096350377));
#10574=CARTESIAN_POINT('Ctrl Pts',(4.28316075951896,0.913336939282048,-4.50609449601116));
#10575=CARTESIAN_POINT('Ctrl Pts',(4.29058641350802,0.907240423900407,-4.50673253875443));
#10576=CARTESIAN_POINT('Ctrl Pts',(4.35498557928602,0.853035563823585,-4.51227640933967));
#10577=CARTESIAN_POINT('Ctrl Pts',(4.40735353745325,0.79970107902609,-4.51686389823039));
#10578=CARTESIAN_POINT('Ctrl Pts',(4.48995908414947,0.697824443301773,-4.52497689603592));
#10579=CARTESIAN_POINT('Ctrl Pts',(4.52237310957322,0.651377358922156,-4.52847971136735));
#10580=CARTESIAN_POINT('Ctrl Pts',(4.56193708787925,0.584967081846571,-4.53341099384109));
#10581=CARTESIAN_POINT('Ctrl Pts',(4.57207810363457,0.566874638875244,-4.53474666413505));
#10582=CARTESIAN_POINT('Ctrl Pts',(4.5889255949637,0.53486379547339,-4.53710415560737));
#10583=CARTESIAN_POINT('Ctrl Pts',(4.59584582403614,0.521063419225569,-4.5381186986392));
#10584=CARTESIAN_POINT('Ctrl Pts',(4.6055693600665,0.500682392057368,-4.53961644974872));
#10585=CARTESIAN_POINT('Ctrl Pts',(4.60858734538229,0.494205521374071,-4.54009233081125));
#10586=CARTESIAN_POINT('Ctrl Pts',(4.61381234188122,0.482720349644697,-4.54093623518798));
#10587=CARTESIAN_POINT('Ctrl Pts',(4.61604375034683,0.477723330771751,-4.54130341896364));
#10588=CARTESIAN_POINT('Ctrl Pts',(4.62063829440744,0.467238633339539,-4.54207396180983));
#10589=CARTESIAN_POINT('Ctrl Pts',(4.62299465324799,0.461748173806508,-4.54247753647737));
#10590=CARTESIAN_POINT('Ctrl Pts',(4.62906485144233,0.447301919183366,-4.54353971388447));
#10591=CARTESIAN_POINT('Ctrl Pts',(4.6327099934989,0.438317934443671,-4.54420058445679));
#10592=CARTESIAN_POINT('Ctrl Pts',(4.64788967505092,0.399537801187319,-4.54705532862281));
#10593=CARTESIAN_POINT('Ctrl Pts',(4.65831906587027,0.369326530362815,-4.54928493984713));
#10594=CARTESIAN_POINT('Ctrl Pts',(4.69389293834458,0.250864131426148,-4.55805453238249));
#10595=CARTESIAN_POINT('Ctrl Pts',(4.70991929931431,0.160221840005983,-4.56485303807176));
#10596=CARTESIAN_POINT('Ctrl Pts',(4.71695580110238,0.0397220695454684,
-4.57365051969951));
#10597=CARTESIAN_POINT('Ctrl Pts',(4.71757685012782,0.0107326568825134,
-4.57574570900212));
#10598=CARTESIAN_POINT('Ctrl Pts',(4.71686996105628,-0.0348756478035519,
-4.5789826953634));
#10599=CARTESIAN_POINT('Ctrl Pts',(4.71626031493139,-0.0514931435986362,
-4.58014963543668));
#10600=CARTESIAN_POINT('Ctrl Pts',(4.71500161198726,-0.0732274486540218,
-4.58165498810216));
#10601=CARTESIAN_POINT('Ctrl Pts',(4.71467063568214,-0.07835984867642,-4.58200893541007));
#10602=CARTESIAN_POINT('Ctrl Pts',(4.71407448855711,-0.0867482258372043,
-4.58258474546325));
#10603=CARTESIAN_POINT('Ctrl Pts',(4.71382937740384,-0.0900054917435229,
-4.58280767506943));
#10604=CARTESIAN_POINT('Ctrl Pts',(4.71332385256295,-0.0963694330864966,
-4.58324188002917));
#10605=CARTESIAN_POINT('Ctrl Pts',(4.71306465099221,-0.0994761523842213,
-4.58345321605845));
#10606=CARTESIAN_POINT('Ctrl Pts',(4.71245740586505,-0.106421484809332,
-4.58392433265226));
#10607=CARTESIAN_POINT('Ctrl Pts',(4.7121028450712,-0.110259528669526,-4.58418375762949));
#10608=CARTESIAN_POINT('Ctrl Pts',(4.71080695372752,-0.123573400928585,
-4.585080711798));
#10609=CARTESIAN_POINT('Ctrl Pts',(4.70976952017576,-0.13303980612306,-4.58571323605646));
#10610=CARTESIAN_POINT('Ctrl Pts',(4.69946363467642,-0.21759551932588,-4.59132461838758));
#10611=CARTESIAN_POINT('Ctrl Pts',(4.68309297948722,-0.291652564604074,
-4.59597497668237));
#10612=CARTESIAN_POINT('Ctrl Pts',(4.64247351184896,-0.4167841101214,-4.60411315894722));
#10613=CARTESIAN_POINT('Ctrl Pts',(4.62146083832885,-0.468635108910132,
-4.60757532613088));
#10614=CARTESIAN_POINT('Ctrl Pts',(4.58777874691445,-0.537280779495973,
-4.61245439098281));
#10615=CARTESIAN_POINT('Ctrl Pts',(4.57822596268234,-0.555523990107598,
-4.61378084252605));
#10616=CARTESIAN_POINT('Ctrl Pts',(4.56072428660126,-0.586916207472989,
-4.61612352438308));
#10617=CARTESIAN_POINT('Ctrl Pts',(4.55298706445551,-0.600177738814442,
-4.61713260540244));
#10618=CARTESIAN_POINT('Ctrl Pts',(4.54128037417088,-0.619370768445844,
-4.618623786095));
#10619=CARTESIAN_POINT('Ctrl Pts',(4.53751250796105,-0.62542381912913,-4.61909865172497));
#10620=CARTESIAN_POINT('Ctrl Pts',(4.53075700789496,-0.63605998194878,-4.6199414027435));
#10621=CARTESIAN_POINT('Ctrl Pts',(4.52779193876714,-0.6406572292671,-4.62030845639633));
#10622=CARTESIAN_POINT('Ctrl Pts',(4.5215176569622,-0.650238098938151,-4.62107937750852));
#10623=CARTESIAN_POINT('Ctrl Pts',(4.51820229420364,-0.655217486505259,
-4.62148346493585));
#10624=CARTESIAN_POINT('Ctrl Pts',(4.50939568762503,-0.668228274093998,
-4.62254848076225));
#10625=CARTESIAN_POINT('Ctrl Pts',(4.50384270393942,-0.676217124235428,
-4.62321169918651));
#10626=CARTESIAN_POINT('Ctrl Pts',(4.47944814397458,-0.710400957820557,
-4.62609068114484));
#10627=CARTESIAN_POINT('Ctrl Pts',(4.45963503736907,-0.735882087728136,
-4.62834293907587));
#10628=CARTESIAN_POINT('Ctrl Pts',(4.38589359421848,-0.823078777287632,
-4.63644251929911));
#10629=CARTESIAN_POINT('Ctrl Pts',(4.32660521756055,-0.879943626302029,
-4.64248368260475));
#10630=CARTESIAN_POINT('Ctrl Pts',(4.22106376312065,-0.961907566959175,
-4.65226416754916));
#10631=CARTESIAN_POINT('Ctrl Pts',(4.17817032352177,-0.990906247482976,
-4.65601472483297));
#10632=CARTESIAN_POINT('Ctrl Pts',(4.12750443208351,-1.02049818102455,-4.66009558767205));
#10633=CARTESIAN_POINT('Ctrl Pts',(4.12147313663783,-1.02394960515021,-4.66057599720942));
#10634=CARTESIAN_POINT('Ctrl Pts',(4.11221961682113,-1.0291367805158,-4.66130449417721));
#10635=CARTESIAN_POINT('Ctrl Pts',(4.10901938995273,-1.03091115812828,-4.66155488756773));
#10636=CARTESIAN_POINT('Ctrl Pts',(4.10314398640771,-1.03413308873951,-4.66201169197118));
#10637=CARTESIAN_POINT('Ctrl Pts',(4.10047146243859,-1.0355851995795,-4.66221837792203));
#10638=CARTESIAN_POINT('Ctrl Pts',(4.09442338332127,-1.03884112878983,-4.66268366270804));
#10639=CARTESIAN_POINT('Ctrl Pts',(4.09104464166341,-1.04063885799809,-4.66294188247286));
#10640=CARTESIAN_POINT('Ctrl Pts',(4.08450203439169,-1.04407917172129,-4.66343872289608));
#10641=CARTESIAN_POINT('Ctrl Pts',(4.08133937867713,-1.04572391295231,-4.66367746909161));
#10642=CARTESIAN_POINT('Ctrl Pts',(4.07816926754726,-1.04735428871609,-4.66391540717654));
#10643=CARTESIAN_POINT('Origin',(3.53951905042299,8.32667268468867E-16,
0.924367114736157));
#10644=CARTESIAN_POINT('',(4.07816965980385,-1.04735408697996,-5.26199342056381));
#10645=CARTESIAN_POINT('',(4.07816923100673,-1.04735430750874,-5.16216634940201));
#10646=CARTESIAN_POINT('',(4.07816926754759,-1.04735428871592,0.924367114736157));
#10647=CARTESIAN_POINT('',(2.3617694621724,-0.000540025086465901,-4.92534712819671));
#10648=CARTESIAN_POINT('Ctrl Pts',(4.07816965980385,-1.04735408697996,-5.26199342056381));
#10649=CARTESIAN_POINT('Ctrl Pts',(4.12181072239703,-1.02490963839082,-5.25892790966009));
#10650=CARTESIAN_POINT('Ctrl Pts',(4.16404503060095,-0.999739693094997,
-5.25581515735499));
#10651=CARTESIAN_POINT('Ctrl Pts',(4.21653578388376,-0.963821510535766,
-5.25166303093834));
#10652=CARTESIAN_POINT('Ctrl Pts',(4.22830102561051,-0.955449068569838,
-5.25071292378843));
#10653=CARTESIAN_POINT('Ctrl Pts',(4.24550409185827,-0.942724041252379,
-5.24929282208923));
#10654=CARTESIAN_POINT('Ctrl Pts',(4.25106232125615,-0.938535916699573,
-5.24882909447093));
#10655=CARTESIAN_POINT('Ctrl Pts',(4.26090649012893,-0.930980626784435,
-5.2479988102137));
#10656=CARTESIAN_POINT('Ctrl Pts',(4.26520682443458,-0.927632480328237,
-5.24763299978676));
#10657=CARTESIAN_POINT('Ctrl Pts',(4.27424915135843,-0.920490964716445,
-5.24685711135079));
#10658=CARTESIAN_POINT('Ctrl Pts',(4.27898534000884,-0.916690537492991,
-5.24644676191384));
#10659=CARTESIAN_POINT('Ctrl Pts',(4.29155148404351,-0.906446417916009,
-5.24534725552976));
#10660=CARTESIAN_POINT('Ctrl Pts',(4.29932781777987,-0.899938062128318,
-5.24465553281595));
#10661=CARTESIAN_POINT('Ctrl Pts',(4.3383579916116,-0.866405498964806,-5.24112476558359));
#10662=CARTESIAN_POINT('Ctrl Pts',(4.36825486627107,-0.837853436406766,
-5.23822373770836));
#10663=CARTESIAN_POINT('Ctrl Pts',(4.46678938675016,-0.733308294601039,
-5.2279449652619));
#10664=CARTESIAN_POINT('Ctrl Pts',(4.52697344195916,-0.650001329079335,
-5.22028621760055));
#10665=CARTESIAN_POINT('Ctrl Pts',(4.58665020397976,-0.539581865519443,
-5.21129135290743));
#10666=CARTESIAN_POINT('Ctrl Pts',(4.59706661343969,-0.518869508816685,
-5.2096513520831));
#10667=CARTESIAN_POINT('Ctrl Pts',(4.60940106064836,-0.492426156105455,
-5.20762781222354));
#10668=CARTESIAN_POINT('Ctrl Pts',(4.61189493878861,-0.486971244410699,
-5.20721407088753));
#10669=CARTESIAN_POINT('Ctrl Pts',(4.61575977668403,-0.47834391561347,-5.20656577028571));
#10670=CARTESIAN_POINT('Ctrl Pts',(4.61715859028351,-0.475184201518537,
-5.20632960542054));
#10671=CARTESIAN_POINT('Ctrl Pts',(4.61977429803975,-0.469204745918405,
-5.20588514589748));
#10672=CARTESIAN_POINT('Ctrl Pts',(4.62099406123722,-0.466386422201719,
-5.20567669131505));
#10673=CARTESIAN_POINT('Ctrl Pts',(4.62382938100447,-0.459764338565198,
-5.2051892680157));
#10674=CARTESIAN_POINT('Ctrl Pts',(4.6254359592854,-0.455956805363756,-5.2049108348728));
#10675=CARTESIAN_POINT('Ctrl Pts',(4.63063246104493,-0.443458014576272,
-5.20400254454878));
#10676=CARTESIAN_POINT('Ctrl Pts',(4.63413845186622,-0.434731946387427,
-5.20337742073631));
#10677=CARTESIAN_POINT('Ctrl Pts',(4.65302503345263,-0.386047474049979,
-5.19993447420054));
#10678=CARTESIAN_POINT('Ctrl Pts',(4.66632395000198,-0.345311104233059,
-5.19721932173884));
#10679=CARTESIAN_POINT('Ctrl Pts',(4.68470474709112,-0.276498392960429,
-5.19276664346341));
#10680=CARTESIAN_POINT('Ctrl Pts',(4.69103918212133,-0.248803330221722,
-5.19100949129946));
#10681=CARTESIAN_POINT('Ctrl Pts',(4.71161889630559,-0.141030778264493,
-5.18422252239453));
#10682=CARTESIAN_POINT('Ctrl Pts',(4.71855660318823,-0.0598008844888874,
-5.17919608584553));
#10683=CARTESIAN_POINT('Ctrl Pts',(4.71679165907389,0.0369037688813997,
-5.17289241417119));
#10684=CARTESIAN_POINT('Ctrl Pts',(4.71620782193635,0.0523085313992264,
-5.17187931924319));
#10685=CARTESIAN_POINT('Ctrl Pts',(4.71491573126955,0.0747504037471623,
-5.17038835889738));
#10686=CARTESIAN_POINT('Ctrl Pts',(4.71444616733386,0.0818000398237494,
-5.1699178370322));
#10687=CARTESIAN_POINT('Ctrl Pts',(4.7134998992822,0.0943082614614065,-5.16907894154682));
#10688=CARTESIAN_POINT('Ctrl Pts',(4.71304847382315,0.0997685940210485,
-5.16871135976159));
#10689=CARTESIAN_POINT('Ctrl Pts',(4.71202671718992,0.11115900144885,-5.16794161908197));
#10690=CARTESIAN_POINT('Ctrl Pts',(4.71144945963075,0.117088282746944,-5.16753925548609));
#10691=CARTESIAN_POINT('Ctrl Pts',(4.70982325574268,0.132572731377017,-5.1664839664535));
#10692=CARTESIAN_POINT('Ctrl Pts',(4.70870228553757,0.142119721793125,-5.16582882729535));
#10693=CARTESIAN_POINT('Ctrl Pts',(4.70300572130557,0.185991816294285,-5.16279674980042));
#10694=CARTESIAN_POINT('Ctrl Pts',(4.69703495084384,0.220115206402822,-5.1603770833594));
#10695=CARTESIAN_POINT('Ctrl Pts',(4.67491572539615,0.320296060508006,-5.1530861452875));
#10696=CARTESIAN_POINT('Ctrl Pts',(4.65454413600666,0.385269186302499,-5.14810366116571));
#10697=CARTESIAN_POINT('Ctrl Pts',(4.61912076825343,0.471367557034039,-5.14127225520403));
#10698=CARTESIAN_POINT('Ctrl Pts',(4.60881180679766,0.494307902040265,-5.13942974161785));
#10699=CARTESIAN_POINT('Ctrl Pts',(4.59034790793633,0.532109237774679,-5.13637080484718));
#10700=CARTESIAN_POINT('Ctrl Pts',(4.58259232458584,0.547156025623537,-5.13514696889147));
#10701=CARTESIAN_POINT('Ctrl Pts',(4.56348996893813,0.582333550366112,-5.1322785551833));
#10702=CARTESIAN_POINT('Ctrl Pts',(4.55186918339786,0.602309044835768,-5.1306439375619));
#10703=CARTESIAN_POINT('Ctrl Pts',(4.53650348460343,0.627019136375058,-5.1286260273197));
#10704=CARTESIAN_POINT('Ctrl Pts',(4.53330075935997,0.632082967781581,-5.12821272777133));
#10705=CARTESIAN_POINT('Ctrl Pts',(4.52819092818517,0.640027273659789,-5.12756496140902));
#10706=CARTESIAN_POINT('Ctrl Pts',(4.52630960927651,0.642924090884075,-5.1273288932832));
#10707=CARTESIAN_POINT('Ctrl Pts',(4.5227313758944,0.648381075324588,-5.12688450712173));
#10708=CARTESIAN_POINT('Ctrl Pts',(4.52103720391257,0.650942862624202,-5.12667602997595));
#10709=CARTESIAN_POINT('Ctrl Pts',(4.51703851400971,0.656938246800565,-5.12618840839514));
#10710=CARTESIAN_POINT('Ctrl Pts',(4.51472590938022,0.660366372049791,-5.12590980088357));
#10711=CARTESIAN_POINT('Ctrl Pts',(4.50708709394372,0.671562244012291,-5.12500034459764));
#10712=CARTESIAN_POINT('Ctrl Pts',(4.50168559651082,0.679278527388979,-5.12437424598452));
#10713=CARTESIAN_POINT('Ctrl Pts',(4.47113727625992,0.721822558033856,-5.12092114835691));
#10714=CARTESIAN_POINT('Ctrl Pts',(4.44418948728184,0.755322808632546,-5.11819748398923));
#10715=CARTESIAN_POINT('Ctrl Pts',(4.39568850609399,0.809286419043412,-5.11366212219573));
#10716=CARTESIAN_POINT('Ctrl Pts',(4.375085813339,0.830541332681467,-5.11183225718775));
#10717=CARTESIAN_POINT('Ctrl Pts',(4.29597236301118,0.906232437590899,-5.10505978450021));
#10718=CARTESIAN_POINT('Ctrl Pts',(4.23277743782858,0.955442124826888,-5.10011581106505));
#10719=CARTESIAN_POINT('Ctrl Pts',(4.15199566313185,1.00608468363147,-5.09390234427455));
#10720=CARTESIAN_POINT('Ctrl Pts',(4.13873925710877,1.0140360445229,-5.09288651473095));
#10721=CARTESIAN_POINT('Ctrl Pts',(4.11919478559555,1.02524198637415,-5.09139227222458));
#10722=CARTESIAN_POINT('Ctrl Pts',(4.11302742834247,1.02870463466391,-5.0909212496014));
#10723=CARTESIAN_POINT('Ctrl Pts',(4.10202692900307,1.03475116840081,-5.09008177993314));
#10724=CARTESIAN_POINT('Ctrl Pts',(4.09720619585746,1.03735728659822,-5.08971412849348));
#10725=CARTESIAN_POINT('Ctrl Pts',(4.08711050211186,1.04272436978215,-5.08894456617716));
#10726=CARTESIAN_POINT('Ctrl Pts',(4.08183245418757,1.04547916246757,-5.08854245276601));
#10727=CARTESIAN_POINT('Ctrl Pts',(4.06799348499323,1.05256919786595,-5.0874885492809));
#10728=CARTESIAN_POINT('Ctrl Pts',(4.05940021302137,1.05683996499785,-5.08683455619067));
#10729=CARTESIAN_POINT('Ctrl Pts',(4.01972822894387,1.07595559461547,-5.08381651801301));
#10730=CARTESIAN_POINT('Ctrl Pts',(3.98806270602655,1.08953635420821,-5.08141023025321));
#10731=CARTESIAN_POINT('Ctrl Pts',(3.89290739331601,1.12549514686094,-5.07418262163846));
#10732=CARTESIAN_POINT('Ctrl Pts',(3.82804800739374,1.14384082649897,-5.06925257873283));
#10733=CARTESIAN_POINT('Ctrl Pts',(3.7036443792427,1.1677703374829,-5.05995623275433));
#10734=CARTESIAN_POINT('Ctrl Pts',(3.64453169197281,1.17456308823098,-5.05560708651603));
#10735=CARTESIAN_POINT('Ctrl Pts',(3.57514463852517,1.17725367404128,-5.05073772466424));
#10736=CARTESIAN_POINT('Ctrl Pts',(3.56513055737188,1.17751410304252,-5.05004079967255));
#10737=CARTESIAN_POINT('Ctrl Pts',(3.55117601957179,1.17769889518903,-5.04907884791963));
#10738=CARTESIAN_POINT('Ctrl Pts',(3.54723776306123,1.17773129161456,-5.04880838697305));
#10739=CARTESIAN_POINT('Ctrl Pts',(3.540442403854,1.17775310321496,-5.04834355983019));
#10740=CARTESIAN_POINT('Ctrl Pts',(3.53758539678206,1.17775187800398,-5.04814869325288));
#10741=CARTESIAN_POINT('Ctrl Pts',(3.53155650614656,1.17772735442585,-5.04773871102051));
#10742=CARTESIAN_POINT('Ctrl Pts',(3.52838466048035,1.1777016384777,-5.04752373595874));
#10743=CARTESIAN_POINT('Ctrl Pts',(3.52051163681021,1.17760599780551,-5.04699183561268));
#10744=CARTESIAN_POINT('Ctrl Pts',(3.51581063687405,1.17752073477916,-5.04667574276497));
#10745=CARTESIAN_POINT('Ctrl Pts',(3.49806462841056,1.17709255317963,-5.04548777109785));
#10746=CARTESIAN_POINT('Ctrl Pts',(3.48502454462631,1.17656097652151,-5.0446255618208));
#10747=CARTESIAN_POINT('Ctrl Pts',(3.45153696241877,1.17463787613255,-5.04243279189006));
#10748=CARTESIAN_POINT('Ctrl Pts',(3.43111149806204,1.17292919227403,-5.04111588118099));
#10749=CARTESIAN_POINT('Ctrl Pts',(3.35327263201899,1.16436668618449,-5.03614110683995));
#10750=CARTESIAN_POINT('Ctrl Pts',(3.29634548165766,1.15382187783944,-5.03259116118402));
#10751=CARTESIAN_POINT('Ctrl Pts',(3.16743493356829,1.11997436303171,-5.02433857426702));
#10752=CARTESIAN_POINT('Ctrl Pts',(3.09647047652549,1.09384410115273,-5.0196258414921));
#10753=CARTESIAN_POINT('Ctrl Pts',(3.01913711947947,1.05660098896032,-5.0139925152941));
#10754=CARTESIAN_POINT('Ctrl Pts',(3.00983689102419,1.05196948755356,-5.01330667541189));
#10755=CARTESIAN_POINT('Ctrl Pts',(2.99461953520751,1.04413830961879,-5.01216995053619));
#10756=CARTESIAN_POINT('Ctrl Pts',(2.98866625697952,1.04100984054052,-5.01172152542976));
#10757=CARTESIAN_POINT('Ctrl Pts',(2.97818577263532,1.03538723511854,-5.01092532310437));
#10758=CARTESIAN_POINT('Ctrl Pts',(2.97364754066414,1.03291394045555,-5.01057828259718));
#10759=CARTESIAN_POINT('Ctrl Pts',(2.96388529930138,1.02750996357235,-5.00982676111007));
#10760=CARTESIAN_POINT('Ctrl Pts',(2.9586670943763,1.02456915019964,-5.00942192931476));
#10761=CARTESIAN_POINT('Ctrl Pts',(2.94798962802038,1.01844388514554,-5.00858702203782));
#10762=CARTESIAN_POINT('Ctrl Pts',(2.9425331218931,1.01525504342289,-5.00815679950824));
#10763=CARTESIAN_POINT('Ctrl Pts',(2.92896179358082,1.00717657580366,-5.00707770216163));
#10764=CARTESIAN_POINT('Ctrl Pts',(2.92087993178016,1.00223273272737,-5.00642690454264));
#10765=CARTESIAN_POINT('Ctrl Pts',(2.89813458345643,0.987938990756681,-5.00457161794335));
#10766=CARTESIAN_POINT('Ctrl Pts',(2.88361782231235,0.978361389566877,-5.00335910521856));
#10767=CARTESIAN_POINT('Ctrl Pts',(2.83441198463984,0.944309867614952,-4.99914917682155));
#10768=CARTESIAN_POINT('Ctrl Pts',(2.8008398717433,0.918286191794954,-4.99609953176539));
#10769=CARTESIAN_POINT('Ctrl Pts',(2.72189126543553,0.849953113278,-4.98850243575755));
#10770=CARTESIAN_POINT('Ctrl Pts',(2.67830960434367,0.805762713450463,-4.98391948335111));
#10771=CARTESIAN_POINT('Ctrl Pts',(2.62935760230804,0.747595313268514,-4.97839474099661));
#10772=CARTESIAN_POINT('Ctrl Pts',(2.62050038630224,0.736679939528711,-4.97737817840808));
#10773=CARTESIAN_POINT('Ctrl Pts',(2.59652165156743,0.706023510672077,-4.97458328105213));
#10774=CARTESIAN_POINT('Ctrl Pts',(2.58182558212455,0.685956792730309,-4.97282080439739));
#10775=CARTESIAN_POINT('Ctrl Pts',(2.56434953644656,0.660436394917194,-4.97067482939049));
#10776=CARTESIAN_POINT('Ctrl Pts',(2.56096292456356,0.655408060055201,-4.97025647199444));
#10777=CARTESIAN_POINT('Ctrl Pts',(2.55567984455888,0.647431666814539,-4.96960012831129));
#10778=CARTESIAN_POINT('Ctrl Pts',(2.55375750923817,0.644500993729968,-4.96936051204091));
#10779=CARTESIAN_POINT('Ctrl Pts',(2.55034861433473,0.639253071728064,-4.96893423068016));
#10780=CARTESIAN_POINT('Ctrl Pts',(2.54885709992483,0.63693919757697,-4.96874724725859));
#10781=CARTESIAN_POINT('Ctrl Pts',(2.54528799277041,0.631359365591405,-4.96829864277084));
#10782=CARTESIAN_POINT('Ctrl Pts',(2.54321837120998,0.628088371321061,-4.9680375421102));
#10783=CARTESIAN_POINT('Ctrl Pts',(2.53692426249731,0.618031268978648,-4.9672403027451));
#10784=CARTESIAN_POINT('Ctrl Pts',(2.53275259825284,0.61121213796607,-4.96670743786144));
#10785=CARTESIAN_POINT('Ctrl Pts',(2.52317564995829,0.595193238280242,-4.96547224342799));
#10786=CARTESIAN_POINT('Ctrl Pts',(2.51782523327688,0.585961312822027,-4.96477294320863));
#10787=CARTESIAN_POINT('Ctrl Pts',(2.4993872981812,0.553126833967579,-4.96232515490447));
#10788=CARTESIAN_POINT('Ctrl Pts',(2.48698554113814,0.529147206672973,-4.96060819549297));
#10789=CARTESIAN_POINT('Ctrl Pts',(2.43299941665534,0.415337533251348,-4.95268731264139));
#10790=CARTESIAN_POINT('Ctrl Pts',(2.40202262557602,0.320926229393458,-4.9467268254807));
#10791=CARTESIAN_POINT('Ctrl Pts',(2.37780790036989,0.195789132497261,-4.93857492600095));
#10792=CARTESIAN_POINT('Ctrl Pts',(2.37341359649751,0.167642610946875,-4.93672864877239));
#10793=CARTESIAN_POINT('Ctrl Pts',(2.36894287836191,0.130127094051754,-4.93423722545964));
#10794=CARTESIAN_POINT('Ctrl Pts',(2.36795141062971,0.120875524460372,-4.93362040694766));
#10795=CARTESIAN_POINT('Ctrl Pts',(2.36651146449389,0.10574952665702,-4.93260754936065));
#10796=CARTESIAN_POINT('Ctrl Pts',(2.36599725113855,0.0998816474920488,
-4.9322135551601));
#10797=CARTESIAN_POINT('Ctrl Pts',(2.36511081596282,0.0888119204264973,
-4.93146815585098));
#10798=CARTESIAN_POINT('Ctrl Pts',(2.36472908438211,0.0836109596068005,
-4.93111705473318));
#10799=CARTESIAN_POINT('Ctrl Pts',(2.36402603852109,0.0730740450178941,
-4.93040387614608));
#10800=CARTESIAN_POINT('Ctrl Pts',(2.36370648662251,0.0677381005423877,
-4.93004175260206));
#10801=CARTESIAN_POINT('Ctrl Pts',(2.36293200124268,0.0531408975087039,
-4.92904838308185));
#10802=CARTESIAN_POINT('Ctrl Pts',(2.36255010438768,0.0438763128627383,
-4.92841490227299));
#10803=CARTESIAN_POINT('Ctrl Pts',(2.3619332874832,0.0228946380504665,-4.92697314292768));
#10804=CARTESIAN_POINT('Ctrl Pts',(2.36176379052719,0.011176820686237,-4.92616293648505));
#10805=CARTESIAN_POINT('Ctrl Pts',(2.36176917474948,-0.000541157121145007,
-4.92534754912936));
#10806=CARTESIAN_POINT('Ctrl Pts',(2.3617691742458,-0.000540059816761217,
-4.92534762548451));
#10807=CARTESIAN_POINT('Ctrl Pts',(2.36181898604999,-0.1091684828109,-4.91778879502375));
#10808=CARTESIAN_POINT('Ctrl Pts',(2.3768982642571,-0.21725951079595,-4.90975117149892));
#10809=CARTESIAN_POINT('Ctrl Pts',(2.41479228157621,-0.350702095365063,
-4.89963175039954));
#10810=CARTESIAN_POINT('Ctrl Pts',(2.42412918804696,-0.379352030733392,
-4.89745194885264));
#10811=CARTESIAN_POINT('Ctrl Pts',(2.44045962029353,-0.423620709524443,
-4.8941011523857));
#10812=CARTESIAN_POINT('Ctrl Pts',(2.44671182077197,-0.439498089175984,
-4.89290302787093));
#10813=CARTESIAN_POINT('Ctrl Pts',(2.45531365661753,-0.46002246942175,-4.89136398367663));
#10814=CARTESIAN_POINT('Ctrl Pts',(2.45735178281537,-0.464796746716891,
-4.89100667874334));
#10815=CARTESIAN_POINT('Ctrl Pts',(2.46072808667034,-0.472563074918726,
-4.89042677503478));
#10816=CARTESIAN_POINT('Ctrl Pts',(2.46204727782729,-0.475563227319261,
-4.89020308145298));
#10817=CARTESIAN_POINT('Ctrl Pts',(2.46464316677656,-0.481400640495505,
-4.88976852858433));
#10818=CARTESIAN_POINT('Ctrl Pts',(2.46591860598063,-0.484238399890764,
-4.88955760145916));
#10819=CARTESIAN_POINT('Ctrl Pts',(2.46908867480344,-0.491217480424574,
-4.88903957602262));
#10820=CARTESIAN_POINT('Ctrl Pts',(2.47099613475291,-0.495352987793376,
-4.88873324326063));
#10821=CARTESIAN_POINT('Ctrl Pts',(2.4765980270547,-0.507315351744546,-4.88784867206811));
#10822=CARTESIAN_POINT('Ctrl Pts',(2.48035489525971,-0.515112872116006,
-4.88727398096347));
#10823=CARTESIAN_POINT('Ctrl Pts',(2.51915839094289,-0.59343115205462,-4.88151403766226));
#10824=CARTESIAN_POINT('Ctrl Pts',(2.56111356399941,-0.660320194402181,
-4.87668683277672));
#10825=CARTESIAN_POINT('Ctrl Pts',(2.65186312867384,-0.777138526529026,
-4.86753387797304));
#10826=CARTESIAN_POINT('Ctrl Pts',(2.69901022010504,-0.827901417128617,
-4.86323554845166));
#10827=CARTESIAN_POINT('Ctrl Pts',(2.75967865557678,-0.882667821003851,
-4.85793415668721));
#10828=CARTESIAN_POINT('Ctrl Pts',(2.76915705345247,-0.890952242532075,
-4.85711216872654));
#10829=CARTESIAN_POINT('Ctrl Pts',(2.78456444155176,-0.903989099496904,
-4.85578457188405));
#10830=CARTESIAN_POINT('Ctrl Pts',(2.79040995131818,-0.908838988332221,
-4.85528280811798));
#10831=CARTESIAN_POINT('Ctrl Pts',(2.80153794472927,-0.917891338641795,
-4.85433091741403));
#10832=CARTESIAN_POINT('Ctrl Pts',(2.80681046243589,-0.922105603404551,
-4.85388127793458));
#10833=CARTESIAN_POINT('Ctrl Pts',(2.81217361515792,-0.926317270244198,
-4.85342519085826));
#10834=CARTESIAN_POINT('Ctrl Pts',(2.81222841116074,-0.926360293511715,
-4.85342053109387));
#10835=CARTESIAN_POINT('Ctrl Pts',(2.81234195190683,-0.926449424129804,
-4.8534108760487));
#10836=CARTESIAN_POINT('Ctrl Pts',(2.81240069721753,-0.926495530754796,
-4.85340588073968));
#10837=CARTESIAN_POINT('Ctrl Pts',(2.81252257883423,-0.92659117157316,-4.85339551706046));
#10838=CARTESIAN_POINT('Ctrl Pts',(2.81258571581292,-0.926640704897272,
-4.85339014865691));
#10839=CARTESIAN_POINT('Ctrl Pts',(2.81271689344659,-0.926743597005745,
-4.85337899527));
#10840=CARTESIAN_POINT('Ctrl Pts',(2.81278493491908,-0.926796954752999,
-4.85337321024575));
#10841=CARTESIAN_POINT('Ctrl Pts',(2.81292651962749,-0.926907959521318,
-4.85336117285522));
#10842=CARTESIAN_POINT('Ctrl Pts',(2.81300006384146,-0.92696560527795,-4.8533549204404));
#10843=CARTESIAN_POINT('Ctrl Pts',(2.81315335640737,-0.92708573029719,-4.85334188866281));
#10844=CARTESIAN_POINT('Ctrl Pts',(2.81323310596572,-0.927148208026781,
-4.85333510923968));
#10845=CARTESIAN_POINT('Ctrl Pts',(2.81339964028152,-0.927278640358562,
-4.85332095292847));
#10846=CARTESIAN_POINT('Ctrl Pts',(2.8134864265113,-0.927346593062875,-4.85331357596712));
#10847=CARTESIAN_POINT('Ctrl Pts',(2.81366802544857,-0.927488742000743,
-4.85329814048013));
#10848=CARTESIAN_POINT('Ctrl Pts',(2.81376283999231,-0.927562935878647,
-4.85329008186285));
#10849=CARTESIAN_POINT('Ctrl Pts',(2.81396168866049,-0.927718488947303,
-4.85327318185809));
#10850=CARTESIAN_POINT('Ctrl Pts',(2.81406572508664,-0.927799845171807,
-4.85326434035588));
#10851=CARTESIAN_POINT('Ctrl Pts',(2.81428446787926,-0.927970842201228,
-4.85324575157455));
#10852=CARTESIAN_POINT('Ctrl Pts',(2.81439917718112,-0.928060479237587,
-4.85323600414871));
#10853=CARTESIAN_POINT('Ctrl Pts',(2.81464104860361,-0.928249412069959,
-4.85321545234029));
#10854=CARTESIAN_POINT('Ctrl Pts',(2.81476821450138,-0.928348702999451,
-4.85320464776902));
#10855=CARTESIAN_POINT('Ctrl Pts',(2.81503721832761,-0.928558651796912,
-4.85318179352913));
#10856=CARTESIAN_POINT('Ctrl Pts',(2.8151790612019,-0.928669303292786,-4.85316974361315));
#10857=CARTESIAN_POINT('Ctrl Pts',(2.81548022081617,-0.928904126657907,
-4.8531441612025));
#10858=CARTESIAN_POINT('Ctrl Pts',(2.81563954414395,-0.929028290037307,
-4.85313062837795));
#10859=CARTESIAN_POINT('Ctrl Pts',(2.81597925999633,-0.929292895934835,
-4.8531017754874));
#10860=CARTESIAN_POINT('Ctrl Pts',(2.81615966146351,-0.92943332690928,-4.85308645497331));
#10861=CARTESIAN_POINT('Ctrl Pts',(2.81642629426616,-0.929640758797993,
-4.853063813394));
#10862=CARTESIAN_POINT('Ctrl Pts',(2.81651249413298,-0.929707800325802,
-4.85305649390827));
#10863=CARTESIAN_POINT('Ctrl Pts',(2.81678542558222,-0.929920010520886,
-4.8530333195128));
#10864=CARTESIAN_POINT('Ctrl Pts',(2.8169721914822,-0.930065134857392,-4.85301746287995));
#10865=CARTESIAN_POINT('Ctrl Pts',(2.82133725349274,-0.933454848709381,
-4.8526468995239));
#10866=CARTESIAN_POINT('Ctrl Pts',(2.82553726016308,-0.93667126017307,-4.85229110269391));
#10867=CARTESIAN_POINT('Ctrl Pts',(2.83512969130231,-0.943915246063989,
-4.85148011500952));
#10868=CARTESIAN_POINT('Ctrl Pts',(2.84053521770156,-0.947925081078398,
-4.85102425483084));
#10869=CARTESIAN_POINT('Ctrl Pts',(2.85438557342324,-0.95801642871208,-4.84985895889958));
#10870=CARTESIAN_POINT('Ctrl Pts',(2.86287703639412,-0.964032640419206,
-4.84914708093828));
#10871=CARTESIAN_POINT('Ctrl Pts',(2.93360151719623,-1.01274625456824,-4.84323727408815));
#10872=CARTESIAN_POINT('Ctrl Pts',(2.99971556311497,-1.04947574867174,-4.83781768434997));
#10873=CARTESIAN_POINT('Ctrl Pts',(3.12194767035934,-1.10276067581353,-4.82806332631947));
#10874=CARTESIAN_POINT('Ctrl Pts',(3.17665399657629,-1.12195194797886,-4.8237872403041));
#10875=CARTESIAN_POINT('Ctrl Pts',(3.25226223265107,-1.1423639737446,-4.81813256979602));
#10876=CARTESIAN_POINT('Ctrl Pts',(3.27211006870983,-1.14717237723388,-4.81667168507945));
#10877=CARTESIAN_POINT('Ctrl Pts',(3.30479848613688,-1.15419699747518,-4.81431386124434));
#10878=CARTESIAN_POINT('Ctrl Pts',(3.3175680978176,-1.1567204770445,-4.81340468577313));
#10879=CARTESIAN_POINT('Ctrl Pts',(3.33499980239412,-1.15986594073542,-4.81218202566516));
#10880=CARTESIAN_POINT('Ctrl Pts',(3.33962709298689,-1.16067236140287,-4.81185922793262));
#10881=CARTESIAN_POINT('Ctrl Pts',(3.3473862022155,-1.16197680087145,-4.81132103954564));
#10882=CARTESIAN_POINT('Ctrl Pts',(3.35051539252966,-1.16248988606737,-4.81110483047383));
#10883=CARTESIAN_POINT('Ctrl Pts',(3.3564686906733,-1.16344135884289,-4.81069513219727));
#10884=CARTESIAN_POINT('Ctrl Pts',(3.3592923729147,-1.16388211380205,-4.8105015081195));
#10885=CARTESIAN_POINT('Ctrl Pts',(3.36601440233178,-1.16490632096715,-4.81004216838426));
#10886=CARTESIAN_POINT('Ctrl Pts',(3.36991416040227,-1.16548049401373,-4.80977696265404));
#10887=CARTESIAN_POINT('Ctrl Pts',(3.38375419949886,-1.16744726644796,-4.80884005592069));
#10888=CARTESIAN_POINT('Ctrl Pts',(3.39370965490633,-1.16873240962715,-4.80817396338375));
#10889=CARTESIAN_POINT('Ctrl Pts',(3.46327460914987,-1.17680973789604,-4.80356656716596));
#10890=CARTESIAN_POINT('Ctrl Pts',(3.52331819541534,-1.17916655427905,-4.799827506927));
#10891=CARTESIAN_POINT('Ctrl Pts',(3.65005907296692,-1.17445336707883,-4.79196989567312));
#10892=CARTESIAN_POINT('Ctrl Pts',(3.71649539435003,-1.16629266550261,-4.78786703465103));
#10893=CARTESIAN_POINT('Ctrl Pts',(3.81545848963402,-1.14548238035953,-4.78143785346733));
#10894=CARTESIAN_POINT('Ctrl Pts',(3.84870985800779,-1.13695785148989,-4.77922304202997));
#10895=CARTESIAN_POINT('Ctrl Pts',(3.89071094569065,-1.12421135815636,-4.77633045465986));
#10896=CARTESIAN_POINT('Ctrl Pts',(3.89984785013332,-1.12131622314379,-4.77569538513455));
#10897=CARTESIAN_POINT('Ctrl Pts',(3.91459906501985,-1.11644321948396,-4.77466014454029));
#10898=CARTESIAN_POINT('Ctrl Pts',(3.92023562499971,-1.1145336995018,-4.77426219702932));
#10899=CARTESIAN_POINT('Ctrl Pts',(3.93103499238363,-1.11078367369686,-4.7734950626842));
#10900=CARTESIAN_POINT('Ctrl Pts',(3.93619991026364,-1.10894968157025,-4.77312609727508));
#10901=CARTESIAN_POINT('Ctrl Pts',(3.94800527484999,-1.10466473120827,-4.77227789947044));
#10902=CARTESIAN_POINT('Ctrl Pts',(3.95463674959023,-1.10218984570484,-4.77179789100892));
#10903=CARTESIAN_POINT('Ctrl Pts',(3.97570533521537,-1.09410988024924,-4.77026129596531));
#10904=CARTESIAN_POINT('Ctrl Pts',(3.99005386349495,-1.08827994916449,-4.76919734025277));
#10905=CARTESIAN_POINT('Ctrl Pts',(4.02932237438677,-1.07141513801035,-4.76623557462156));
#10906=CARTESIAN_POINT('Ctrl Pts',(4.05396561751214,-1.05980213712042,-4.76432014601751));
#10907=CARTESIAN_POINT('Ctrl Pts',(4.07816946571175,-1.04735418680084,-4.76238152739268));
#10908=CARTESIAN_POINT('Ctrl Pts',(4.07816926754726,-1.04735428871609,-4.66391540717654));
#10909=CARTESIAN_POINT('Ctrl Pts',(4.07594237517118,-1.04849957076134,-4.66408255037298));
#10910=CARTESIAN_POINT('Ctrl Pts',(4.07371180386683,-1.04963776406353,-4.66424929480144));
#10911=CARTESIAN_POINT('Ctrl Pts',(4.04042211211563,-1.06649088614516,-4.66672805048002));
#10912=CARTESIAN_POINT('Ctrl Pts',(4.0086815204711,-1.08083013267527,-4.66896494141043));
#10913=CARTESIAN_POINT('Ctrl Pts',(3.95009147986544,-1.10423040334051,-4.67295075052231));
#10914=CARTESIAN_POINT('Ctrl Pts',(3.92346369370455,-1.11376888769826,-4.6747110445444));
#10915=CARTESIAN_POINT('Ctrl Pts',(3.83337807483642,-1.14242368521899,-4.68057183162995));
#10916=CARTESIAN_POINT('Ctrl Pts',(3.76865968539658,-1.15714263997218,-4.68463580821676));
#10917=CARTESIAN_POINT('Ctrl Pts',(3.66663614832824,-1.17144706502294,-4.69116873956656));
#10918=CARTESIAN_POINT('Ctrl Pts',(3.63000799642946,-1.17484395378423,-4.69353720779345));
#10919=CARTESIAN_POINT('Ctrl Pts',(3.58349994369115,-1.17696926980004,-4.69660390671092));
#10920=CARTESIAN_POINT('Ctrl Pts',(3.57371140871894,-1.17729429377407,-4.69725261074648));
#10921=CARTESIAN_POINT('Ctrl Pts',(3.55792522256068,-1.17762142918079,-4.69830454967573));
#10922=CARTESIAN_POINT('Ctrl Pts',(3.55192948374963,-1.17769987540759,-4.69870542348624));
#10923=CARTESIAN_POINT('Ctrl Pts',(3.54046693973192,-1.17776230546359,-4.69947448198897));
#10924=CARTESIAN_POINT('Ctrl Pts',(3.53500031929333,-1.17775401761402,-4.69984241798241));
#10925=CARTESIAN_POINT('Ctrl Pts',(3.52255137258316,-1.17764847108797,-4.70068304766807));
#10926=CARTESIAN_POINT('Ctrl Pts',(3.51556951052194,-1.17752717142828,-4.70115647112397));
#10927=CARTESIAN_POINT('Ctrl Pts',(3.49362664586136,-1.17695071446321,-4.70265076676722));
#10928=CARTESIAN_POINT('Ctrl Pts',(3.47867350584121,-1.17627245187627,-4.70367844800702));
#10929=CARTESIAN_POINT('Ctrl Pts',(3.37381403098154,-1.16951136556598,-4.71095425256885));
#10930=CARTESIAN_POINT('Ctrl Pts',(3.28486878464908,-1.15341330796791,-4.71751751035369));
#10931=CARTESIAN_POINT('Ctrl Pts',(3.13648430369497,-1.10854656736093,-4.7288945734192));
#10932=CARTESIAN_POINT('Ctrl Pts',(3.07597624575129,-1.08463928832256,-4.7336563320011));
#10933=CARTESIAN_POINT('Ctrl Pts',(3.01038139189544,-1.0522242280023,-4.73876251140944));
#10934=CARTESIAN_POINT('Ctrl Pts',(3.00305789832098,-1.04850938449694,-4.73933167849372));
#10935=CARTESIAN_POINT('Ctrl Pts',(2.99230306569419,-1.04291180642469,-4.74016551164074));
#10936=CARTESIAN_POINT('Ctrl Pts',(2.98884148492761,-1.04108817584861,-4.74043358055913));
#10937=CARTESIAN_POINT('Ctrl Pts',(2.982700608023,-1.03781384020369,-4.74090849801768));
#10938=CARTESIAN_POINT('Ctrl Pts',(2.98001778785014,-1.03636995451515,-4.74111575597655));
#10939=CARTESIAN_POINT('Ctrl Pts',(2.97418454116829,-1.03320126512422,-4.74156589831628));
#10940=CARTESIAN_POINT('Ctrl Pts',(2.97103638544072,-1.03147245338185,-4.7418085289892));
#10941=CARTESIAN_POINT('Ctrl Pts',(2.96226074820748,-1.0266009248748,-4.74248415282486));
#10942=CARTESIAN_POINT('Ctrl Pts',(2.95665097989623,-1.02342631557843,-4.74291520800155));
#10943=CARTESIAN_POINT('Ctrl Pts',(2.92427927831815,-1.00475441370576,-4.74539948592566));
#10944=CARTESIAN_POINT('Ctrl Pts',(2.89810743256667,-0.988252457315542,
-4.74739543981475));
#10945=CARTESIAN_POINT('Ctrl Pts',(2.81874821178269,-0.933731936282084,
-4.75350587934091));
#10946=CARTESIAN_POINT('Ctrl Pts',(2.76805383453747,-0.892305073729162,
-4.75750011858764));
#10947=CARTESIAN_POINT('Ctrl Pts',(2.68017429558994,-0.807374732461095,
-4.76508590753014));
#10948=CARTESIAN_POINT('Ctrl Pts',(2.64221148736273,-0.764961088451493,
-4.76865181562321));
#10949=CARTESIAN_POINT('Ctrl Pts',(2.59639385165059,-0.705647021776681,
-4.77351572210995));
#10950=CARTESIAN_POINT('Ctrl Pts',(2.58565828138658,-0.691066159061978,
-4.77470201729709));
#10951=CARTESIAN_POINT('Ctrl Pts',(2.57089487314005,-0.670015039881867,
-4.77640499125867));
#10952=CARTESIAN_POINT('Ctrl Pts',(2.56658680154747,-0.663743764608143,
-4.77691111934945));
#10953=CARTESIAN_POINT('Ctrl Pts',(2.55924430036471,-0.652830169326876,
-4.77779008900089));
#10954=CARTESIAN_POINT('Ctrl Pts',(2.55618130525719,-0.648207291479624,
-4.77816185457187));
#10955=CARTESIAN_POINT('Ctrl Pts',(2.55036007655923,-0.639285285181651,
-4.77887837605372));
#10956=CARTESIAN_POINT('Ctrl Pts',(2.54759693251548,-0.634989497563756,
-4.77922294012964));
#10957=CARTESIAN_POINT('Ctrl Pts',(2.5411411174682,-0.62480784549932,-4.78003867619195));
#10958=CARTESIAN_POINT('Ctrl Pts',(2.53747245154041,-0.618907061594607,
-4.78051070968078));
#10959=CARTESIAN_POINT('Ctrl Pts',(2.52665496992359,-0.60115959798838,-4.78192845602149));
#10960=CARTESIAN_POINT('Ctrl Pts',(2.51966269772991,-0.589219398436419,
-4.78287971914512));
#10961=CARTESIAN_POINT('Ctrl Pts',(2.4722993367599,-0.504970634263997,-4.78957636750384));
#10962=CARTESIAN_POINT('Ctrl Pts',(2.43945026368169,-0.42871575861482,-4.79558411563196));
#10963=CARTESIAN_POINT('Ctrl Pts',(2.40738734594908,-0.325589333328425,
-4.80350798074462));
#10964=CARTESIAN_POINT('Ctrl Pts',(2.40067753052457,-0.301281637022407,
-4.80535980599111));
#10965=CARTESIAN_POINT('Ctrl Pts',(2.38432607889428,-0.233651103097251,
-4.81044600652398));
#10966=CARTESIAN_POINT('Ctrl Pts',(2.376343426479,-0.189965581231032,-4.81365869338497));
#10967=CARTESIAN_POINT('Ctrl Pts',(2.36965958782558,-0.136438239716641,
-4.81743560495512));
#10968=CARTESIAN_POINT('Ctrl Pts',(2.36859003216975,-0.126932282345681,
-4.81810024147724));
#10969=CARTESIAN_POINT('Ctrl Pts',(2.36722159069247,-0.11327417371505,-4.8190454584071));
#10970=CARTESIAN_POINT('Ctrl Pts',(2.36682874431602,-0.109132120882722,
-4.81933083023163));
#10971=CARTESIAN_POINT('Ctrl Pts',(2.36618378468905,-0.101925800603485,
-4.81982499208126));
#10972=CARTESIAN_POINT('Ctrl Pts',(2.36592170833022,-0.0988625013259678,
-4.8200343200167));
#10973=CARTESIAN_POINT('Ctrl Pts',(2.36539180889145,-0.092369459952888,
-4.82047643419576));
#10974=CARTESIAN_POINT('Ctrl Pts',(2.36512701428202,-0.0889395449169065,
-4.82070905396838));
#10975=CARTESIAN_POINT('Ctrl Pts',(2.36444676922117,-0.079594922763808,
-4.82134041675857));
#10976=CARTESIAN_POINT('Ctrl Pts',(2.36406094202169,-0.0736780619804741,
-4.82173757126383));
#10977=CARTESIAN_POINT('Ctrl Pts',(2.36243157575517,-0.0454039588929165,
-4.82362400025371));
#10978=CARTESIAN_POINT('Ctrl Pts',(2.36178101448085,-0.0230155722425881,
-4.82508373987338));
#10979=CARTESIAN_POINT('Ctrl Pts',(2.36174401658426,0.0471985237747278,
-4.829593103011));
#10980=CARTESIAN_POINT('Ctrl Pts',(2.3646311847031,0.0949786277497044,-4.83256307013559));
#10981=CARTESIAN_POINT('Ctrl Pts',(2.3811127466578,0.230240856367583,-4.8409985176109));
#10982=CARTESIAN_POINT('Ctrl Pts',(2.40166106301473,0.316532919826317,-4.84643564789581));
#10983=CARTESIAN_POINT('Ctrl Pts',(2.43679006200633,0.413897779696194,-4.85318542095783));
#10984=CARTESIAN_POINT('Ctrl Pts',(2.44218128664968,0.427986439667305,-4.85417716662488));
#10985=CARTESIAN_POINT('Ctrl Pts',(2.45046987214241,0.448459597062111,-4.85564243623371));
#10986=CARTESIAN_POINT('Ctrl Pts',(2.45315615543315,0.454928323754113,-4.85610897651905));
#10987=CARTESIAN_POINT('Ctrl Pts',(2.45804259059345,0.466405023252212,-4.85694327579659));
#10988=CARTESIAN_POINT('Ctrl Pts',(2.4602202495084,0.471422396056728,-4.85731027257533));
#10989=CARTESIAN_POINT('Ctrl Pts',(2.46485398363867,0.481898207369978,-4.85808136374389));
#10990=CARTESIAN_POINT('Ctrl Pts',(2.46731687334954,0.487353441797358,-4.85848568004611));
#10991=CARTESIAN_POINT('Ctrl Pts',(2.47389833630932,0.501639816882176,-4.85955196275789));
#10992=CARTESIAN_POINT('Ctrl Pts',(2.47808504058831,0.5104388749908,-4.86021622912454));
#10993=CARTESIAN_POINT('Ctrl Pts',(2.49832540071275,0.551651311248119,-4.86336397318484));
#10994=CARTESIAN_POINT('Ctrl Pts',(2.51575599386501,0.583362757437863,-4.86589429827743));
#10995=CARTESIAN_POINT('Ctrl Pts',(2.56813394305839,0.66905648477249,-4.87304338174069));
#10996=CARTESIAN_POINT('Ctrl Pts',(2.60608093576134,0.721052920950755,-4.87775116002841));
#10997=CARTESIAN_POINT('Ctrl Pts',(2.68755045370288,0.815409888972056,-4.8868996745501));
#10998=CARTESIAN_POINT('Ctrl Pts',(2.73048932778562,0.858030384853922,-4.8913244050864));
#10999=CARTESIAN_POINT('Ctrl Pts',(2.78414315453906,0.903660695744325,-4.89626348002543));
#11000=CARTESIAN_POINT('Ctrl Pts',(2.79185635786389,0.910052697294059,-4.89696041008659));
#11001=CARTESIAN_POINT('Ctrl Pts',(2.80271440234051,0.918819612625345,-4.89792234319587));
#11002=CARTESIAN_POINT('Ctrl Pts',(2.80579076202136,0.921278117559275,-4.89819278072557));
#11003=CARTESIAN_POINT('Ctrl Pts',(2.81111989604328,0.925493324914357,-4.8986575588927));
#11004=CARTESIAN_POINT('Ctrl Pts',(2.81336681279798,0.927257327174282,-4.89885239987541));
#11005=CARTESIAN_POINT('Ctrl Pts',(2.81812169032928,0.930962388345032,-4.89926231600909));
#11006=CARTESIAN_POINT('Ctrl Pts',(2.82063111368446,0.932901524552633,-4.89947725067882));
#11007=CARTESIAN_POINT('Ctrl Pts',(2.82687926435044,0.937689549601756,-4.90000902738763));
#11008=CARTESIAN_POINT('Ctrl Pts',(2.83062732232272,0.94052627598783,-4.90032503752866));
#11009=CARTESIAN_POINT('Ctrl Pts',(2.84483978053464,0.951149781903242,-4.90151254062941));
#11010=CARTESIAN_POINT('Ctrl Pts',(2.85541676486228,0.958785321776503,-4.90237437294793));
#11011=CARTESIAN_POINT('Ctrl Pts',(2.88292124661867,0.977953898020603,-4.90456601645266));
#11012=CARTESIAN_POINT('Ctrl Pts',(2.90002714399,0.989224293938772,-4.90588219422197));
#11013=CARTESIAN_POINT('Ctrl Pts',(2.9665208201606,1.03058819911785,-4.91085715353935));
#11014=CARTESIAN_POINT('Ctrl Pts',(3.01780819301119,1.0574769938129,-4.91440789604782));
#11015=CARTESIAN_POINT('Ctrl Pts',(3.14010377862566,1.11052160963622,-4.92266194772751));
#11016=CARTESIAN_POINT('Ctrl Pts',(3.21205779908429,1.1338243803949,-4.9273753365722));
#11017=CARTESIAN_POINT('Ctrl Pts',(3.29588425755089,1.1523215915183,-4.93300927013435));
#11018=CARTESIAN_POINT('Ctrl Pts',(3.30605663399126,1.15442550712546,-4.93369498093768));
#11019=CARTESIAN_POINT('Ctrl Pts',(3.3228574078038,1.15766921371327,-4.93483149939424));
#11020=CARTESIAN_POINT('Ctrl Pts',(3.3294702419773,1.1588872985261,-4.93527984816823));
#11021=CARTESIAN_POINT('Ctrl Pts',(3.34143872464283,1.16098609045903,-4.93609329993561));
#11022=CARTESIAN_POINT('Ctrl Pts',(3.34679075643416,1.16188653521442,-4.93645777348734));
#11023=CARTESIAN_POINT('Ctrl Pts',(3.35829104697559,1.16373973930365,-4.93724256981999));
#11024=CARTESIAN_POINT('Ctrl Pts',(3.36444099136388,1.16468083213406,-4.93766324560173));
#11025=CARTESIAN_POINT('Ctrl Pts',(3.38131574953266,1.16712641167665,-4.9388204040293));
#11026=CARTESIAN_POINT('Ctrl Pts',(3.39205408767386,1.16853173531024,-4.93955994350245));
#11027=CARTESIAN_POINT('Ctrl Pts',(3.45576337635456,1.1759772147161,-4.94396759026165));
#11028=CARTESIAN_POINT('Ctrl Pts',(3.50906807416584,1.17856212843965,-4.94774153101322));
#11029=CARTESIAN_POINT('Ctrl Pts',(3.61033405240667,1.17659800293228,-4.95506187508456));
#11030=CARTESIAN_POINT('Ctrl Pts',(3.65820619677908,1.17273635210013,-4.95858594720604));
#11031=CARTESIAN_POINT('Ctrl Pts',(3.73365671957204,1.16198223156333,-4.96417761414976));
#11032=CARTESIAN_POINT('Ctrl Pts',(3.76145538193309,1.15699459816853,-4.96624536504702));
#11033=CARTESIAN_POINT('Ctrl Pts',(3.82290217532677,1.14367346340159,-4.97080393714518));
#11034=CARTESIAN_POINT('Ctrl Pts',(3.85641908781445,1.13484353457212,-4.97328234020087));
#11035=CARTESIAN_POINT('Ctrl Pts',(3.89528922304976,1.12274636261065,-4.97611184231512));
#11036=CARTESIAN_POINT('Ctrl Pts',(3.90106355613962,1.12090025637399,-4.97653098363207));
#11037=CARTESIAN_POINT('Ctrl Pts',(3.91045784998563,1.11781666693035,-4.97721064972915));
#11038=CARTESIAN_POINT('Ctrl Pts',(3.91408640416377,1.11660601486784,-4.97747262382686));
#11039=CARTESIAN_POINT('Ctrl Pts',(3.92058945564488,1.11440103162938,-4.97794106619979));
#11040=CARTESIAN_POINT('Ctrl Pts',(3.9234660493333,1.11341322773696,-4.97814789811702));
#11041=CARTESIAN_POINT('Ctrl Pts',(3.92979668368952,1.11121187606592,-4.97860223891341));
#11042=CARTESIAN_POINT('Ctrl Pts',(3.93324890939516,1.10999336196327,-4.97884945630969));
#11043=CARTESIAN_POINT('Ctrl Pts',(3.94324494394163,1.10641261090348,-4.97956385642956));
#11044=CARTESIAN_POINT('Ctrl Pts',(3.94977371094593,1.1040084157086,-4.98002867814957));
#11045=CARTESIAN_POINT('Ctrl Pts',(4.00506944076144,1.08308768601547,-4.98395345115396));
#11046=CARTESIAN_POINT('Ctrl Pts',(4.05258455145938,1.06140536821004,-4.98724711658884));
#11047=CARTESIAN_POINT('Ctrl Pts',(4.17164865522746,0.997201983320257,-4.99567345831521));
#11048=CARTESIAN_POINT('Ctrl Pts',(4.24040421909818,0.950136426472314,-5.00072993691118));
#11049=CARTESIAN_POINT('Ctrl Pts',(4.32716778581371,0.87616263716116,-5.00800130417276));
#11050=CARTESIAN_POINT('Ctrl Pts',(4.34990039028731,0.855180286455938,-5.01000182993786));
#11051=CARTESIAN_POINT('Ctrl Pts',(4.37856066632914,0.826556759223605,-5.01267122140765));
#11052=CARTESIAN_POINT('Ctrl Pts',(4.38525861238371,0.819702076277839,-5.01330623739476));
#11053=CARTESIAN_POINT('Ctrl Pts',(4.39597841446718,0.808460158657226,-5.01434137203927));
#11054=CARTESIAN_POINT('Ctrl Pts',(4.40005206822568,0.804122747761935,-5.01473926739358));
#11055=CARTESIAN_POINT('Ctrl Pts',(4.40781380533997,0.795731934218784,-5.01550628778432));
#11056=CARTESIAN_POINT('Ctrl Pts',(4.41150681758084,0.791683285624797,-5.01587519137215));
#11057=CARTESIAN_POINT('Ctrl Pts',(4.41998514415882,0.782257205135081,-5.0167314312037));
#11058=CARTESIAN_POINT('Ctrl Pts',(4.42474963970937,0.776861427163581,-5.01721961093467));
#11059=CARTESIAN_POINT('Ctrl Pts',(4.43976544584706,0.75953856378957,-5.01878094850704));
#11060=CARTESIAN_POINT('Ctrl Pts',(4.44982708297487,0.747450096538627,-5.01986169829694));
#11061=CARTESIAN_POINT('Ctrl Pts',(4.47290531154009,0.718565618349747,-5.02242494659652));
#11062=CARTESIAN_POINT('Ctrl Pts',(4.48571503494254,0.701612088290005,-5.02391486948382));
#11063=CARTESIAN_POINT('Ctrl Pts',(4.53234344503568,0.636299038446352,-5.02960137648408));
#11064=CARTESIAN_POINT('Ctrl Pts',(4.56296725837986,0.585772229158071,-5.0338991803957));
#11065=CARTESIAN_POINT('Ctrl Pts',(4.62179279736881,0.469906809288292,-5.04343112368654));
#11066=CARTESIAN_POINT('Ctrl Pts',(4.64813228953771,0.403865518499825,-5.04866147002493));
#11067=CARTESIAN_POINT('Ctrl Pts',(4.67115501107625,0.32648221392716,-5.05431985113295));
#11068=CARTESIAN_POINT('Ctrl Pts',(4.67382544033851,0.31707982072097,-5.05499957702466));
#11069=CARTESIAN_POINT('Ctrl Pts',(4.67739662796914,0.303882986312167,-5.05594174084201));
#11070=CARTESIAN_POINT('Ctrl Pts',(4.67839597714514,0.300115973771326,-5.05620933467332));
#11071=CARTESIAN_POINT('Ctrl Pts',(4.68009281730321,0.293589247781774,-5.05667056193083));
#11072=CARTESIAN_POINT('Ctrl Pts',(4.68079902900792,0.290831867286321,-5.05686467842316));
#11073=CARTESIAN_POINT('Ctrl Pts',(4.682273894142,0.284985199214715,-5.05727467063104));
#11074=CARTESIAN_POINT('Ctrl Pts',(4.68304003264503,0.281895300300368,-5.05749039735209));
#11075=CARTESIAN_POINT('Ctrl Pts',(4.68492015832999,0.274178792600658,-5.05802685898348));
#11076=CARTESIAN_POINT('Ctrl Pts',(4.68601866517052,0.26954840682987,-5.05834672958593));
#11077=CARTESIAN_POINT('Ctrl Pts',(4.69011954729817,0.251783789469712,-5.05956656713604));
#11078=CARTESIAN_POINT('Ctrl Pts',(4.69292467254144,0.238604461361061,-5.06045618263244));
#11079=CARTESIAN_POINT('Ctrl Pts',(4.69960316471049,0.204350057448847,-5.06273558269781));
#11080=CARTESIAN_POINT('Ctrl Pts',(4.70312882616146,0.183211625227725,-5.06411032068186));
#11081=CARTESIAN_POINT('Ctrl Pts',(4.7138833174533,0.105762915398194,-5.06906940637668));
#11082=CARTESIAN_POINT('Ctrl Pts',(4.71761607580232,0.0490443384848221,
-5.07255505310615));
#11083=CARTESIAN_POINT('Ctrl Pts',(4.71675170872838,-0.0827354315696169,
-5.08071566725665));
#11084=CARTESIAN_POINT('Ctrl Pts',(4.70909511443206,-0.157516755015795,
-5.08540207221873));
#11085=CARTESIAN_POINT('Ctrl Pts',(4.69234225810892,-0.241250456079762,
-5.0910063822924));
#11086=CARTESIAN_POINT('Ctrl Pts',(4.69016798173377,-0.251416300976573,
-5.09169261791472));
#11087=CARTESIAN_POINT('Ctrl Pts',(4.68636566296886,-0.268110343125979,
-5.09282982688427));
#11088=CARTESIAN_POINT('Ctrl Pts',(4.68481571720163,-0.274655876897023,
-5.09327833609971));
#11089=CARTESIAN_POINT('Ctrl Pts',(4.6819140121794,-0.286458148742733,-5.09409195931201));
#11090=CARTESIAN_POINT('Ctrl Pts',(4.68058181338018,-0.291719538145418,
-5.09445644264509));
#11091=CARTESIAN_POINT('Ctrl Pts',(4.67764499153434,-0.30299024760524,-5.09524112677651));
#11092=CARTESIAN_POINT('Ctrl Pts',(4.67602904118461,-0.308996417959883,
-5.09566167963423));
#11093=CARTESIAN_POINT('Ctrl Pts',(4.67147140981349,-0.325416691712802,
-5.09681815039107));
#11094=CARTESIAN_POINT('Ctrl Pts',(4.66843371198944,-0.335803276526833,
-5.0975571190521));
#11095=CARTESIAN_POINT('Ctrl Pts',(4.64963634002357,-0.396935957768268,
-5.10195194457051));
#11096=CARTESIAN_POINT('Ctrl Pts',(4.63060233275566,-0.446603141658404,
-5.10571289725965));
#11097=CARTESIAN_POINT('Ctrl Pts',(4.58806951823101,-0.538471856962764,
-5.1130288020892));
#11098=CARTESIAN_POINT('Ctrl Pts',(4.56519964453649,-0.580851876318216,
-5.11656225081209));
#11099=CARTESIAN_POINT('Ctrl Pts',(4.52487129943661,-0.645736921039312,
-5.1221674246078));
#11100=CARTESIAN_POINT('Ctrl Pts',(4.50907789240489,-0.66921668575073,-5.1242392176676));
#11101=CARTESIAN_POINT('Ctrl Pts',(4.4720931256705,-0.720139658713265,-5.12880234908559));
#11102=CARTESIAN_POINT('Ctrl Pts',(4.45050292872451,-0.747264613724035,
-5.13128133490666));
#11103=CARTESIAN_POINT('Ctrl Pts',(4.42376484515356,-0.777972485918973,
-5.13411141147721));
#11104=CARTESIAN_POINT('Ctrl Pts',(4.41974850969115,-0.782513844765413,
-5.13453057514588));
#11105=CARTESIAN_POINT('Ctrl Pts',(4.41314101893004,-0.789869831532346,
-5.135210270097));
#11106=CARTESIAN_POINT('Ctrl Pts',(4.41057096132481,-0.79270313748375,-5.13547225089546));
#11107=CARTESIAN_POINT('Ctrl Pts',(4.40593270427108,-0.797766691133861,
-5.13594070027414));
#11108=CARTESIAN_POINT('Ctrl Pts',(4.4038696348932,-0.800001488012628,-5.13614753254693));
#11109=CARTESIAN_POINT('Ctrl Pts',(4.39930428958679,-0.804908570244363,
-5.13660186822187));
#11110=CARTESIAN_POINT('Ctrl Pts',(4.39679820010056,-0.807577194066002,
-5.13684908018532));
#11111=CARTESIAN_POINT('Ctrl Pts',(4.38949384653271,-0.815282958961408,
-5.13756344871047));
#11112=CARTESIAN_POINT('Ctrl Pts',(4.38466324534603,-0.820289432306725,
-5.13802824458919));
#11113=CARTESIAN_POINT('Ctrl Pts',(4.34325230834112,-0.862453888401102,
-5.14195156931448));
#11114=CARTESIAN_POINT('Ctrl Pts',(4.30428086816322,-0.897192667489721,
-5.1452439502416));
#11115=CARTESIAN_POINT('Ctrl Pts',(4.20526894619093,-0.974294721189144,
-5.15306117737643));
#11116=CARTESIAN_POINT('Ctrl Pts',(4.14334526395964,-1.01383453137555,-5.15753270343064));
#11117=CARTESIAN_POINT('Ctrl Pts',(4.07816923100673,-1.04735430750874,-5.16216634940201));
#11118=CARTESIAN_POINT('Origin',(3.53951905042299,8.32667268468867E-16,
0.924367114736157));
#11119=CARTESIAN_POINT('',(4.07816926754817,-1.04735428871561,-5.76049882461148));
#11120=CARTESIAN_POINT('',(4.07816910321358,-1.04735437323224,-5.66222605418069));
#11121=CARTESIAN_POINT('',(4.07816926754759,-1.04735428871592,0.924367114736157));
#11122=CARTESIAN_POINT('Ctrl Pts',(4.07816926754817,-1.04735428871561,-5.76049882461148));
#11123=CARTESIAN_POINT('Ctrl Pts',(4.08187797021829,-1.04544691742776,-5.7602109730814));
#11124=CARTESIAN_POINT('Ctrl Pts',(4.08557659149742,-1.04351982170539,-5.75992423025184));
#11125=CARTESIAN_POINT('Ctrl Pts',(4.0921535430674,-1.04004848361736,-5.75941502498637));
#11126=CARTESIAN_POINT('Ctrl Pts',(4.0950358034973,-1.03851185282131,-5.75919210917261));
#11127=CARTESIAN_POINT('Ctrl Pts',(4.10065735843889,-1.03548471091922,-5.75875785247854));
#11128=CARTESIAN_POINT('Ctrl Pts',(4.1033971772514,-1.03399528321234,-5.75854645139605));
#11129=CARTESIAN_POINT('Ctrl Pts',(4.10951216720323,-1.03063950239022,-5.75807510583635));
#11130=CARTESIAN_POINT('Ctrl Pts',(4.11288418351973,-1.02876739948968,-5.75781551783258));
#11131=CARTESIAN_POINT('Ctrl Pts',(4.1245602271969,-1.0222097597932,-5.75691758717413));
#11132=CARTESIAN_POINT('Ctrl Pts',(4.13281677414963,-1.01743982462621,-5.75628426325137));
#11133=CARTESIAN_POINT('Ctrl Pts',(4.20590408407458,-0.974023855332084,
-5.75068435481918));
#11134=CARTESIAN_POINT('Ctrl Pts',(4.26694757189161,-0.929323684561039,
-5.74604456307055));
#11135=CARTESIAN_POINT('Ctrl Pts',(4.36509400579341,-0.841817399823423,
-5.73791063778276));
#11136=CARTESIAN_POINT('Ctrl Pts',(4.4041764651071,-0.801621765672082,-5.73444162186334));
#11137=CARTESIAN_POINT('Ctrl Pts',(4.45353200338592,-0.743034592168187,
-5.72955373113003));
#11138=CARTESIAN_POINT('Ctrl Pts',(4.46639760688376,-0.726922382736174,
-5.7282256810086));
#11139=CARTESIAN_POINT('Ctrl Pts',(4.4881039329886,-0.698224859840442,-5.72588040195009));
#11140=CARTESIAN_POINT('Ctrl Pts',(4.49713350583108,-0.685788417565081,
-5.72487034405517));
#11141=CARTESIAN_POINT('Ctrl Pts',(4.50999413973082,-0.667326043785865,
-5.72337794449112));
#11142=CARTESIAN_POINT('Ctrl Pts',(4.51401810663431,-0.66143596317433,-5.72290285309094));
#11143=CARTESIAN_POINT('Ctrl Pts',(4.52103366408996,-0.65096395058456,-5.72205979796052));
#11144=CARTESIAN_POINT('Ctrl Pts',(4.52404732127105,-0.646397001834558,
-5.72169266739557));
#11145=CARTESIAN_POINT('Ctrl Pts',(4.53028885661337,-0.63679355978032,-5.72092168133152));
#11146=CARTESIAN_POINT('Ctrl Pts',(4.53351039682175,-0.631753154043889,
-5.72051760644787));
#11147=CARTESIAN_POINT('Ctrl Pts',(4.54186840199153,-0.618454062256777,
-5.71945284293456));
#11148=CARTESIAN_POINT('Ctrl Pts',(4.54694112024298,-0.610156056360615,
-5.71878986685697));
#11149=CARTESIAN_POINT('Ctrl Pts',(4.56837709552367,-0.57409469829039,-5.715913935312));
#11150=CARTESIAN_POINT('Ctrl Pts',(4.58369840858914,-0.545731365712486,
-5.71366458384287));
#11151=CARTESIAN_POINT('Ctrl Pts',(4.64285297026951,-0.424587807314039,
-5.70410312700539));
#11152=CARTESIAN_POINT('Ctrl Pts',(4.67562736878406,-0.326914693602247,
-5.6964529405097));
#11153=CARTESIAN_POINT('Ctrl Pts',(4.69949361741635,-0.204996112739021,
-5.68746766158048));
#11154=CARTESIAN_POINT('Ctrl Pts',(4.70306836807499,-0.183623260953599,
-5.68591494403306));
#11155=CARTESIAN_POINT('Ctrl Pts',(4.70792153912013,-0.148711527529558,
-5.68342666138627));
#11156=CARTESIAN_POINT('Ctrl Pts',(4.70955873143027,-0.135228245804641,
-5.68247722908563));
#11157=CARTESIAN_POINT('Ctrl Pts',(4.71145576148858,-0.116970915556129,
-5.6812098309718));
#11158=CARTESIAN_POINT('Ctrl Pts',(4.71192024703539,-0.112219811000617,
-5.68088167733769));
#11159=CARTESIAN_POINT('Ctrl Pts',(4.71264663212656,-0.104292356197923,
-5.68033704921217));
#11160=CARTESIAN_POINT('Ctrl Pts',(4.71292454502956,-0.101117577404194,
-5.68011971509213));
#11161=CARTESIAN_POINT('Ctrl Pts',(4.71342611637666,-0.0951070651807408,
-5.67970977738906));
#11162=CARTESIAN_POINT('Ctrl Pts',(4.71365239347741,-0.0922715910167022,
-5.67951702687181));
#11163=CARTESIAN_POINT('Ctrl Pts',(4.71416367599844,-0.0855580854412196,
-5.67906210678509));
#11164=CARTESIAN_POINT('Ctrl Pts',(4.71443975529531,-0.0816793774734788,
-5.67880042413697));
#11165=CARTESIAN_POINT('Ctrl Pts',(4.7153453324281,-0.0680004129323329,
-5.67788136728897));
#11166=CARTESIAN_POINT('Ctrl Pts',(4.71587148298568,-0.0581933969691904,
-5.67722935507856));
#11167=CARTESIAN_POINT('Ctrl Pts',(4.71917359912949,0.0221236688189603,
-5.67193755633074));
#11168=CARTESIAN_POINT('Ctrl Pts',(4.71573051204669,0.0927560213869958,
-5.66758116501317));
#11169=CARTESIAN_POINT('Ctrl Pts',(4.70220420960147,0.189753681766197,-5.6615231504757));
#11170=CARTESIAN_POINT('Ctrl Pts',(4.69748385131342,0.21670423472124,-5.65983245808009));
#11171=CARTESIAN_POINT('Ctrl Pts',(4.6803833773342,0.29763991504475,-5.65468216482137));
#11172=CARTESIAN_POINT('Ctrl Pts',(4.66513246507091,0.350933452613339,-5.6511877373165));
#11173=CARTESIAN_POINT('Ctrl Pts',(4.64128702055945,0.416422732710736,-5.64663709518971));
#11174=CARTESIAN_POINT('Ctrl Pts',(4.63613717342558,0.42980136769828,-5.64569374705179));
#11175=CARTESIAN_POINT('Ctrl Pts',(4.62813390331266,0.449511869367758,-5.64428181793294));
#11176=CARTESIAN_POINT('Ctrl Pts',(4.6254664755146,0.455918200029565,-5.6438193974));
#11177=CARTESIAN_POINT('Ctrl Pts',(4.62060420778169,0.467311056885394,-5.64299056394301));
#11178=CARTESIAN_POINT('Ctrl Pts',(4.61843107060644,0.472306671931109,-5.64262488726538));
#11179=CARTESIAN_POINT('Ctrl Pts',(4.61375786272512,0.482848889929473,-5.64184834642741));
#11180=CARTESIAN_POINT('Ctrl Pts',(4.61124932293543,0.488391540617809,-5.64143720443628));
#11181=CARTESIAN_POINT('Ctrl Pts',(4.60442340864151,0.503167630464035,-5.64033330433663));
#11182=CARTESIAN_POINT('Ctrl Pts',(4.60002900316412,0.51236469951574,-5.63963794435653));
#11183=CARTESIAN_POINT('Ctrl Pts',(4.57912584711362,0.554691690831046,-5.63639839525907));
#11184=CARTESIAN_POINT('Ctrl Pts',(4.56118206338029,0.587085459727697,-5.63380539522078));
#11185=CARTESIAN_POINT('Ctrl Pts',(4.50080424386323,0.684910158569189,-5.62561004491299));
#11186=CARTESIAN_POINT('Ctrl Pts',(4.45338256230509,0.747008867384006,-5.61985722810707));
#11187=CARTESIAN_POINT('Ctrl Pts',(4.36598167253843,0.840574132074291,-5.61049174841205));
#11188=CARTESIAN_POINT('Ctrl Pts',(4.32947457570331,0.874972456660877,-5.60686257165182));
#11189=CARTESIAN_POINT('Ctrl Pts',(4.28555602926795,0.911357088863594,-5.60289629057012));
#11190=CARTESIAN_POINT('Ctrl Pts',(4.28019000214669,0.915723464946005,-5.60241805397284));
#11191=CARTESIAN_POINT('Ctrl Pts',(4.27193198134609,0.922322994137551,-5.60169213411281));
#11192=CARTESIAN_POINT('Ctrl Pts',(4.26906766433747,0.924590302644373,-5.60144216954969));
#11193=CARTESIAN_POINT('Ctrl Pts',(4.26379853065051,0.928721461643172,-5.6009857401457));
#11194=CARTESIAN_POINT('Ctrl Pts',(4.26139703398494,0.930589327297677,-5.60077900394143));
#11195=CARTESIAN_POINT('Ctrl Pts',(4.25595140505116,0.934791129956243,-5.60031309520597));
#11196=CARTESIAN_POINT('Ctrl Pts',(4.25290309109886,0.937119515831706,-5.60005430600372));
#11197=CARTESIAN_POINT('Ctrl Pts',(4.24498070036995,0.943109796148837,-5.59938676436009));
#11198=CARTESIAN_POINT('Ctrl Pts',(4.24008939695203,0.946748868803118,-5.59897951721716));
#11199=CARTESIAN_POINT('Ctrl Pts',(4.20653678410166,0.971309196386732,-5.59621746260358));
#11200=CARTESIAN_POINT('Ctrl Pts',(4.1769678758686,0.990966066580671,-5.593938803187));
#11201=CARTESIAN_POINT('Ctrl Pts',(4.1236633269368,1.02302689362179,-5.59001188727124));
#11202=CARTESIAN_POINT('Ctrl Pts',(4.10031071697327,1.0360122437924,-5.58834834205699));
#11203=CARTESIAN_POINT('Ctrl Pts',(4.0149451061379,1.07974731373108,-5.58240010731714));
#11204=CARTESIAN_POINT('Ctrl Pts',(3.95069627641039,1.10581053528477,-5.5781586868987));
#11205=CARTESIAN_POINT('Ctrl Pts',(3.86237914718799,1.13286947952707,-5.57229031259537));
#11206=CARTESIAN_POINT('Ctrl Pts',(3.84003153921409,1.13900133542013,-5.57080326312618));
#11207=CARTESIAN_POINT('Ctrl Pts',(3.80119010815015,1.14843618571334,-5.56820406305948));
#11208=CARTESIAN_POINT('Ctrl Pts',(3.78477927048749,1.15205242659533,-5.56710148814794));
#11209=CARTESIAN_POINT('Ctrl Pts',(3.76104852165796,1.15675164212147,-5.56549817696128));
#11210=CARTESIAN_POINT('Ctrl Pts',(3.75378650553274,1.15811878566181,-5.56500634661502));
#11211=CARTESIAN_POINT('Ctrl Pts',(3.74108842812285,1.1603857995812,-5.56414405906378));
#11212=CARTESIAN_POINT('Ctrl Pts',(3.73565796752716,1.16131603852538,-5.56377456470146));
#11213=CARTESIAN_POINT('Ctrl Pts',(3.72512620924544,1.16304415374054,-5.56305647579265));
#11214=CARTESIAN_POINT('Ctrl Pts',(3.72002578973926,1.16384665508634,-5.56270803512962));
#11215=CARTESIAN_POINT('Ctrl Pts',(3.70643205950566,1.16589398957059,-5.5617774757776));
#11216=CARTESIAN_POINT('Ctrl Pts',(3.69793026970683,1.16707952872154,-5.56119352437753));
#11217=CARTESIAN_POINT('Ctrl Pts',(3.66670418889264,1.17108639498765,-5.55904111579447));
#11218=CARTESIAN_POINT('Ctrl Pts',(3.64391321872698,1.17333760505385,-5.55745523764452));
#11219=CARTESIAN_POINT('Ctrl Pts',(3.51977541046958,1.18195421843716,-5.5487308679879));
#11220=CARTESIAN_POINT('Ctrl Pts',(3.41800597233407,1.17585429781606,-5.54121423498232));
#11221=CARTESIAN_POINT('Ctrl Pts',(3.28877692812439,1.15114172511511,-5.53161666038536));
#11222=CARTESIAN_POINT('Ctrl Pts',(3.25947335182741,1.14436599608088,-5.52944104699182));
#11223=CARTESIAN_POINT('Ctrl Pts',(3.21940805364577,1.1334704130046,-5.52649260053368));
#11224=CARTESIAN_POINT('Ctrl Pts',(3.20840064848533,1.13030387640634,-5.52568536704231));
#11225=CARTESIAN_POINT('Ctrl Pts',(3.18936118987572,1.12452471241741,-5.52429596647582));
#11226=CARTESIAN_POINT('Ctrl Pts',(3.18130794977989,1.12198537144151,-5.52371044199923));
#11227=CARTESIAN_POINT('Ctrl Pts',(3.16952152012374,1.11812903937646,-5.52285736138255));
#11228=CARTESIAN_POINT('Ctrl Pts',(3.16576676330985,1.11687955937425,-5.52258617996448));
#11229=CARTESIAN_POINT('Ctrl Pts',(3.15915449739544,1.11464209941013,-5.5221097332622));
#11230=CARTESIAN_POINT('Ctrl Pts',(3.15629441392398,1.11366201412777,-5.5219040235197));
#11231=CARTESIAN_POINT('Ctrl Pts',(3.15008452685253,1.11150727139893,-5.52145820897832));
#11232=CARTESIAN_POINT('Ctrl Pts',(3.14673624183696,1.11032847780941,-5.5212183468747));
#11233=CARTESIAN_POINT('Ctrl Pts',(3.13749912224382,1.10702945415866,-5.5205579155664));
#11234=CARTESIAN_POINT('Ctrl Pts',(3.1316216762133,1.10487735581501,-5.52013914740789));
#11235=CARTESIAN_POINT('Ctrl Pts',(3.09979435348579,1.09293480366891,-5.51787792953038));
#11236=CARTESIAN_POINT('Ctrl Pts',(3.07417707657814,1.08227603717349,-5.51608134887564));
#11237=CARTESIAN_POINT('Ctrl Pts',(2.96001171004169,1.0299701053567,-5.50807902160259));
#11238=CARTESIAN_POINT('Ctrl Pts',(2.87648634691669,0.978293121355073,-5.50220561684417));
#11239=CARTESIAN_POINT('Ctrl Pts',(2.76860924777622,0.891319951639726,-5.49345204055826));
#11240=CARTESIAN_POINT('Ctrl Pts',(2.73825861855538,0.8641379241976,-5.49083746251266));
#11241=CARTESIAN_POINT('Ctrl Pts',(2.70221543367556,0.828323419154846,-5.48749274426946));
#11242=CARTESIAN_POINT('Ctrl Pts',(2.69514436495158,0.82111412938354,-5.48682422764823));
#11243=CARTESIAN_POINT('Ctrl Pts',(2.68397740238912,0.809432093422194,-5.4857479111911));
#11244=CARTESIAN_POINT('Ctrl Pts',(2.67982173206068,0.805016983585061,-5.48534267741472));
#11245=CARTESIAN_POINT('Ctrl Pts',(2.67199447980697,0.796571343576881,-5.48457030632363));
#11246=CARTESIAN_POINT('Ctrl Pts',(2.66831642135929,0.792547010233152,-5.48420345578446));
#11247=CARTESIAN_POINT('Ctrl Pts',(2.659996158091,0.783315522386645,-5.48336451722359));
#11248=CARTESIAN_POINT('Ctrl Pts',(2.65537204681401,0.778092409765785,-5.48289169695835));
#11249=CARTESIAN_POINT('Ctrl Pts',(2.64126301155107,0.76186754058363,-5.48142836813775));
#11250=CARTESIAN_POINT('Ctrl Pts',(2.6319353164037,0.750731505820629,-5.48043155259047));
#11251=CARTESIAN_POINT('Ctrl Pts',(2.56321523408886,0.665535869787396,-5.47285818393117));
#11252=CARTESIAN_POINT('Ctrl Pts',(2.51277738798021,0.584723669108077,-5.46592659351282));
#11253=CARTESIAN_POINT('Ctrl Pts',(2.46545831132143,0.483500004215814,-5.45772823416619));
#11254=CARTESIAN_POINT('Ctrl Pts',(2.4586538936309,0.468091072589877,-5.45649369246843));
#11255=CARTESIAN_POINT('Ctrl Pts',(2.44008257185676,0.423469110787301,-5.45296442669784));
#11256=CARTESIAN_POINT('Ctrl Pts',(2.42915290952481,0.393921260158824,-5.45068242777589));
#11257=CARTESIAN_POINT('Ctrl Pts',(2.41398944423184,0.347256351690499,-5.44719518984603));
#11258=CARTESIAN_POINT('Ctrl Pts',(2.40893312800836,0.330423095061284,-5.44596034541842));
#11259=CARTESIAN_POINT('Ctrl Pts',(2.40285897387676,0.308425755885177,-5.44438180528872));
#11260=CARTESIAN_POINT('Ctrl Pts',(2.40149657098967,0.303360207342615,-5.44402069540589));
#11261=CARTESIAN_POINT('Ctrl Pts',(2.39933495208893,0.295103547797664,-5.44343617738116));
#11262=CARTESIAN_POINT('Ctrl Pts',(2.39851520022268,0.291917961967814,-5.44321164229907));
#11263=CARTESIAN_POINT('Ctrl Pts',(2.39694789207287,0.28571986987984,-5.44277673694889));
#11264=CARTESIAN_POINT('Ctrl Pts',(2.39619888504174,0.282707792013207,-5.44256629072002));
#11265=CARTESIAN_POINT('Ctrl Pts',(2.39438954056102,0.275306836420999,-5.44205134654796));
#11266=CARTESIAN_POINT('Ctrl Pts',(2.39334250255954,0.270914693819421,-5.44174759315083));
#11267=CARTESIAN_POINT('Ctrl Pts',(2.39039590650725,0.258231316151745,-5.44087545242379));
#11268=CARTESIAN_POINT('Ctrl Pts',(2.3885608303912,0.249925185453371,-5.44031047211065));
#11269=CARTESIAN_POINT('Ctrl Pts',(2.37023652933059,0.162497560652178,-5.43442131039376));
#11270=CARTESIAN_POINT('Ctrl Pts',(2.36184102968371,0.081886818770969,-5.42947575984217));
#11271=CARTESIAN_POINT('Ctrl Pts',(2.36170060219808,-0.076853429083801,
-5.41965115857095));
#11272=CARTESIAN_POINT('Ctrl Pts',(2.36935922258636,-0.154552289663843,
-5.41479595816134));
#11273=CARTESIAN_POINT('Ctrl Pts',(2.38667217463884,-0.241138361243689,
-5.409001177948));
#11274=CARTESIAN_POINT('Ctrl Pts',(2.38885056288667,-0.251327771583916,
-5.40831339200768));
#11275=CARTESIAN_POINT('Ctrl Pts',(2.39265897433033,-0.268052941995784,
-5.40717410680193));
#11276=CARTESIAN_POINT('Ctrl Pts',(2.39421041201499,-0.274606142455594,
-5.40672508692881));
#11277=CARTESIAN_POINT('Ctrl Pts',(2.39711386709529,-0.286417407576641,
-5.40591086490822));
#11278=CARTESIAN_POINT('Ctrl Pts',(2.39844621198487,-0.291680150079233,
-5.40554629698149));
#11279=CARTESIAN_POINT('Ctrl Pts',(2.40138202360195,-0.302948523881468,
-5.40476179433949));
#11280=CARTESIAN_POINT('Ctrl Pts',(2.40299674058769,-0.308951026269503,
-5.40434151002534));
#11281=CARTESIAN_POINT('Ctrl Pts',(2.40754710119242,-0.325347854318808,
-5.40318672721635));
#11282=CARTESIAN_POINT('Ctrl Pts',(2.41057827428529,-0.335714805536738,
-5.40244919348077));
#11283=CARTESIAN_POINT('Ctrl Pts',(2.42922746280897,-0.396386270078313,
-5.39808783960088));
#11284=CARTESIAN_POINT('Ctrl Pts',(2.44806122956953,-0.445632011384026,
-5.39436084152631));
#11285=CARTESIAN_POINT('Ctrl Pts',(2.50386500754007,-0.566569682512507,
-5.38473903378777));
#11286=CARTESIAN_POINT('Ctrl Pts',(2.5450141752443,-0.636034191557404,-5.37875501912202));
#11287=CARTESIAN_POINT('Ctrl Pts',(2.61159521268414,-0.725973060111868,
-5.37066474697488));
#11288=CARTESIAN_POINT('Ctrl Pts',(2.63126613025116,-0.750437572912024,
-5.36842656594675));
#11289=CARTESIAN_POINT('Ctrl Pts',(2.65614517266138,-0.778965671894448,
-5.36579699003843));
#11290=CARTESIAN_POINT('Ctrl Pts',(2.66043801205456,-0.783807028939528,
-5.36535003425088));
#11291=CARTESIAN_POINT('Ctrl Pts',(2.66717946535301,-0.791284811132123,
-5.36465891038453));
#11292=CARTESIAN_POINT('Ctrl Pts',(2.66960054914071,-0.793945719811108,
-5.36441282502232));
#11293=CARTESIAN_POINT('Ctrl Pts',(2.67409449905466,-0.798839589984025,
-5.36396001357935));
#11294=CARTESIAN_POINT('Ctrl Pts',(2.67616383505845,-0.801075600121314,
-5.36375304667247));
#11295=CARTESIAN_POINT('Ctrl Pts',(2.68090602061594,-0.806160023831496,
-5.36328222341102));
#11296=CARTESIAN_POINT('Ctrl Pts',(2.68358438151723,-0.809003190747652,
-5.36301878660978));
#11297=CARTESIAN_POINT('Ctrl Pts',(2.69191235383771,-0.81775594760654,-5.36220710403092));
#11298=CARTESIAN_POINT('Ctrl Pts',(2.69760953546321,-0.823620227858253,
-5.36166230643215));
#11299=CARTESIAN_POINT('Ctrl Pts',(2.71110311019176,-0.837223235370462,
-5.3603948724688));
#11300=CARTESIAN_POINT('Ctrl Pts',(2.71894772913704,-0.844913274583829,
-5.35967548753292));
#11301=CARTESIAN_POINT('Ctrl Pts',(2.74731345207494,-0.871952276395717,
-5.35713053458738));
#11302=CARTESIAN_POINT('Ctrl Pts',(2.76842167346318,-0.890673642735563,
-5.35533925522086));
#11303=CARTESIAN_POINT('Ctrl Pts',(2.85592957464787,-0.962841104189329,
-5.34821800193056));
#11304=CARTESIAN_POINT('Ctrl Pts',(2.92736595278234,-1.00976567656509,-5.34305707909272));
#11305=CARTESIAN_POINT('Ctrl Pts',(3.03746428937339,-1.06607390707546,-5.33523298199446));
#11306=CARTESIAN_POINT('Ctrl Pts',(3.07251965177669,-1.08188892823429,-5.33276222380301));
#11307=CARTESIAN_POINT('Ctrl Pts',(3.11786854942945,-1.09973270802842,-5.32955570707003));
#11308=CARTESIAN_POINT('Ctrl Pts',(3.12750305218602,-1.10337843928046,-5.32887397826383));
#11309=CARTESIAN_POINT('Ctrl Pts',(3.14292394472285,-1.10898362741727,-5.32778142848127));
#11310=CARTESIAN_POINT('Ctrl Pts',(3.1486800460156,-1.11102530754527,-5.32737331432099));
#11311=CARTESIAN_POINT('Ctrl Pts',(3.1590815479487,-1.1146238695666,-5.32663517410387));
#11312=CARTESIAN_POINT('Ctrl Pts',(3.16372130770967,-1.11619672066612,-5.32630567909582));
#11313=CARTESIAN_POINT('Ctrl Pts',(3.17466507196386,-1.11983062315997,-5.32552787824893));
#11314=CARTESIAN_POINT('Ctrl Pts',(3.18097688613779,-1.12186744470275,-5.3250787966946));
#11315=CARTESIAN_POINT('Ctrl Pts',(3.19950159289169,-1.127673067179,-5.32375917437759));
#11316=CARTESIAN_POINT('Ctrl Pts',(3.21175870416564,-1.13129640280128,-5.32288399234048));
#11317=CARTESIAN_POINT('Ctrl Pts',(3.28691637123713,-1.15218990980757,-5.31750325672743));
#11318=CARTESIAN_POINT('Ctrl Pts',(3.35109297639296,-1.16440661909638,-5.31283836441222));
#11319=CARTESIAN_POINT('Ctrl Pts',(3.4815427068083,-1.17817031081259,-5.3032740446111));
#11320=CARTESIAN_POINT('Ctrl Pts',(3.5476091309705,-1.17956820168689,-5.29838988657289));
#11321=CARTESIAN_POINT('Ctrl Pts',(3.64346970167869,-1.17353924632251,-5.2914541057521));
#11322=CARTESIAN_POINT('Ctrl Pts',(3.67341384531329,-1.17050101662678,-5.28931070605149));
#11323=CARTESIAN_POINT('Ctrl Pts',(3.70954916706981,-1.1654294403968,-5.28677636928521));
#11324=CARTESIAN_POINT('Ctrl Pts',(3.71587976536528,-1.16448826697449,-5.28633434340028));
#11325=CARTESIAN_POINT('Ctrl Pts',(3.72574079816218,-1.16293996018326,-5.28564920427298));
#11326=CARTESIAN_POINT('Ctrl Pts',(3.72927655145256,-1.16236826435742,-5.28540422464926));
#11327=CARTESIAN_POINT('Ctrl Pts',(3.73581670205787,-1.16128015001069,-5.28495241344372));
#11328=CARTESIAN_POINT('Ctrl Pts',(3.73882169674808,-1.16076819837799,-5.28474534983561));
#11329=CARTESIAN_POINT('Ctrl Pts',(3.74569398209677,-1.15956991420605,-5.28427298725828));
#11330=CARTESIAN_POINT('Ctrl Pts',(3.74955985527981,-1.15887589921931,-5.28400811895301));
#11331=CARTESIAN_POINT('Ctrl Pts',(3.76157266207668,-1.15665723149773,-5.28318751018547));
#11332=CARTESIAN_POINT('Ctrl Pts',(3.76970723664417,-1.15506587088829,-5.28263532794448));
#11333=CARTESIAN_POINT('Ctrl Pts',(3.83661038237051,-1.14124278450046,-5.2781177011429));
#11334=CARTESIAN_POINT('Ctrl Pts',(3.89439008077191,-1.1246185530536,-5.27436561515831));
#11335=CARTESIAN_POINT('Ctrl Pts',(3.99427769691301,-1.08740815070123,-5.26775588752701));
#11336=CARTESIAN_POINT('Ctrl Pts',(4.03685409330635,-1.06860254091493,-5.26489557995374));
#11337=CARTESIAN_POINT('Ctrl Pts',(4.07816965980385,-1.04735408697996,-5.26199342056381));
#11338=CARTESIAN_POINT('',(2.36176914077046,-0.000461317087656274,-5.32467780803899));
#11339=CARTESIAN_POINT('Ctrl Pts',(4.07816923100673,-1.04735430750874,-5.16216634940201));
#11340=CARTESIAN_POINT('Ctrl Pts',(4.06954594519216,-1.05178922931881,-5.16277941607337));
#11341=CARTESIAN_POINT('Ctrl Pts',(4.06086571266395,-1.05611877161022,-5.16339511164852));
#11342=CARTESIAN_POINT('Ctrl Pts',(4.02422928907034,-1.07383027455862,-5.16599008202834));
#11343=CARTESIAN_POINT('Ctrl Pts',(3.99580880295806,-1.08621124808923,-5.16799465148405));
#11344=CARTESIAN_POINT('Ctrl Pts',(3.95799837785832,-1.10093691545352,-5.1706686799783));
#11345=CARTESIAN_POINT('Ctrl Pts',(3.94901980326884,-1.10430800222505,-5.17130413723277));
#11346=CARTESIAN_POINT('Ctrl Pts',(3.93440401552854,-1.10959287681835,-5.17233981341572));
#11347=CARTESIAN_POINT('Ctrl Pts',(3.92879158409062,-1.11157428014712,-5.17273780465028));
#11348=CARTESIAN_POINT('Ctrl Pts',(3.91798382177167,-1.11529794418402,-5.1735048881612));
#11349=CARTESIAN_POINT('Ctrl Pts',(3.91279086561634,-1.11704665869182,-5.17387375809825));
#11350=CARTESIAN_POINT('Ctrl Pts',(3.90075138453087,-1.12100759623962,-5.1747297395303));
#11351=CARTESIAN_POINT('Ctrl Pts',(3.89389647247439,-1.12319342448057,-5.17521769286783));
#11352=CARTESIAN_POINT('Ctrl Pts',(3.87201250858318,-1.12995129713792,-5.17677755899423));
#11353=CARTESIAN_POINT('Ctrl Pts',(3.85691235686831,-1.13428536152726,-5.17785704354953));
#11354=CARTESIAN_POINT('Ctrl Pts',(3.82122668420206,-1.1437595538521,-5.18041675377306));
#11355=CARTESIAN_POINT('Ctrl Pts',(3.80058055724751,-1.14864785781617,-5.1819043760131));
#11356=CARTESIAN_POINT('Ctrl Pts',(3.72220228778639,-1.16498294694491,-5.18757730057855));
#11357=CARTESIAN_POINT('Ctrl Pts',(3.66377693921275,-1.1726538325667,-5.19186328929927));
#11358=CARTESIAN_POINT('Ctrl Pts',(3.53396619351954,-1.17988554379157,-5.20139999393195));
#11359=CARTESIAN_POINT('Ctrl Pts',(3.46268409500139,-1.17739497352301,-5.20664755121257));
#11360=CARTESIAN_POINT('Ctrl Pts',(3.38233431058428,-1.16725493270965,-5.21232347803451));
#11361=CARTESIAN_POINT('Ctrl Pts',(3.37262582040075,-1.1659064223766,-5.21300508535927));
#11362=CARTESIAN_POINT('Ctrl Pts',(3.35909531752035,-1.16385455303246,-5.21394812755899));
#11363=CARTESIAN_POINT('Ctrl Pts',(3.35525855932799,-1.1632532899158,-5.21421476270541));
#11364=CARTESIAN_POINT('Ctrl Pts',(3.34861834408074,-1.16217901591583,-5.21467479594472));
#11365=CARTESIAN_POINT('Ctrl Pts',(3.34581352524841,-1.16171481641241,-5.2148686713017));
#11366=CARTESIAN_POINT('Ctrl Pts',(3.33986735586797,-1.16070858738544,-5.21527870637729));
#11367=CARTESIAN_POINT('Ctrl Pts',(3.33672646713476,-1.16016395076476,-5.21549471418181));
#11368=CARTESIAN_POINT('Ctrl Pts',(3.32888218764301,-1.15877090726724,-5.2160328215323));
#11369=CARTESIAN_POINT('Ctrl Pts',(3.32418161675929,-1.15790660034051,-5.21635404532803));
#11370=CARTESIAN_POINT('Ctrl Pts',(3.30610006356069,-1.15446797790832,-5.21758540470949));
#11371=CARTESIAN_POINT('Ctrl Pts',(3.29275826485404,-1.15169001447968,-5.21848493652365));
#11372=CARTESIAN_POINT('Ctrl Pts',(3.2582370480039,-1.14387469091385,-5.22079594981218));
#11373=CARTESIAN_POINT('Ctrl Pts',(3.23714309880603,-1.13848046687896,-5.22219185667478));
#11374=CARTESIAN_POINT('Ctrl Pts',(3.11600526270854,-1.10389780745085,-5.23017686243674));
#11375=CARTESIAN_POINT('Ctrl Pts',(3.02003998118047,-1.06211955896774,-5.2364198330601));
#11376=CARTESIAN_POINT('Ctrl Pts',(2.90448907796051,-0.992359828262857,
-5.24502942516393));
#11377=CARTESIAN_POINT('Ctrl Pts',(2.87879268843153,-0.975439139234408,
-5.24701933167632));
#11378=CARTESIAN_POINT('Ctrl Pts',(2.84601225213423,-0.951963701838311,
-5.24967654751156));
#11379=CARTESIAN_POINT('Ctrl Pts',(2.83830333440822,-0.946299677497521,
-5.25031040477959));
#11380=CARTESIAN_POINT('Ctrl Pts',(2.82591555379399,-0.936963432540757,
-5.25134411747404));
#11381=CARTESIAN_POINT('Ctrl Pts',(2.82119390832007,-0.933348494587354,
-5.2517417611111));
#11382=CARTESIAN_POINT('Ctrl Pts',(2.8123533742184,-0.926473277831047,-5.25249329455644));
#11383=CARTESIAN_POINT('Ctrl Pts',(2.80822851409927,-0.923220886427001,
-5.25284686966135));
#11384=CARTESIAN_POINT('Ctrl Pts',(2.80407572692206,-0.919901181918829,
-5.25320584702733));
#11385=CARTESIAN_POINT('Ctrl Pts',(2.80402585121794,-0.9198613050351,-5.25321015885017));
#11386=CARTESIAN_POINT('Ctrl Pts',(2.79867626710525,-0.915583464329012,
-5.25367268508899));
#11387=CARTESIAN_POINT('Ctrl Pts',(2.79341337937164,-0.911299859561506,
-5.25413270434317));
#11388=CARTESIAN_POINT('Ctrl Pts',(2.78234325708448,-0.902129415389332,
-5.25511110413334));
#11389=CARTESIAN_POINT('Ctrl Pts',(2.77654567677841,-0.89723145874577,-5.25562991832872));
#11390=CARTESIAN_POINT('Ctrl Pts',(2.76126933520918,-0.884070450884006,
-5.25701433163151));
#11391=CARTESIAN_POINT('Ctrl Pts',(2.75187509932375,-0.875711234747423,
-5.25788377987637));
#11392=CARTESIAN_POINT('Ctrl Pts',(2.72335576010973,-0.849503861365732,
-5.26058040448012));
#11393=CARTESIAN_POINT('Ctrl Pts',(2.70469106348343,-0.831168686064245,
-5.26242686756778));
#11394=CARTESIAN_POINT('Ctrl Pts',(2.65458394974946,-0.778554626165861,
-5.26761634042853));
#11395=CARTESIAN_POINT('Ctrl Pts',(2.62453950966349,-0.743013621361341,
-5.27100335456085));
#11396=CARTESIAN_POINT('Ctrl Pts',(2.55176092095107,-0.645791386941205,
-5.27990625261433));
#11397=CARTESIAN_POINT('Ctrl Pts',(2.51267170899475,-0.581634814651451,
-5.28544405643126));
#11398=CARTESIAN_POINT('Ctrl Pts',(2.47576333958393,-0.505579398100091,
-5.29136621820683));
#11399=CARTESIAN_POINT('Ctrl Pts',(2.4716880949209,-0.496914283527631,-5.29203190084747));
#11400=CARTESIAN_POINT('Ctrl Pts',(2.46611739268188,-0.484684298346281,
-5.29295787822271));
#11401=CARTESIAN_POINT('Ctrl Pts',(2.46453324370589,-0.481160580591559,
-5.29322310658612));
#11402=CARTESIAN_POINT('Ctrl Pts',(2.46170120190408,-0.47477729657079,-5.29370066701408));
#11403=CARTESIAN_POINT('Ctrl Pts',(2.46044728053015,-0.471920451078741,
-5.29391335332554));
#11404=CARTESIAN_POINT('Ctrl Pts',(2.45790520166865,-0.466065651054419,
-5.29434704622143));
#11405=CARTESIAN_POINT('Ctrl Pts',(2.45661812699473,-0.463067273304233,
-5.29456798820606));
#11406=CARTESIAN_POINT('Ctrl Pts',(2.45334082313665,-0.455344051664382,
-5.2951342045985));
#11407=CARTESIAN_POINT('Ctrl Pts',(2.45136892829536,-0.450611430090074,
-5.29547840366465));
#11408=CARTESIAN_POINT('Ctrl Pts',(2.44318859744525,-0.43061146081172,-5.29692197235739));
#11409=CARTESIAN_POINT('Ctrl Pts',(2.43726974073351,-0.415226707600595,
-5.2980055041011));
#11410=CARTESIAN_POINT('Ctrl Pts',(2.42196474723824,-0.372808362453588,
-5.30093316575204));
#11411=CARTESIAN_POINT('Ctrl Pts',(2.41323733858201,-0.345548012929315,
-5.30274937538456));
#11412=CARTESIAN_POINT('Ctrl Pts',(2.3765262167229,-0.214631806628227,-5.31128132720297));
#11413=CARTESIAN_POINT('Ctrl Pts',(2.36181118552444,-0.107802247071361,
-5.31773716168021));
#11414=CARTESIAN_POINT('Ctrl Pts',(2.36176914077046,-0.000461317087656274,
-5.32467780803899));
#11415=CARTESIAN_POINT('Ctrl Pts',(2.36176914030695,-0.000460132223236021,
-5.32467788465214));
#11416=CARTESIAN_POINT('Ctrl Pts',(2.36176218208443,0.0173500656714707,
-5.32582948951348));
#11417=CARTESIAN_POINT('Ctrl Pts',(2.36215921809729,0.035157527681886,-5.32699181323502));
#11418=CARTESIAN_POINT('Ctrl Pts',(2.3632691720255,0.0598215599466171,-5.32862005852875));
#11419=CARTESIAN_POINT('Ctrl Pts',(2.36363868602289,0.0666915346234238,
-5.32907556756017));
#11420=CARTESIAN_POINT('Ctrl Pts',(2.3644002772694,0.078861738762373,-5.32988620127089));
#11421=CARTESIAN_POINT('Ctrl Pts',(2.36476808268668,0.0841633358823255,
-5.33024057524318));
#11422=CARTESIAN_POINT('Ctrl Pts',(2.36557001120865,0.0946900465848394,
-5.33094677471049));
#11423=CARTESIAN_POINT('Ctrl Pts',(2.36600317047549,0.0999151119196681,
-5.3312985625889));
#11424=CARTESIAN_POINT('Ctrl Pts',(2.36700216866462,0.111061256840237,-5.33205176524902));
#11425=CARTESIAN_POINT('Ctrl Pts',(2.36757800207991,0.116981270939718,-5.33245348045136));
#11426=CARTESIAN_POINT('Ctrl Pts',(2.36919749596898,0.132416576679595,-5.33350536151939));
#11427=CARTESIAN_POINT('Ctrl Pts',(2.37031234577512,0.141923793023607,-5.33415771540511));
#11428=CARTESIAN_POINT('Ctrl Pts',(2.37550618290751,0.181987410491881,-5.33692625935416));
#11429=CARTESIAN_POINT('Ctrl Pts',(2.38066783325029,0.212388623843495,-5.33907556510917));
#11430=CARTESIAN_POINT('Ctrl Pts',(2.40181113676883,0.312853355052812,-5.34634522342824));
#11431=CARTESIAN_POINT('Ctrl Pts',(2.42300696479493,0.381647643014338,-5.35160907313795));
#11432=CARTESIAN_POINT('Ctrl Pts',(2.46712095405588,0.488880828005473,-5.36011728039088));
#11433=CARTESIAN_POINT('Ctrl Pts',(2.48618966019543,0.528715246695372,-5.3633476902778));
#11434=CARTESIAN_POINT('Ctrl Pts',(2.51445764562731,0.580134262995262,-5.36754283658415));
#11435=CARTESIAN_POINT('Ctrl Pts',(2.52170112289692,0.592750667957972,-5.36857415580377));
#11436=CARTESIAN_POINT('Ctrl Pts',(2.53438378119058,0.613922487675207,-5.37030437269975));
#11437=CARTESIAN_POINT('Ctrl Pts',(2.5397029241979,0.622547557451122,-5.37100909978507));
#11438=CARTESIAN_POINT('Ctrl Pts',(2.54741440164807,0.634698003507631,-5.37200053260632));
#11439=CARTESIAN_POINT('Ctrl Pts',(2.5497153862648,0.638280422394235,-5.37229267667029));
#11440=CARTESIAN_POINT('Ctrl Pts',(2.55371926113885,0.644440361987284,-5.37279461853859));
#11441=CARTESIAN_POINT('Ctrl Pts',(2.55541294259596,0.647023781763348,-5.37300500443261));
#11442=CARTESIAN_POINT('Ctrl Pts',(2.55898890146486,0.652431766350065,-5.37344511852398));
#11443=CARTESIAN_POINT('Ctrl Pts',(2.56087324129983,0.655254884589665,-5.37367470863777));
#11444=CARTESIAN_POINT('Ctrl Pts',(2.56596637797745,0.662814442887124,-5.37428916829446));
#11445=CARTESIAN_POINT('Ctrl Pts',(2.56919757487456,0.667535788630894,-5.37467258993907));
#11446=CARTESIAN_POINT('Ctrl Pts',(2.58397292363304,0.68879118293419,-5.37639811437618));
#11447=CARTESIAN_POINT('Ctrl Pts',(2.59590690287419,0.705051718620397,-5.3777164237304));
#11448=CARTESIAN_POINT('Ctrl Pts',(2.65304360781473,0.778851347227151,-5.3837323719598));
#11449=CARTESIAN_POINT('Ctrl Pts',(2.70313147551925,0.832409768482937,-5.38820095348185));
#11450=CARTESIAN_POINT('Ctrl Pts',(2.79380895083795,0.912863535265693,-5.39571449053853));
#11451=CARTESIAN_POINT('Ctrl Pts',(2.83166270732532,0.942519097487514,-5.39871231668154));
#11452=CARTESIAN_POINT('Ctrl Pts',(2.88670025609378,0.980446920214892,-5.40299124493225));
#11453=CARTESIAN_POINT('Ctrl Pts',(2.902433894309,0.990742644470822,-5.40420574270628));
#11454=CARTESIAN_POINT('Ctrl Pts',(2.92690330446177,1.00593092150125,-5.40608626431453));
#11455=CARTESIAN_POINT('Ctrl Pts',(2.93546662468846,1.0110963001918,-5.40674284887687));
#11456=CARTESIAN_POINT('Ctrl Pts',(2.94973379430735,1.01945629389923,-5.40783491118338));
#11457=CARTESIAN_POINT('Ctrl Pts',(2.95540042169561,1.02271364919015,-5.40826817784132));
#11458=CARTESIAN_POINT('Ctrl Pts',(2.96513402031088,1.02820154260224,-5.40901174861282));
#11459=CARTESIAN_POINT('Ctrl Pts',(2.96918763612002,1.03045555549498,-5.40932122120047));
#11460=CARTESIAN_POINT('Ctrl Pts',(2.97794458271416,1.03525735527898,-5.4099894209425));
#11461=CARTESIAN_POINT('Ctrl Pts',(2.98265215237526,1.03779715295912,-5.41034841851274));
#11462=CARTESIAN_POINT('Ctrl Pts',(2.99270515863957,1.0431327909147,-5.41111469014369));
#11463=CARTESIAN_POINT('Ctrl Pts',(2.99805508422066,1.04591979745029,-5.41152225979603));
#11464=CARTESIAN_POINT('Ctrl Pts',(3.01229375241259,1.05319881003785,-5.41260655109632));
#11465=CARTESIAN_POINT('Ctrl Pts',(3.02121830481511,1.05761929580783,-5.41328571568033));
#11466=CARTESIAN_POINT('Ctrl Pts',(3.06131711267147,1.07685150537706,-5.41633604545866));
#11467=CARTESIAN_POINT('Ctrl Pts',(3.09307459823361,1.09040047183823,-5.41874930666968));
#11468=CARTESIAN_POINT('Ctrl Pts',(3.2190923431032,1.1377360072122,-5.42832076112145));
#11469=CARTESIAN_POINT('Ctrl Pts',(3.31690868400419,1.16084305911693,-5.43578429227747));
#11470=CARTESIAN_POINT('Ctrl Pts',(3.43782525288453,1.17354828775046,-5.44457594973637));
#11471=CARTESIAN_POINT('Ctrl Pts',(3.45926406281154,1.17520911382985,-5.44611638640693));
#11472=CARTESIAN_POINT('Ctrl Pts',(3.49422615156354,1.17695624930548,-5.44858726044562));
#11473=CARTESIAN_POINT('Ctrl Pts',(3.50772609327481,1.17739827853978,-5.44953134280699));
#11474=CARTESIAN_POINT('Ctrl Pts',(3.52599390410295,1.17768196908734,-5.45079277762062));
#11475=CARTESIAN_POINT('Ctrl Pts',(3.5307569668994,1.17772703872595,-5.45112019992988));
#11476=CARTESIAN_POINT('Ctrl Pts',(3.53870456490796,1.17775402310513,-5.45166392419398));
#11477=CARTESIAN_POINT('Ctrl Pts',(3.54188894347072,1.17775192067781,-5.45188108026688));
#11478=CARTESIAN_POINT('Ctrl Pts',(3.54791889706899,1.17772348303803,-5.45229091579987));
#11479=CARTESIAN_POINT('Ctrl Pts',(3.5507644430228,1.17769975015124,-5.45248374065223));
#11480=CARTESIAN_POINT('Ctrl Pts',(3.55750390427682,1.1776191119659,-5.45293912362569));
#11481=CARTESIAN_POINT('Ctrl Pts',(3.56139770870814,1.17755320610843,-5.45320119220142));
#11482=CARTESIAN_POINT('Ctrl Pts',(3.57504488355748,1.17725450006819,-5.45411630001598));
#11483=CARTESIAN_POINT('Ctrl Pts',(3.5847959439077,1.17691981919061,-5.45476406446361));
#11484=CARTESIAN_POINT('Ctrl Pts',(3.66602687351153,1.17312066026462,-5.46011784882681));
#11485=CARTESIAN_POINT('Ctrl Pts',(3.73706861921467,1.16326839096062,-5.46453201091551));
#11486=CARTESIAN_POINT('Ctrl Pts',(3.86383029435777,1.1337319934743,-5.47258287667158));
#11487=CARTESIAN_POINT('Ctrl Pts',(3.91980155044283,1.11620364603449,-5.47620364459922));
#11488=CARTESIAN_POINT('Ctrl Pts',(3.99389843075455,1.08677601058208,-5.4812858656866));
#11489=CARTESIAN_POINT('Ctrl Pts',(4.01334732673234,1.07843840956472,-5.48264772785415));
#11490=CARTESIAN_POINT('Ctrl Pts',(4.04679741904642,1.0630190430275,-5.48504723714126));
#11491=CARTESIAN_POINT('Ctrl Pts',(4.06090151420348,1.05617286369517,-5.48607723312786));
#11492=CARTESIAN_POINT('Ctrl Pts',(4.08126778919107,1.04577963771955,-5.48759355788668));
#11493=CARTESIAN_POINT('Ctrl Pts',(4.08764115927244,1.04245330666869,-5.4880722934461));
#11494=CARTESIAN_POINT('Ctrl Pts',(4.09881712362062,1.03648962550631,-5.48891944990733));
#11495=CARTESIAN_POINT('Ctrl Pts',(4.10363255932552,1.03387669758515,-5.48928700929849));
#11496=CARTESIAN_POINT('Ctrl Pts',(4.11364328508493,1.02835396742885,-5.49005653744723));
#11497=CARTESIAN_POINT('Ctrl Pts',(4.11883507683806,1.02543817875423,-5.49045870973892));
#11498=CARTESIAN_POINT('Ctrl Pts',(4.13234101291831,1.01771773643904,-5.49151312243515));
#11499=CARTESIAN_POINT('Ctrl Pts',(4.14061875806983,1.01285063177031,-5.49216757038399));
#11500=CARTESIAN_POINT('Ctrl Pts',(4.17545454986344,0.991790613991663,-5.49495741811053));
#11501=CARTESIAN_POINT('Ctrl Pts',(4.20142293523542,0.974651485641543,-5.49712657330734));
#11502=CARTESIAN_POINT('Ctrl Pts',(4.31101306282396,0.895921061803214,-5.50668454251924));
#11503=CARTESIAN_POINT('Ctrl Pts',(4.38695770417687,0.824451149262318,-5.51442809527893));
#11504=CARTESIAN_POINT('Ctrl Pts',(4.46626971605132,0.727118307275257,-5.52350995054909));
#11505=CARTESIAN_POINT('Ctrl Pts',(4.47953615140166,0.709884352673366,-5.52506848630949));
#11506=CARTESIAN_POINT('Ctrl Pts',(4.5003218346634,0.681277074820825,-5.5275649641275));
#11507=CARTESIAN_POINT('Ctrl Pts',(4.50813394512856,0.670123621807461,-5.52851688051838));
#11508=CARTESIAN_POINT('Ctrl Pts',(4.51842399668223,0.654876321188191,-5.52978700012526));
#11509=CARTESIAN_POINT('Ctrl Pts',(4.52107264542861,0.650899709609903,-5.53011544670346));
#11510=CARTESIAN_POINT('Ctrl Pts',(4.525447827731,0.644243485056328,-5.53066040453951));
#11511=CARTESIAN_POINT('Ctrl Pts',(4.5271877883482,0.641572822678699,-5.53087777782732));
#11512=CARTESIAN_POINT('Ctrl Pts',(4.53045924655372,0.636506617202525,-5.53128766930372));
#11513=CARTESIAN_POINT('Ctrl Pts',(4.53199294418861,0.634112542598711,-5.53148033514983));
#11514=CARTESIAN_POINT('Ctrl Pts',(4.53560148518286,0.628434510935416,-5.53193490482366));
#11515=CARTESIAN_POINT('Ctrl Pts',(4.53766879720479,0.62514577134661,-5.53219632333358));
#11516=CARTESIAN_POINT('Ctrl Pts',(4.54489631165479,0.613520776955705,-5.53311403632526));
#11517=CARTESIAN_POINT('Ctrl Pts',(4.5499688293379,0.605130102383565,-5.53376498722855));
#11518=CARTESIAN_POINT('Ctrl Pts',(4.59093069200686,0.53542170806235,-5.53908781609312));
#11519=CARTESIAN_POINT('Ctrl Pts',(4.62131379546568,0.471026319230465,-5.54347221653309));
#11520=CARTESIAN_POINT('Ctrl Pts',(4.66593766211988,0.348925689767928,-5.55151342141762));
#11521=CARTESIAN_POINT('Ctrl Pts',(4.68198248282185,0.292138107049691,-5.55515519603111));
#11522=CARTESIAN_POINT('Ctrl Pts',(4.6979351009883,0.213583911850137,-5.5602642443986));
#11523=CARTESIAN_POINT('Ctrl Pts',(4.70159687499713,0.192667804005683,-5.56163068907727));
#11524=CARTESIAN_POINT('Ctrl Pts',(4.70698232404128,0.156114205717943,-5.56403754091896));
#11525=CARTESIAN_POINT('Ctrl Pts',(4.70896178997384,0.140519683769094,-5.56507023063991));
#11526=CARTESIAN_POINT('Ctrl Pts',(4.71139165954182,0.117734631973119,-5.56658979084234));
#11527=CARTESIAN_POINT('Ctrl Pts',(4.7120891921917,0.110571761122995,-5.56706902122872));
#11528=CARTESIAN_POINT('Ctrl Pts',(4.71320212871983,0.0979444839358324,
-5.56791674287458));
#11529=CARTESIAN_POINT('Ctrl Pts',(4.7136451265351,0.0924826787972153,-5.56828436880864));
#11530=CARTESIAN_POINT('Ctrl Pts',(4.71448968572289,0.0810831956584553,
-5.56905372815509));
#11531=CARTESIAN_POINT('Ctrl Pts',(4.71488438850021,0.0751451810903372,
-5.56945566304316));
#11532=CARTESIAN_POINT('Ctrl Pts',(4.71579738451836,0.0596342999625881,
-5.57050876091953));
#11533=CARTESIAN_POINT('Ctrl Pts',(4.71624381656709,0.0500578097297874,
-5.57116212130397));
#11534=CARTESIAN_POINT('Ctrl Pts',(4.71763718277229,0.00953948035335322,
-5.5739405839824));
#11535=CARTESIAN_POINT('Ctrl Pts',(4.71748084156572,-0.0214254082874622,
-5.57609909750216));
#11536=CARTESIAN_POINT('Ctrl Pts',(4.71241285210513,-0.135339396400184,
-5.58417444206101));
#11537=CARTESIAN_POINT('Ctrl Pts',(4.69994979858721,-0.217701048469125,
-5.59029772181375));
#11538=CARTESIAN_POINT('Ctrl Pts',(4.66573224543815,-0.348509682531906,
-5.60019532681509));
#11539=CARTESIAN_POINT('Ctrl Pts',(4.64919481134619,-0.39804040616317,-5.6039791475489));
#11540=CARTESIAN_POINT('Ctrl Pts',(4.62678942015821,-0.452754462394137,
-5.60809134848805));
#11541=CARTESIAN_POINT('Ctrl Pts',(4.62409600643031,-0.459169132747586,
-5.60857233143898));
#11542=CARTESIAN_POINT('Ctrl Pts',(4.61989871430554,-0.468922430823454,
-5.60930151450108));
#11543=CARTESIAN_POINT('Ctrl Pts',(4.61843590318965,-0.472278403055192,
-5.60955202705499));
#11544=CARTESIAN_POINT('Ctrl Pts',(4.61572915396957,-0.478409998010614,
-5.61000894561765));
#11545=CARTESIAN_POINT('Ctrl Pts',(4.61449010808012,-0.481187633692278,
-5.61021562749309));
#11546=CARTESIAN_POINT('Ctrl Pts',(4.61166844272129,-0.487447817537524,
-5.61068077477072));
#11547=CARTESIAN_POINT('Ctrl Pts',(4.61007960850839,-0.490927476041106,
-5.61093886213976));
#11548=CARTESIAN_POINT('Ctrl Pts',(4.60592903017717,-0.499901557667233,
-5.61160343808227));
#11549=CARTESIAN_POINT('Ctrl Pts',(4.60334172924343,-0.505384135208795,
-5.61200844315704));
#11550=CARTESIAN_POINT('Ctrl Pts',(4.58568560902857,-0.542061587197846,
-5.6147126877148));
#11551=CARTESIAN_POINT('Ctrl Pts',(4.56928747413064,-0.5726017214246,-5.61693937957217));
#11552=CARTESIAN_POINT('Ctrl Pts',(4.53712998081129,-0.62662908446548,-5.62091221103024));
#11553=CARTESIAN_POINT('Ctrl Pts',(4.52182749215795,-0.650355152412231,
-5.62266953486143));
#11554=CARTESIAN_POINT('Ctrl Pts',(4.47825271446647,-0.712864378237065,
-5.62739396113424));
#11555=CARTESIAN_POINT('Ctrl Pts',(4.44844014040838,-0.750505744939403,
-5.63034410841217));
#11556=CARTESIAN_POINT('Ctrl Pts',(4.38081643216606,-0.825928274920015,
-5.63667888365917));
#11557=CARTESIAN_POINT('Ctrl Pts',(4.3425662536174,-0.86316447177844,-5.64006883885905));
#11558=CARTESIAN_POINT('Ctrl Pts',(4.29367360988861,-0.9046895931212,-5.64428484399493));
#11559=CARTESIAN_POINT('Ctrl Pts',(4.28532264179532,-0.911586172443673,
-5.64500100448675));
#11560=CARTESIAN_POINT('Ctrl Pts',(4.27202653094454,-0.922261656382174,
-5.64613580920986));
#11561=CARTESIAN_POINT('Ctrl Pts',(4.26714437954487,-0.926118323848458,
-5.6465513647534));
#11562=CARTESIAN_POINT('Ctrl Pts',(4.25794669162269,-0.933266436718698,
-5.6473322780599));
#11563=CARTESIAN_POINT('Ctrl Pts',(4.2536384990577,-0.936567097937192,-5.64769726197379));
#11564=CARTESIAN_POINT('Ctrl Pts',(4.24394208786454,-0.943890066386496,
-5.64851704790031));
#11565=CARTESIAN_POINT('Ctrl Pts',(4.23854196243696,-0.947896217072016,
-5.64897245759095));
#11566=CARTESIAN_POINT('Ctrl Pts',(4.22471328612309,-0.957972759821006,
-5.65013594436673));
#11567=CARTESIAN_POINT('Ctrl Pts',(4.21623833684439,-0.963978186788384,
-5.65084645119532));
#11568=CARTESIAN_POINT('Ctrl Pts',(4.16618808175879,-0.998458963888642,
-5.65502879908426));
#11569=CARTESIAN_POINT('Ctrl Pts',(4.12292517028468,-1.02433651174554,-5.65859284907271));
#11570=CARTESIAN_POINT('Ctrl Pts',(4.07816910321358,-1.04735437323224,-5.66222605418069));
#11571=CARTESIAN_POINT('Origin',(3.53951905042299,8.32667268468867E-16,
0.924367114736157));
#11572=CARTESIAN_POINT('',(4.07816929763934,-1.04735427323984,-6.26232527378825));
#11573=CARTESIAN_POINT('',(4.07816926754759,-1.04735428871591,-6.16392277459278));
#11574=CARTESIAN_POINT('',(4.07816926754759,-1.04735428871592,0.924367114736157));
#11575=CARTESIAN_POINT('',(2.36176914596391,-0.00047439080146823,-5.92346349896571));
#11576=CARTESIAN_POINT('Ctrl Pts',(4.07816929763934,-1.04735427323984,-6.26232527378825));
#11577=CARTESIAN_POINT('Ctrl Pts',(4.09023496895785,-1.0411489452008,-6.26135474120664));
#11578=CARTESIAN_POINT('Ctrl Pts',(4.10219477249534,-1.03473442025141,-6.26037854515567));
#11579=CARTESIAN_POINT('Ctrl Pts',(4.15591265580702,-1.00471610897298,-6.25593093081369));
#11580=CARTESIAN_POINT('Ctrl Pts',(4.19631180554023,-0.978784133249123,
-6.25240843958408));
#11581=CARTESIAN_POINT('Ctrl Pts',(4.25778352792731,-0.933802532810267,
-6.24681982066333));
#11582=CARTESIAN_POINT('Ctrl Pts',(4.27994647057524,-0.91632873992709,-6.24475351838742));
#11583=CARTESIAN_POINT('Ctrl Pts',(4.32788019253289,-0.87566097856935,-6.24019587139681));
#11584=CARTESIAN_POINT('Ctrl Pts',(4.35330024887309,-0.852089253740686,
-6.23771698249531));
#11585=CARTESIAN_POINT('Ctrl Pts',(4.38190563252322,-0.823114006289329,
-6.23488695704736));
#11586=CARTESIAN_POINT('Ctrl Pts',(4.38613184606868,-0.818766510776791,
-6.23446775457701));
#11587=CARTESIAN_POINT('Ctrl Pts',(4.39296976965588,-0.811622799150122,
-6.23378798835348));
#11588=CARTESIAN_POINT('Ctrl Pts',(4.39560169710329,-0.80884621613251,-6.23352597489406));
#11589=CARTESIAN_POINT('Ctrl Pts',(4.40030201720195,-0.80383891424895,-6.23305746059494));
#11590=CARTESIAN_POINT('Ctrl Pts',(4.40237533328976,-0.801612968778922,
-6.23285059601951));
#11591=CARTESIAN_POINT('Ctrl Pts',(4.4069252862916,-0.796689959333669,-6.2323961786076));
#11592=CARTESIAN_POINT('Ctrl Pts',(4.4093979823794,-0.793989366412672,-6.23214891738346));
#11593=CARTESIAN_POINT('Ctrl Pts',(4.41653319784795,-0.786123189220053,
-6.23143437434541));
#11594=CARTESIAN_POINT('Ctrl Pts',(4.42116268032956,-0.780927652881034,
-6.23096945458401));
#11595=CARTESIAN_POINT('Ctrl Pts',(4.46012823840423,-0.736409518276674,
-6.22704195826365));
#11596=CARTESIAN_POINT('Ctrl Pts',(4.49186557160994,-0.694879719389327,
-6.22374591948965));
#11597=CARTESIAN_POINT('Ctrl Pts',(4.56675906252071,-0.582060826952844,
-6.21531085374561));
#11598=CARTESIAN_POINT('Ctrl Pts',(4.60529671783504,-0.508069307664121,
-6.21024808736332));
#11599=CARTESIAN_POINT('Ctrl Pts',(4.64697982004174,-0.401963480249736,
-6.20297687442576));
#11600=CARTESIAN_POINT('Ctrl Pts',(4.65711327379942,-0.372863100348872,
-6.20098400327493));
#11601=CARTESIAN_POINT('Ctrl Pts',(4.66888478841956,-0.334244986214066,
-6.19832333086072));
#11602=CARTESIAN_POINT('Ctrl Pts',(4.6715638691723,-0.325055688189363,-6.19768909172239));
#11603=CARTESIAN_POINT('Ctrl Pts',(4.67572577032009,-0.310104395832672,
-6.19665487016446));
#11604=CARTESIAN_POINT('Ctrl Pts',(4.67727749371054,-0.304361904951789,
-6.19625710304884));
#11605=CARTESIAN_POINT('Ctrl Pts',(4.68017547767282,-0.293305348078831,
-6.19549008695273));
#11606=CARTESIAN_POINT('Ctrl Pts',(4.68152827126876,-0.287993142276344,
-6.19512105771836));
#11607=CARTESIAN_POINT('Ctrl Pts',(4.6845734084807,-0.275676450108379,-6.19426416495626));
#11608=CARTESIAN_POINT('Ctrl Pts',(4.68623863507582,-0.268665550882278,
-6.19377545438209));
#11609=CARTESIAN_POINT('Ctrl Pts',(4.69134182081782,-0.24626800761427,-6.19221091107657));
#11610=CARTESIAN_POINT('Ctrl Pts',(4.6945350807744,-0.230827974661903,-6.19112744335127));
#11611=CARTESIAN_POINT('Ctrl Pts',(4.70131415070436,-0.194374599057004,
-6.18855664629942));
#11612=CARTESIAN_POINT('Ctrl Pts',(4.70464120747205,-0.173319362174652,
-6.18706183393518));
#11613=CARTESIAN_POINT('Ctrl Pts',(4.7150620447811,-0.0933500990174083,
-6.18134660387077));
#11614=CARTESIAN_POINT('Ctrl Pts',(4.71827113560712,-0.0340245659343623,
-6.17702383848102));
#11615=CARTESIAN_POINT('Ctrl Pts',(4.71548489131035,0.0957328978677734,
-6.16750274731688));
#11616=CARTESIAN_POINT('Ctrl Pts',(4.70765258143186,0.165910477065057,-6.16230951768129));
#11617=CARTESIAN_POINT('Ctrl Pts',(4.69163089455348,0.24460159325757,-6.15668100972105));
#11618=CARTESIAN_POINT('Ctrl Pts',(4.68954969955024,0.254206928685382,-6.15599752700367));
#11619=CARTESIAN_POINT('Ctrl Pts',(4.68647754975801,0.267575003137327,-6.15505230289059));
#11620=CARTESIAN_POINT('Ctrl Pts',(4.68558789099588,0.271360268355784,-6.15478533128826));
#11621=CARTESIAN_POINT('Ctrl Pts',(4.6840149862692,0.277906829739487,-6.15432485924397));
#11622=CARTESIAN_POINT('Ctrl Pts',(4.68334046006642,0.280670155991929,-6.15413087961108));
#11623=CARTESIAN_POINT('Ctrl Pts',(4.68188897747402,0.286524289739774,-6.15372079270956));
#11624=CARTESIAN_POINT('Ctrl Pts',(4.68110947314463,0.289614443884628,-6.15350483651458));
#11625=CARTESIAN_POINT('Ctrl Pts',(4.67913101803897,0.297325435688441,-6.15296714395954));
#11626=CARTESIAN_POINT('Ctrl Pts',(4.67791648259323,0.301942278955648,-6.15264628015004));
#11627=CARTESIAN_POINT('Ctrl Pts',(4.67313872392961,0.319665394521243,-6.15141822327237));
#11628=CARTESIAN_POINT('Ctrl Pts',(4.66937680094446,0.332717644775483,-6.15052156033705));
#11629=CARTESIAN_POINT('Ctrl Pts',(4.65902984375411,0.366415212227218,-6.1482197691367));
#11630=CARTESIAN_POINT('Ctrl Pts',(4.65209919136348,0.386949698220904,-6.14683005916396));
#11631=CARTESIAN_POINT('Ctrl Pts',(4.60911685662259,0.503574401638551,-6.13895045862899));
#11632=CARTESIAN_POINT('Ctrl Pts',(4.56119542337881,0.594816078070128,-6.13279828597343));
#11633=CARTESIAN_POINT('Ctrl Pts',(4.48350324151432,0.704999917821411,-6.12421250578414));
#11634=CARTESIAN_POINT('Ctrl Pts',(4.46388623566266,0.730531351248177,-6.12213273950298));
#11635=CARTESIAN_POINT('Ctrl Pts',(4.43701588978873,0.762685381098157,-6.11937209760121));
#11636=CARTESIAN_POINT('Ctrl Pts',(4.43069016383441,0.770067272730883,-6.11872811227026));
#11637=CARTESIAN_POINT('Ctrl Pts',(4.42032615549249,0.781862954258344,-6.11768192736207));
#11638=CARTESIAN_POINT('Ctrl Pts',(4.41634427080329,0.786325865183131,-6.11728204072387));
#11639=CARTESIAN_POINT('Ctrl Pts',(4.40865468574665,0.794813344171872,-6.11651359743817));
#11640=CARTESIAN_POINT('Ctrl Pts',(4.40495258268798,0.798842790642308,-6.11614528005657));
#11641=CARTESIAN_POINT('Ctrl Pts',(4.39635859647735,0.808066808883381,-6.11529394186543));
#11642=CARTESIAN_POINT('Ctrl Pts',(4.39144735827215,0.813242970894683,-6.11481010939629));
#11643=CARTESIAN_POINT('Ctrl Pts',(4.37580358012886,0.829433387577266,-6.11327710661366));
#11644=CARTESIAN_POINT('Ctrl Pts',(4.36490255654542,0.840281850415247,-6.11222072910309));
#11645=CARTESIAN_POINT('Ctrl Pts',(4.33888443132437,0.865179654213928,-6.10972547856839));
#11646=CARTESIAN_POINT('Ctrl Pts',(4.3236046633512,0.879050913690368,-6.10827970605825));
#11647=CARTESIAN_POINT('Ctrl Pts',(4.26546839620884,0.929106010391572,-6.10284944527884));
#11648=CARTESIAN_POINT('Ctrl Pts',(4.22041258014362,0.962612682667298,-6.0987735335591));
#11649=CARTESIAN_POINT('Ctrl Pts',(4.1096343323993,1.03331533686176,-6.08914023447894));
#11650=CARTESIAN_POINT('Ctrl Pts',(4.04237379823384,1.06766615234464,-6.08357204699742));
#11651=CARTESIAN_POINT('Ctrl Pts',(3.96341105184678,1.09886383412478,-6.07762477296247));
#11652=CARTESIAN_POINT('Ctrl Pts',(3.95449185959204,1.10226300714134,-6.07696125378353));
#11653=CARTESIAN_POINT('Ctrl Pts',(3.94191009331509,1.10688364268902,-6.07603775020791));
#11654=CARTESIAN_POINT('Ctrl Pts',(3.93828162347891,1.10819599405154,-6.07577286621487));
#11655=CARTESIAN_POINT('Ctrl Pts',(3.93170860778717,1.11053687056379,-6.07529571892222));
#11656=CARTESIAN_POINT('Ctrl Pts',(3.92876630647829,1.11157157405482,-6.0750831035106));
#11657=CARTESIAN_POINT('Ctrl Pts',(3.92273494563442,1.11366570574782,-6.07464930181903));
#11658=CARTESIAN_POINT('Ctrl Pts',(3.91964553633732,1.11472399358168,-6.07442818176472));
#11659=CARTESIAN_POINT('Ctrl Pts',(3.91168450935162,1.11741412574173,-6.07386107016147));
#11660=CARTESIAN_POINT('Ctrl Pts',(3.90680648024522,1.11902698963564,-6.073516160187));
#11661=CARTESIAN_POINT('Ctrl Pts',(3.88614866036797,1.12570762334384,-6.07206577415419));
#11662=CARTESIAN_POINT('Ctrl Pts',(3.87027250288145,1.13047421978312,-6.07097632146394));
#11663=CARTESIAN_POINT('Ctrl Pts',(3.826501935294,1.14261457581979,-6.06802788090749));
#11664=CARTESIAN_POINT('Ctrl Pts',(3.7984279121614,1.1493013873189,-6.06619729594464));
#11665=CARTESIAN_POINT('Ctrl Pts',(3.68173355665175,1.17260243035188,-6.05873226487686));
#11666=CARTESIAN_POINT('Ctrl Pts',(3.59160002312312,1.18004638063982,-6.05328081782732));
#11667=CARTESIAN_POINT('Ctrl Pts',(3.4681031231792,1.17605748836533,-6.045422827928));
#11668=CARTESIAN_POINT('Ctrl Pts',(3.4347719003372,1.17355833482817,-6.04326617553621));
#11669=CARTESIAN_POINT('Ctrl Pts',(3.39180236078252,1.16849135846763,-6.0404165623393));
#11670=CARTESIAN_POINT('Ctrl Pts',(3.3820256921699,1.16721382258042,-6.03976356927852));
#11671=CARTESIAN_POINT('Ctrl Pts',(3.36631614842783,1.16496006459645,-6.03870632271181));
#11672=CARTESIAN_POINT('Ctrl Pts',(3.36037256105679,1.16406087918425,-6.03830447385833));
#11673=CARTESIAN_POINT('Ctrl Pts',(3.34904024132537,1.16225760463174,-6.03753464015022));
#11674=CARTESIAN_POINT('Ctrl Pts',(3.34365039319316,1.16136143539783,-6.03716691226133));
#11675=CARTESIAN_POINT('Ctrl Pts',(3.33129718361274,1.15921902887461,-6.03632037491132));
#11676=CARTESIAN_POINT('Ctrl Pts',(3.32433848119451,1.15794750380657,-6.03584078445057));
#11677=CARTESIAN_POINT('Ctrl Pts',(3.30261535686581,1.1537755840954,-6.03433486591795));
#11678=CARTESIAN_POINT('Ctrl Pts',(3.2878952924871,1.15065499026485,-6.03330168788211));
#11679=CARTESIAN_POINT('Ctrl Pts',(3.25370060041941,1.14271834499085,-6.0308707016088));
#11680=CARTESIAN_POINT('Ctrl Pts',(3.23428168918236,1.13768513816858,-6.02946646928371));
#11681=CARTESIAN_POINT('Ctrl Pts',(3.16362062670901,1.11743114227027,-6.02426876592153));
#11682=CARTESIAN_POINT('Ctrl Pts',(3.11330712790216,1.09922438801772,-6.02039227058267));
#11683=CARTESIAN_POINT('Ctrl Pts',(2.99166532473383,1.04559622403568,-6.01065627823979));
#11684=CARTESIAN_POINT('Ctrl Pts',(2.92235092134621,1.00624083082896,-6.0047678923588));
#11685=CARTESIAN_POINT('Ctrl Pts',(2.84981253488101,0.954719600240245,-5.99853975550467));
#11686=CARTESIAN_POINT('Ctrl Pts',(2.8421643027805,0.949147492627594,-5.99788240316152));
#11687=CARTESIAN_POINT('Ctrl Pts',(2.83159398420192,0.941249750043009,-5.99697387005026));
#11688=CARTESIAN_POINT('Ctrl Pts',(2.82861479137434,0.939001664940125,-5.99671780099785));
#11689=CARTESIAN_POINT('Ctrl Pts',(2.82319119836403,0.934868439340018,-5.99625169877643));
#11690=CARTESIAN_POINT('Ctrl Pts',(2.82074342770127,0.932987778897274,-5.99604136490264));
#11691=CARTESIAN_POINT('Ctrl Pts',(2.81573090290748,0.929105142132876,-5.9956107426378));
#11692=CARTESIAN_POINT('Ctrl Pts',(2.81316701755263,0.927102137100601,-5.99539052778835));
#11693=CARTESIAN_POINT('Ctrl Pts',(2.80673448666815,0.922033734680722,-5.99483805452521));
#11694=CARTESIAN_POINT('Ctrl Pts',(2.80287670380741,0.918954558221804,-5.99450674135558));
#11695=CARTESIAN_POINT('Ctrl Pts',(2.7943208730998,0.912037028173135,-5.9937717092654));
#11696=CARTESIAN_POINT('Ctrl Pts',(2.78963286005736,0.908186417749585,-5.99336879662046));
#11697=CARTESIAN_POINT('Ctrl Pts',(2.77586143854283,0.896695593604447,-5.99218400117474));
#11698=CARTESIAN_POINT('Ctrl Pts',(2.76686326791718,0.888953880141247,-5.99140828875435));
#11699=CARTESIAN_POINT('Ctrl Pts',(2.73421665808705,0.859995584259759,-5.988581418607));
#11700=CARTESIAN_POINT('Ctrl Pts',(2.71131096530185,0.837959430794632,-5.98657319649999));
#11701=CARTESIAN_POINT('Ctrl Pts',(2.67160936435353,0.796544441714306,-5.98298600219773));
#11702=CARTESIAN_POINT('Ctrl Pts',(2.65450251521094,0.777493446020089,-5.98140049337148));
#11703=CARTESIAN_POINT('Ctrl Pts',(2.58361082598284,0.693170820613504,-5.97458445170998));
#11704=CARTESIAN_POINT('Ctrl Pts',(2.53632793676492,0.62277750278925,-5.96937011291797));
#11705=CARTESIAN_POINT('Ctrl Pts',(2.48996839576904,0.534571163312495,-5.9628743519718));
#11706=CARTESIAN_POINT('Ctrl Pts',(2.48320368584932,0.521076503303184,-5.96188227556779));
#11707=CARTESIAN_POINT('Ctrl Pts',(2.47363591261027,0.501037708494094,-5.96040966482948));
#11708=CARTESIAN_POINT('Ctrl Pts',(2.47062965804543,0.494591864024867,-5.95993606199502));
#11709=CARTESIAN_POINT('Ctrl Pts',(2.46540835448122,0.483126661858874,-5.959093626612));
#11710=CARTESIAN_POINT('Ctrl Pts',(2.46316962898218,0.478118269640409,-5.95872560912309));
#11711=CARTESIAN_POINT('Ctrl Pts',(2.45858173133207,0.467658856001614,-5.95795693048653));
#11712=CARTESIAN_POINT('Ctrl Pts',(2.45623861849636,0.462205362346718,-5.95755607780845));
#11713=CARTESIAN_POINT('Ctrl Pts',(2.45024788695567,0.447966385887117,-5.95650915875833));
#11714=CARTESIAN_POINT('Ctrl Pts',(2.44666536934578,0.439154156302012,-5.95586094303869));
#11715=CARTESIAN_POINT('Ctrl Pts',(2.43094374827078,0.399098195333223,-5.95291243462964));
#11716=CARTESIAN_POINT('Ctrl Pts',(2.42003614690547,0.367391088674902,-5.95057225856815));
#11717=CARTESIAN_POINT('Ctrl Pts',(2.37812953154315,0.226268154702565,-5.94012295799659));
#11718=CARTESIAN_POINT('Ctrl Pts',(2.3617233639395,0.113186697719935,-5.93158837563074));
#11719=CARTESIAN_POINT('Ctrl Pts',(2.36176914596391,-0.00047439080146823,
-5.92346349896571));
#11720=CARTESIAN_POINT('Ctrl Pts',(2.36176914658663,-0.000475934275394455,
-5.92346338863304));
#11721=CARTESIAN_POINT('Ctrl Pts',(2.36177760495954,-0.0214070762438138,
-5.92196716112806));
#11722=CARTESIAN_POINT('Ctrl Pts',(2.3623440511716,-0.0423361050014404,
-5.92048893771383));
#11723=CARTESIAN_POINT('Ctrl Pts',(2.36370274366909,-0.0676029612356144,
-5.91873422110888));
#11724=CARTESIAN_POINT('Ctrl Pts',(2.36396159790513,-0.0719640527127362,
-5.91843243505327));
#11725=CARTESIAN_POINT('Ctrl Pts',(2.36444920185137,-0.0794724480462547,
-5.91791483065283));
#11726=CARTESIAN_POINT('Ctrl Pts',(2.36466634244599,-0.0826204221579617,
-5.91769841766443));
#11727=CARTESIAN_POINT('Ctrl Pts',(2.36510396526883,-0.0886138533579433,
-5.91728757574057));
#11728=CARTESIAN_POINT('Ctrl Pts',(2.36532214384525,-0.0914594575013904,
-5.91709302330615));
#11729=CARTESIAN_POINT('Ctrl Pts',(2.36577866569802,-0.0971425736467546,
-5.91670552777087));
#11730=CARTESIAN_POINT('Ctrl Pts',(2.36601695921495,-0.0999800616037671,
-5.91651258241162));
#11731=CARTESIAN_POINT('Ctrl Pts',(2.36660605016895,-0.106702248326651,
-5.91605666773188));
#11732=CARTESIAN_POINT('Ctrl Pts',(2.36696586203937,-0.110586153962821,
-5.91579419050447));
#11733=CARTESIAN_POINT('Ctrl Pts',(2.36829937255023,-0.124241523053148,
-5.9148744267966));
#11734=CARTESIAN_POINT('Ctrl Pts',(2.36937600734381,-0.134002850878811,
-5.91422249313009));
#11735=CARTESIAN_POINT('Ctrl Pts',(2.37355925964272,-0.168020178416457,
-5.91196636331695));
#11736=CARTESIAN_POINT('Ctrl Pts',(2.37729923935332,-0.192193396399408,
-5.91039118992659));
#11737=CARTESIAN_POINT('Ctrl Pts',(2.40079692035164,-0.318001176972263,
-5.90225943617596));
#11738=CARTESIAN_POINT('Ctrl Pts',(2.43313902489403,-0.416819604865689,
-5.89605944901046));
#11739=CARTESIAN_POINT('Ctrl Pts',(2.48765961102549,-0.530269248192219,
-5.88805173051619));
#11740=CARTESIAN_POINT('Ctrl Pts',(2.49790247751019,-0.550116877253475,
-5.88661677915914));
#11741=CARTESIAN_POINT('Ctrl Pts',(2.51660560100441,-0.583960689153967,
-5.88410043890528));
#11742=CARTESIAN_POINT('Ctrl Pts',(2.52480471413348,-0.598094294283077,
-5.88302779575204));
#11743=CARTESIAN_POINT('Ctrl Pts',(2.53709281764408,-0.618296143640833,
-5.88146028177884));
#11744=CARTESIAN_POINT('Ctrl Pts',(2.54094873935566,-0.624504446131463,
-5.88097376278203));
#11745=CARTESIAN_POINT('Ctrl Pts',(2.54780566233151,-0.635318687087124,
-5.88011762402527));
#11746=CARTESIAN_POINT('Ctrl Pts',(2.55078162628431,-0.639940296155991,
-5.87974892570641));
#11747=CARTESIAN_POINT('Ctrl Pts',(2.55662808426741,-0.648881583288878,
-5.87903003201151));
#11748=CARTESIAN_POINT('Ctrl Pts',(2.55949497838933,-0.653203473072743,
-5.87867997564401));
#11749=CARTESIAN_POINT('Ctrl Pts',(2.56725086968374,-0.664729606458764,
-5.87773940284533));
#11750=CARTESIAN_POINT('Ctrl Pts',(2.57219128532318,-0.671898692357601,
-5.87714698042595));
#11751=CARTESIAN_POINT('Ctrl Pts',(2.5909084968569,-0.698425065503021,-5.87492668849393));
#11752=CARTESIAN_POINT('Ctrl Pts',(2.60518974233784,-0.717417701090581,
-5.87327993452043));
#11753=CARTESIAN_POINT('Ctrl Pts',(2.68302084173491,-0.814656754862096,
-5.86453738217128));
#11754=CARTESIAN_POINT('Ctrl Pts',(2.75584210404748,-0.884928640498914,
-5.857073789571));
#11755=CARTESIAN_POINT('Ctrl Pts',(2.86061040135281,-0.962842778902455,
-5.84755154736277));
#11756=CARTESIAN_POINT('Ctrl Pts',(2.88519171118066,-0.97971380636161,-5.84539549744997));
#11757=CARTESIAN_POINT('Ctrl Pts',(2.92001481048248,-1.00171814184796,-5.84247078212881));
#11758=CARTESIAN_POINT('Ctrl Pts',(2.9297296395284,-1.00766146832375,-5.8416682503467));
#11759=CARTESIAN_POINT('Ctrl Pts',(2.94460103162576,-1.01646561578382,-5.84046157248804));
#11760=CARTESIAN_POINT('Ctrl Pts',(2.94969512219012,-1.01943000458922,-5.84005205394333));
#11761=CARTESIAN_POINT('Ctrl Pts',(2.9591083372682,-1.02481362690101,-5.83930260876271));
#11762=CARTESIAN_POINT('Ctrl Pts',(2.96342084733076,-1.02724409387685,-5.83896204622149));
#11763=CARTESIAN_POINT('Ctrl Pts',(2.97051545957373,-1.03118378185554,-5.83840648308147));
#11764=CARTESIAN_POINT('Ctrl Pts',(2.97328849428612,-1.03270907629403,-5.83819050175509));
#11765=CARTESIAN_POINT('Ctrl Pts',(2.97880193514254,-1.03571283388441,-5.83776344437208));
#11766=CARTESIAN_POINT('Ctrl Pts',(2.98154210170897,-1.03719163257148,-5.83755235284934));
#11767=CARTESIAN_POINT('Ctrl Pts',(2.98767350633388,-1.04046926614404,-5.83708251675237));
#11768=CARTESIAN_POINT('Ctrl Pts',(2.99106777168128,-1.04226244017224,-5.83682412112084));
#11769=CARTESIAN_POINT('Ctrl Pts',(3.00283071737263,-1.04840337248369,-5.83593428939906));
#11770=CARTESIAN_POINT('Ctrl Pts',(3.0112430742722,-1.05266732875569,-5.8353077539383));
#11771=CARTESIAN_POINT('Ctrl Pts',(3.08887096324529,-1.09084942727537,-5.8296075090175));
#11772=CARTESIAN_POINT('Ctrl Pts',(3.16121893189687,-1.11800208080267,-5.82487561105016));
#11773=CARTESIAN_POINT('Ctrl Pts',(3.28881424901934,-1.15206908925458,-5.81670538909766));
#11774=CARTESIAN_POINT('Ctrl Pts',(3.3428424701339,-1.16251183834201,-5.81329723741568));
#11775=CARTESIAN_POINT('Ctrl Pts',(3.41764273791609,-1.17160449562992,-5.80848750862781));
#11776=CARTESIAN_POINT('Ctrl Pts',(3.4379460894029,-1.17353900279816,-5.80717339832075));
#11777=CARTESIAN_POINT('Ctrl Pts',(3.47349188199594,-1.1759964798411,-5.80485053102374));
#11778=CARTESIAN_POINT('Ctrl Pts',(3.48871354951401,-1.17675234184652,-5.80384875230846));
#11779=CARTESIAN_POINT('Ctrl Pts',(3.51105154830254,-1.17742737026895,-5.80236631673948));
#11780=CARTESIAN_POINT('Ctrl Pts',(3.51815971165065,-1.17757776213472,-5.80189277018669));
#11781=CARTESIAN_POINT('Ctrl Pts',(3.53073679420862,-1.17772995173204,-5.80105146650971));
#11782=CARTESIAN_POINT('Ctrl Pts',(3.53620523001797,-1.17775803291908,-5.80068453068911));
#11783=CARTESIAN_POINT('Ctrl Pts',(3.54766698721581,-1.17773706514276,-5.79991295324079));
#11784=CARTESIAN_POINT('Ctrl Pts',(3.55366012036343,-1.17768035193621,-5.79950808550401));
#11785=CARTESIAN_POINT('Ctrl Pts',(3.5694290271699,-1.17741074604027,-5.79843893338811));
#11786=CARTESIAN_POINT('Ctrl Pts',(3.57920286343207,-1.17712185290534,-5.79777232709906));
#11787=CARTESIAN_POINT('Ctrl Pts',(3.62164878129819,-1.17533801354753,-5.79485958774397));
#11788=CARTESIAN_POINT('Ctrl Pts',(3.65425141888492,-1.17260430804531,-5.79257589995079));
#11789=CARTESIAN_POINT('Ctrl Pts',(3.77690513087472,-1.15715590298647,-5.78380345109363));
#11790=CARTESIAN_POINT('Ctrl Pts',(3.86548866471428,-1.1353862014243,-5.7770655728495));
#11791=CARTESIAN_POINT('Ctrl Pts',(3.97776758578952,-1.09355815475573,-5.76833328612069));
#11792=CARTESIAN_POINT('Ctrl Pts',(4.004485597182,-1.08246826768167,-5.76624314554824));
#11793=CARTESIAN_POINT('Ctrl Pts',(4.04585689750954,-1.06348136172682,-5.76301293255282));
#11794=CARTESIAN_POINT('Ctrl Pts',(4.06079680188451,-1.05623870290635,-5.76184783550009));
#11795=CARTESIAN_POINT('Ctrl Pts',(4.0764432923149,-1.04824060315226,-5.76063280410153));
#11796=CARTESIAN_POINT('Ctrl Pts',(4.0773065526916,-1.04779797959445,-5.76056578435822));
#11797=CARTESIAN_POINT('Ctrl Pts',(4.07816926754817,-1.04735428871561,-5.76049882461148));
#11798=CARTESIAN_POINT('Ctrl Pts',(4.07816910321358,-1.04735437323224,-5.66222605418069));
#11799=CARTESIAN_POINT('Ctrl Pts',(4.05590441778445,-1.05880500950996,-5.66403345536945));
#11800=CARTESIAN_POINT('Ctrl Pts',(4.033270176812,-1.06954797620782,-5.66585731820949));
#11801=CARTESIAN_POINT('Ctrl Pts',(3.9573207630993,-1.10266827073946,-5.67191846171575));
#11802=CARTESIAN_POINT('Ctrl Pts',(3.90271247636352,-1.12184061798517,-5.67618723591131));
#11803=CARTESIAN_POINT('Ctrl Pts',(3.82711691893152,-1.1422798301042,-5.68184226915528));
#11804=CARTESIAN_POINT('Ctrl Pts',(3.80717965346055,-1.14711535848151,-5.68331001265983));
#11805=CARTESIAN_POINT('Ctrl Pts',(3.7743595768206,-1.1541730742003,-5.68567759216775));
#11806=CARTESIAN_POINT('Ctrl Pts',(3.76154856302646,-1.15670587834702,-5.68658978412911));
#11807=CARTESIAN_POINT('Ctrl Pts',(3.74406989137212,-1.15986039142249,-5.68781577392829));
#11808=CARTESIAN_POINT('Ctrl Pts',(3.73943729280115,-1.16066785618203,-5.68813894950106));
#11809=CARTESIAN_POINT('Ctrl Pts',(3.73167211651291,-1.16197345975913,-5.68867756801459));
#11810=CARTESIAN_POINT('Ctrl Pts',(3.7285421777667,-1.16248672254725,-5.68889383240835));
#11811=CARTESIAN_POINT('Ctrl Pts',(3.72258971076087,-1.16343816075113,-5.68930347999926));
#11812=CARTESIAN_POINT('Ctrl Pts',(3.7197676104416,-1.16387872118291,-5.68949699901895));
#11813=CARTESIAN_POINT('Ctrl Pts',(3.71305224277283,-1.16490205181255,-5.68995589237857));
#11814=CARTESIAN_POINT('Ctrl Pts',(3.70915757036099,-1.1654755822497,-5.6902207589026));
#11815=CARTESIAN_POINT('Ctrl Pts',(3.69535119074833,-1.16743803917434,-5.69115541536521));
#11816=CARTESIAN_POINT('Ctrl Pts',(3.68542440026647,-1.16872018740007,-5.69181963129424));
#11817=CARTESIAN_POINT('Ctrl Pts',(3.61187920507642,-1.17726761440479,-5.69669105897549));
#11818=CARTESIAN_POINT('Ctrl Pts',(3.54777056232801,-1.17946136770664,-5.70066699475069));
#11819=CARTESIAN_POINT('Ctrl Pts',(3.42224438139773,-1.17351549179823,-5.70844565012187));
#11820=CARTESIAN_POINT('Ctrl Pts',(3.36102169153983,-1.16577445977327,-5.71223871160024));
#11821=CARTESIAN_POINT('Ctrl Pts',(3.27775688639229,-1.14853123257754,-5.71763875963724));
#11822=CARTESIAN_POINT('Ctrl Pts',(3.25497425519768,-1.14309998583426,-5.71914116522909));
#11823=CARTESIAN_POINT('Ctrl Pts',(3.21601702606997,-1.1325760135616,-5.72176469560425));
#11824=CARTESIAN_POINT('Ctrl Pts',(3.19976229474584,-1.12780640457901,-5.72287599154865));
#11825=CARTESIAN_POINT('Ctrl Pts',(3.17655096827304,-1.12044820307637,-5.72448967257269));
#11826=CARTESIAN_POINT('Ctrl Pts',(3.16950666430863,-1.11814168796561,-5.72498298655269));
#11827=CARTESIAN_POINT('Ctrl Pts',(3.15726230291476,-1.11400414252061,-5.72584695276355));
#11828=CARTESIAN_POINT('Ctrl Pts',(3.15205240373679,-1.11220279019376,-5.72621663024624));
#11829=CARTESIAN_POINT('Ctrl Pts',(3.14199452048952,-1.10864597316496,-5.72693439884319));
#11830=CARTESIAN_POINT('Ctrl Pts',(3.13714503210403,-1.10689511410968,-5.72728233184394));
#11831=CARTESIAN_POINT('Ctrl Pts',(3.12428634094326,-1.10215694432326,-5.72820992393417));
#11832=CARTESIAN_POINT('Ctrl Pts',(3.11629802369937,-1.09911422918797,-5.72879139469081));
#11833=CARTESIAN_POINT('Ctrl Pts',(3.08725966083902,-1.08769014304142,-5.73092464958761));
#11834=CARTESIAN_POINT('Ctrl Pts',(3.06642070778634,-1.07878924663544,-5.73249345498974));
#11835=CARTESIAN_POINT('Ctrl Pts',(2.95345433061729,-1.02663545059916,-5.74121409764393));
#11836=CARTESIAN_POINT('Ctrl Pts',(2.86698592534885,-0.972185419718714,
-5.74874716505658));
#11837=CARTESIAN_POINT('Ctrl Pts',(2.76540078565253,-0.888112378900456,
-5.7583665023148));
#11838=CARTESIAN_POINT('Ctrl Pts',(2.7429355093011,-0.868019349789785,-5.76054682250989));
#11839=CARTESIAN_POINT('Ctrl Pts',(2.71301598321759,-0.83911814188063,-5.76350094255396));
#11840=CARTESIAN_POINT('Ctrl Pts',(2.70488423859892,-0.831030281523895,
-5.76430927323719));
#11841=CARTESIAN_POINT('Ctrl Pts',(2.69096671686843,-0.816777469859977,
-5.76570035168024));
#11842=CARTESIAN_POINT('Ctrl Pts',(2.68512688463055,-0.810666722720063,
-5.76628646766268));
#11843=CARTESIAN_POINT('Ctrl Pts',(2.67664930214213,-0.801602475234878,
-5.7671402171437));
#11844=CARTESIAN_POINT('Ctrl Pts',(2.67396000801465,-0.798697862807326,
-5.76741148428987));
#11845=CARTESIAN_POINT('Ctrl Pts',(2.66924276954727,-0.793551130123568,
-5.76788799702388));
#11846=CARTESIAN_POINT('Ctrl Pts',(2.6672087551954,-0.79131469768356,-5.76809368788746));
#11847=CARTESIAN_POINT('Ctrl Pts',(2.66280634073862,-0.786436567107738,
-5.76853935997601));
#11848=CARTESIAN_POINT('Ctrl Pts',(2.66044125314773,-0.783791985527263,
-5.76877909930313));
#11849=CARTESIAN_POINT('Ctrl Pts',(2.65394142832779,-0.776457614236689,
-5.76943896328464));
#11850=CARTESIAN_POINT('Ctrl Pts',(2.64983195567053,-0.771745443220508,
-5.76985729155267));
#11851=CARTESIAN_POINT('Ctrl Pts',(2.62775640454187,-0.746021577465351,
-5.77211213630108));
#11852=CARTESIAN_POINT('Ctrl Pts',(2.61049529189164,-0.724413175764943,
-5.7739030850614));
#11853=CARTESIAN_POINT('Ctrl Pts',(2.54453804874295,-0.635603930868825,
-5.78095332906597));
#11854=CARTESIAN_POINT('Ctrl Pts',(2.50224156354834,-0.563947579280367,
-5.78597648144959));
#11855=CARTESIAN_POINT('Ctrl Pts',(2.44534065814713,-0.439099542260725,
-5.7945514377408));
#11856=CARTESIAN_POINT('Ctrl Pts',(2.42629130910713,-0.388275199489886,
-5.7979956957979));
#11857=CARTESIAN_POINT('Ctrl Pts',(2.40770688448018,-0.325905601496133,
-5.80227263997611));
#11858=CARTESIAN_POINT('Ctrl Pts',(2.40474700643433,-0.315445138389542,
-5.80299143874695));
#11859=CARTESIAN_POINT('Ctrl Pts',(2.40031923231351,-0.298927508463371,
-5.80412948282503));
#11860=CARTESIAN_POINT('Ctrl Pts',(2.39875383935721,-0.292896929999704,
-5.80454560931671));
#11861=CARTESIAN_POINT('Ctrl Pts',(2.39591473307706,-0.281591323858041,
-5.80532703057016));
#11862=CARTESIAN_POINT('Ctrl Pts',(2.39462948027629,-0.276319342077268,
-5.80569194683368));
#11863=CARTESIAN_POINT('Ctrl Pts',(2.39183610346387,-0.264507022519579,
-5.80651084102657));
#11864=CARTESIAN_POINT('Ctrl Pts',(2.39034737474615,-0.257962338919741,
-5.80696542067858));
#11865=CARTESIAN_POINT('Ctrl Pts',(2.38670593283457,-0.241296591596315,
-5.80812535161508));
#11866=CARTESIAN_POINT('Ctrl Pts',(2.38463054984694,-0.23115940083819,-5.80883310712443));
#11867=CARTESIAN_POINT('Ctrl Pts',(2.36870487123071,-0.147794703097492,
-5.8146729711907));
#11868=CARTESIAN_POINT('Ctrl Pts',(2.36170273807556,-0.0734445351739944,
-5.82002094522557));
#11869=CARTESIAN_POINT('Ctrl Pts',(2.36184042799039,0.0801506629869638,
-5.83125281056311));
#11870=CARTESIAN_POINT('Ctrl Pts',(2.36987871761785,0.159040563076637,-5.83712062759711));
#11871=CARTESIAN_POINT('Ctrl Pts',(2.38837836564954,0.249277888215904,-5.84361948445117));
#11872=CARTESIAN_POINT('Ctrl Pts',(2.39120252526141,0.261980027144235,-5.84452883310714));
#11873=CARTESIAN_POINT('Ctrl Pts',(2.39536585718711,0.279342047056117,-5.84576195026205));
#11874=CARTESIAN_POINT('Ctrl Pts',(2.39652402375803,0.284043799293962,-5.84609488965759));
#11875=CARTESIAN_POINT('Ctrl Pts',(2.39841798137968,0.291533401966075,-5.84662350512072));
#11876=CARTESIAN_POINT('Ctrl Pts',(2.39913505269272,0.294325860926441,-5.846820210163));
#11877=CARTESIAN_POINT('Ctrl Pts',(2.40065571714905,0.300158724722065,-5.84723023708367));
#11878=CARTESIAN_POINT('Ctrl Pts',(2.40146124377929,0.303198583381686,-5.84744343888796));
#11879=CARTESIAN_POINT('Ctrl Pts',(2.40346673775005,0.310646218766213,-5.84796466282368));
#11880=CARTESIAN_POINT('Ctrl Pts',(2.4046802092756,0.315050371696231,-5.84827192525692));
#11881=CARTESIAN_POINT('Ctrl Pts',(2.40920476308002,0.331106324480908,-5.84938894917187));
#11882=CARTESIAN_POINT('Ctrl Pts',(2.41267005334852,0.342714388728082,-5.85019046800396));
#11883=CARTESIAN_POINT('Ctrl Pts',(2.42187751144078,0.371906635869094,-5.85219562012209));
#11884=CARTESIAN_POINT('Ctrl Pts',(2.42785610046585,0.389413299306522,-5.85338836885609));
#11885=CARTESIAN_POINT('Ctrl Pts',(2.45689613768073,0.468320250347978,-5.85875035692082));
#11886=CARTESIAN_POINT('Ctrl Pts',(2.48465021012575,0.527872297016709,-5.86276331676315));
#11887=CARTESIAN_POINT('Ctrl Pts',(2.55238885172492,0.646285944922952,-5.87121994260289));
#11888=CARTESIAN_POINT('Ctrl Pts',(2.5930266930545,0.704458511257287,-5.87565894743985));
#11889=CARTESIAN_POINT('Ctrl Pts',(2.64536381751722,0.766609716498963,-5.88099099172694));
#11890=CARTESIAN_POINT('Ctrl Pts',(2.65219366545694,0.774504801667363,-5.88168005157804));
#11891=CARTESIAN_POINT('Ctrl Pts',(2.66360419031718,0.787345949712134,-5.8828209760035));
#11892=CARTESIAN_POINT('Ctrl Pts',(2.66812407855202,0.792345433830036,-5.88327034809631));
#11893=CARTESIAN_POINT('Ctrl Pts',(2.67636144668496,0.801301117765885,-5.88408489483804));
#11894=CARTESIAN_POINT('Ctrl Pts',(2.68006386816501,0.805270959508957,-5.88444943225166));
#11895=CARTESIAN_POINT('Ctrl Pts',(2.6880605541363,0.813727263512018,-5.88523352005582));
#11896=CARTESIAN_POINT('Ctrl Pts',(2.69236310996546,0.818205622248709,-5.88565341747766));
#11897=CARTESIAN_POINT('Ctrl Pts',(2.70422893034798,0.830362352117846,-5.88680622327996));
#11898=CARTESIAN_POINT('Ctrl Pts',(2.7118623365081,0.837971103938437,-5.88754215018546));
#11899=CARTESIAN_POINT('Ctrl Pts',(2.75707937586495,0.88182150167839,-5.89186994696998));
#11900=CARTESIAN_POINT('Ctrl Pts',(2.7969299043815,0.915631465178649,-5.89556310449824));
#11901=CARTESIAN_POINT('Ctrl Pts',(2.90014188769413,0.992017827517853,-5.90483582406355));
#11902=CARTESIAN_POINT('Ctrl Pts',(2.96564810248908,1.03129705080707,-5.9104882905964));
#11903=CARTESIAN_POINT('Ctrl Pts',(3.04780609670735,1.07029473326181,-5.91708805263446));
#11904=CARTESIAN_POINT('Ctrl Pts',(3.06124366046387,1.0763666318341,-5.91815230514171));
#11905=CARTESIAN_POINT('Ctrl Pts',(3.09549191005506,1.09107399361051,-5.92082122346563));
#11906=CARTESIAN_POINT('Ctrl Pts',(3.1164441601943,1.09936816319868,-5.92241416415505));
#11907=CARTESIAN_POINT('Ctrl Pts',(3.14320756721701,1.10908411229172,-5.92438837180267));
#11908=CARTESIAN_POINT('Ctrl Pts',(3.14880752163197,1.11106924394302,-5.92479815364328));
#11909=CARTESIAN_POINT('Ctrl Pts',(3.15767584750484,1.11413764092582,-5.92544164240144));
#11910=CARTESIAN_POINT('Ctrl Pts',(3.16093426437226,1.11524906414737,-5.92567691680511));
#11911=CARTESIAN_POINT('Ctrl Pts',(3.16711107838899,1.11732574164928,-5.92612066512895));
#11912=CARTESIAN_POINT('Ctrl Pts',(3.17002835871406,1.11829385205943,-5.92632929172806));
#11913=CARTESIAN_POINT('Ctrl Pts',(3.17689843847846,1.12054389525013,-5.92681841097791));
#11914=CARTESIAN_POINT('Ctrl Pts',(3.18085427700204,1.12181634459729,-5.92709835617977));
#11915=CARTESIAN_POINT('Ctrl Pts',(3.19390963362582,1.12593966075054,-5.92801694034282));
#11916=CARTESIAN_POINT('Ctrl Pts',(3.20303732410554,1.12870104577624,-5.92865069601643));
#11917=CARTESIAN_POINT('Ctrl Pts',(3.25454283755589,1.14360255588783,-5.93218464190927));
#11918=CARTESIAN_POINT('Ctrl Pts',(3.29754717982951,1.15346813387787,-5.93497612372975));
#11919=CARTESIAN_POINT('Ctrl Pts',(3.36850400898774,1.16560158873795,-5.93947185000744));
#11920=CARTESIAN_POINT('Ctrl Pts',(3.39615908020165,1.16932509941993,-5.941197200551));
#11921=CARTESIAN_POINT('Ctrl Pts',(3.50385170993643,1.17994661414321,-5.94789086714254));
#11922=CARTESIAN_POINT('Ctrl Pts',(3.58436942354338,1.1796324027728,-5.95285927334266));
#11923=CARTESIAN_POINT('Ctrl Pts',(3.67958241869871,1.16949384898834,-5.95909945158123));
#11924=CARTESIAN_POINT('Ctrl Pts',(3.69490630658036,1.16755658304031,-5.96011448456682));
#11925=CARTESIAN_POINT('Ctrl Pts',(3.71718250921266,1.16429409650172,-5.96160772785424));
#11926=CARTESIAN_POINT('Ctrl Pts',(3.72416840961237,1.16320662749307,-5.96207856110625));
#11927=CARTESIAN_POINT('Ctrl Pts',(3.73654993867548,1.16116489387022,-5.96291776644867));
#11928=CARTESIAN_POINT('Ctrl Pts',(3.74194954116544,1.16023574172269,-5.96328534405909));
#11929=CARTESIAN_POINT('Ctrl Pts',(3.75320257220275,1.15821839929621,-5.96405482568101));
#11930=CARTESIAN_POINT('Ctrl Pts',(3.7590546122738,1.15712343455128,-5.96445693266082));
#11931=CARTESIAN_POINT('Ctrl Pts',(3.7743187940757,1.15414742027536,-5.96551098365056));
#11932=CARTESIAN_POINT('Ctrl Pts',(3.78371652530272,1.15219563059152,-5.96616513241124));
#11933=CARTESIAN_POINT('Ctrl Pts',(3.82675803935259,1.14270622793917,-5.96918579055234));
#11934=CARTESIAN_POINT('Ctrl Pts',(3.86008146848052,1.13380910050893,-5.97159463617168));
#11935=CARTESIAN_POINT('Ctrl Pts',(3.95727721363896,1.10323104992977,-5.97883453960332));
#11936=CARTESIAN_POINT('Ctrl Pts',(4.01972795658668,1.07751481677913,-5.98377480776373));
#11937=CARTESIAN_POINT('Ctrl Pts',(4.08678927887574,1.04290713118811,-5.98931248482588));
#11938=CARTESIAN_POINT('Ctrl Pts',(4.09391153456015,1.03913856710895,-5.98990356147036));
#11939=CARTESIAN_POINT('Ctrl Pts',(4.15011244382659,1.00865897608824,-5.99458904261567));
#11940=CARTESIAN_POINT('Ctrl Pts',(4.19727845647524,0.978555705884622,-5.99865502741021));
#11941=CARTESIAN_POINT('Ctrl Pts',(4.24729721532134,0.941374811239059,-6.00299203176129));
#11942=CARTESIAN_POINT('Ctrl Pts',(4.25242991902042,0.937493767429404,-6.00343734647252));
#11943=CARTESIAN_POINT('Ctrl Pts',(4.26065100879718,0.931170906272169,-6.0041507128686));
#11944=CARTESIAN_POINT('Ctrl Pts',(4.26375932641686,0.928755393972669,-6.00442045392978));
#11945=CARTESIAN_POINT('Ctrl Pts',(4.26925331145728,0.924441596151063,-6.00489718061023));
#11946=CARTESIAN_POINT('Ctrl Pts',(4.27164378230166,0.922549583568344,-6.00510458813698));
#11947=CARTESIAN_POINT('Ctrl Pts',(4.27682093511297,0.918419168113932,-6.00555372542975));
#11948=CARTESIAN_POINT('Ctrl Pts',(4.27960478858504,0.916177351033183,-6.00579521108816));
#11949=CARTESIAN_POINT('Ctrl Pts',(4.28745901458286,0.90979323942721,-6.00647659886485));
#11950=CARTESIAN_POINT('Ctrl Pts',(4.2925052098444,0.905621210585541,-6.00691446374079));
#11951=CARTESIAN_POINT('Ctrl Pts',(4.32616402126353,0.877317361924188,-6.00983770837115));
#11952=CARTESIAN_POINT('Ctrl Pts',(4.35365017138381,0.851872764363065,-6.01223797092243));
#11953=CARTESIAN_POINT('Ctrl Pts',(4.41676399519084,0.787596195246808,-6.01791612874001));
#11954=CARTESIAN_POINT('Ctrl Pts',(4.4510890804904,0.747600828657859,-6.02114961614977));
#11955=CARTESIAN_POINT('Ctrl Pts',(4.52638143105319,0.646942469589884,-6.02893706756474));
#11956=CARTESIAN_POINT('Ctrl Pts',(4.56459512533909,0.584507375386231,-6.03350763673975));
#11957=CARTESIAN_POINT('Ctrl Pts',(4.60138332518485,0.509557236070088,-6.03898648710132));
#11958=CARTESIAN_POINT('Ctrl Pts',(4.60586361685565,0.500113556196835,-6.03967640651002));
#11959=CARTESIAN_POINT('Ctrl Pts',(4.61302673722192,0.484480946207145,-6.04081846159462));
#11960=CARTESIAN_POINT('Ctrl Pts',(4.61578320737482,0.478326250733105,-6.04126809613255));
#11961=CARTESIAN_POINT('Ctrl Pts',(4.62066294234223,0.467174933498236,-6.04208292425452));
#11962=CARTESIAN_POINT('Ctrl Pts',(4.62280481904,0.462186623940911,-6.0424474786049));
#11963=CARTESIAN_POINT('Ctrl Pts',(4.62732173268691,0.451463087436911,-6.04323138738794));
#11964=CARTESIAN_POINT('Ctrl Pts',(4.62968605796868,0.445723555549147,-6.04365108733417));
#11965=CARTESIAN_POINT('Ctrl Pts',(4.63602608564814,0.429980532021151,-6.04480278948988));
#11966=CARTESIAN_POINT('Ctrl Pts',(4.63991010525876,0.419941006948005,-6.04553780054602));
#11967=CARTESIAN_POINT('Ctrl Pts',(4.66172987062527,0.361158501535252,-6.04984582608918));
#11968=CARTESIAN_POINT('Ctrl Pts',(4.67656069430446,0.311331854197686,-6.05351902030705));
#11969=CARTESIAN_POINT('Ctrl Pts',(4.70440071669947,0.188678151739639,-6.06259990435234));
#11970=CARTESIAN_POINT('Ctrl Pts',(4.71393687725998,0.11528430726658,-6.06807243452782));
#11971=CARTESIAN_POINT('Ctrl Pts',(4.71710910509289,0.0252881591905452,
-6.07461937195196));
#11972=CARTESIAN_POINT('Ctrl Pts',(4.71734563529417,0.00907752200102984,
-6.07579156722361));
#11973=CARTESIAN_POINT('Ctrl Pts',(4.71710481213331,-0.0306826391398403,
-6.07864231504494));
#11974=CARTESIAN_POINT('Ctrl Pts',(4.71625587545994,-0.0542243082636352,
-6.08030933238487));
#11975=CARTESIAN_POINT('Ctrl Pts',(4.71430359219265,-0.0837417753592146,
-6.08236105018067));
#11976=CARTESIAN_POINT('Ctrl Pts',(4.71385955155349,-0.0897540851022286,
-6.08277694316532));
#11977=CARTESIAN_POINT('Ctrl Pts',(4.71308787211326,-0.0992132425788758,
-6.08342782248112));
#11978=CARTESIAN_POINT('Ctrl Pts',(4.71279117487023,-0.102662405591984,
-6.08366443550864));
#11979=CARTESIAN_POINT('Ctrl Pts',(4.7122027868054,-0.109166543400187,-6.08410919525693));
#11980=CARTESIAN_POINT('Ctrl Pts',(4.71191436689844,-0.112221664211276,
-6.08431750593605));
#11981=CARTESIAN_POINT('Ctrl Pts',(4.71121086989207,-0.119374647054153,
-6.08480386463247));
#11982=CARTESIAN_POINT('Ctrl Pts',(4.7107862340634,-0.123471502678084,-6.08508138397478));
#11983=CARTESIAN_POINT('Ctrl Pts',(4.70932980611231,-0.136838817368064,
-6.08598372569516));
#11984=CARTESIAN_POINT('Ctrl Pts',(4.70820934469925,-0.146099539736795,
-6.08660389932088));
#11985=CARTESIAN_POINT('Ctrl Pts',(4.70142462970588,-0.197088081499661,
-6.08999597737722));
#11986=CARTESIAN_POINT('Ctrl Pts',(4.6936349970882,-0.238506708506432,-6.09266850379989));
#11987=CARTESIAN_POINT('Ctrl Pts',(4.68106826005522,-0.289962352409489,
-6.09598177255176));
#11988=CARTESIAN_POINT('Ctrl Pts',(4.67834877505836,-0.300465685335471,
-6.09665768602606));
#11989=CARTESIAN_POINT('Ctrl Pts',(4.65041839586667,-0.402507750322544,
-6.10323249202609));
#11990=CARTESIAN_POINT('Ctrl Pts',(4.61437356907952,-0.490709926578817,
-6.10901415270714));
#11991=CARTESIAN_POINT('Ctrl Pts',(4.55920521722374,-0.589636496441019,
-6.1163580264285));
#11992=CARTESIAN_POINT('Ctrl Pts',(4.54990507022347,-0.605434644556412,
-6.1175580596317));
#11993=CARTESIAN_POINT('Ctrl Pts',(4.53650506174603,-0.627028022809492,
-6.11923999862852));
#11994=CARTESIAN_POINT('Ctrl Pts',(4.53271552115075,-0.633013439868542,
-6.11971076099428));
#11995=CARTESIAN_POINT('Ctrl Pts',(4.52608253361021,-0.643283761225334,
-6.12052663031118));
#11996=CARTESIAN_POINT('Ctrl Pts',(4.5232645648998,-0.647584948203317,-6.12087079920097));
#11997=CARTESIAN_POINT('Ctrl Pts',(4.51736269007792,-0.656465811604456,
-6.1215866744195));
#11998=CARTESIAN_POINT('Ctrl Pts',(4.51427457170972,-0.661042523108681,
-6.12195853088882));
#11999=CARTESIAN_POINT('Ctrl Pts',(4.50693567913406,-0.671755799496713,
-6.12283601105967));
#12000=CARTESIAN_POINT('Ctrl Pts',(4.50265855611122,-0.677873937988855,
-6.12334261337593));
#12001=CARTESIAN_POINT('Ctrl Pts',(4.48830816062349,-0.697991208772863,
-6.12502696731538));
#12002=CARTESIAN_POINT('Ctrl Pts',(4.47798597202029,-0.711809163839903,
-6.12621409714304));
#12003=CARTESIAN_POINT('Ctrl Pts',(4.45259460187782,-0.744287017379406,
-6.12907918687214));
#12004=CARTESIAN_POINT('Ctrl Pts',(4.43725202505627,-0.762722424332887,
-6.13076716461647));
#12005=CARTESIAN_POINT('Ctrl Pts',(4.3786865913866,-0.828877042952145,-6.13705658888953));
#12006=CARTESIAN_POINT('Ctrl Pts',(4.33213858664354,-0.873494133910334,
-6.14177251505145));
#12007=CARTESIAN_POINT('Ctrl Pts',(4.23542319709147,-0.952072742278277,
-6.15091740595427));
#12008=CARTESIAN_POINT('Ctrl Pts',(4.1858107260038,-0.986424659151665,-6.15533038276007));
#12009=CARTESIAN_POINT('Ctrl Pts',(4.12512835546305,-1.02188907604602,-6.16025918078904));
#12010=CARTESIAN_POINT('Ctrl Pts',(4.1164094273622,-1.02683642879581,-6.16095662195275));
#12011=CARTESIAN_POINT('Ctrl Pts',(4.10417747106957,-1.03357217812863,-6.1619191413475));
#12012=CARTESIAN_POINT('Ctrl Pts',(4.10071732519429,-1.03545500960532,-6.16218966244169));
#12013=CARTESIAN_POINT('Ctrl Pts',(4.09473149177945,-1.03867336986333,-6.16265454515327));
#12014=CARTESIAN_POINT('Ctrl Pts',(4.09221029877305,-1.04001711944647,-6.16284940762528));
#12015=CARTESIAN_POINT('Ctrl Pts',(4.08688048340478,-1.04283295842484,-6.16325932263553));
#12016=CARTESIAN_POINT('Ctrl Pts',(4.0840707599462,-1.04430290317715,-6.1634742349395));
#12017=CARTESIAN_POINT('Ctrl Pts',(4.08022727770696,-1.04629394310005,-6.16376665336777));
#12018=CARTESIAN_POINT('Ctrl Pts',(4.07919866498243,-1.04682487363855,-6.1638447594958));
#12019=CARTESIAN_POINT('Ctrl Pts',(4.07816926754759,-1.04735428871591,-6.16392277459278));
#12020=CARTESIAN_POINT('Origin',(3.53951905042299,8.32667268468867E-16,
0.924367114736157));
#12021=CARTESIAN_POINT('',(4.0781692678987,-1.04735428853534,-6.76206729648848));
#12022=CARTESIAN_POINT('',(4.07816925191529,-1.04735429675555,-6.66223230003384));
#12023=CARTESIAN_POINT('',(4.07816926754759,-1.04735428871592,0.924367114736157));
#12024=CARTESIAN_POINT('Ctrl Pts',(4.0781692678987,-1.04735428853534,-6.76206729648848));
#12025=CARTESIAN_POINT('Ctrl Pts',(4.12294586906839,-1.02432585754318,-6.75891221404368));
#12026=CARTESIAN_POINT('Ctrl Pts',(4.16619577612126,-0.998451771647165,
-6.75570421536983));
#12027=CARTESIAN_POINT('Ctrl Pts',(4.21650939873315,-0.963791849091696,
-6.75168804733695));
#12028=CARTESIAN_POINT('Ctrl Pts',(4.22527931040189,-0.95757167534045,-6.75097700677152));
#12029=CARTESIAN_POINT('Ctrl Pts',(4.23897441162349,-0.947573620149851,
-6.74984844905781));
#12030=CARTESIAN_POINT('Ctrl Pts',(4.2439571426804,-0.94387527756948,-6.74943396220505));
#12031=CARTESIAN_POINT('Ctrl Pts',(4.25324476262864,-0.936867202031728,
-6.74865392619116));
#12032=CARTESIAN_POINT('Ctrl Pts',(4.25755645574725,-0.933566724648117,
-6.74828874172827));
#12033=CARTESIAN_POINT('Ctrl Pts',(4.2671759881112,-0.926097185242173,-6.74746701256643));
#12034=CARTESIAN_POINT('Ctrl Pts',(4.27247108641371,-0.921912102717862,
-6.74700984792915));
#12035=CARTESIAN_POINT('Ctrl Pts',(4.28588694809413,-0.911119981172702,
-6.74583895582923));
#12036=CARTESIAN_POINT('Ctrl Pts',(4.29395597890684,-0.9044498700557,-6.74512274566076));
#12037=CARTESIAN_POINT('Ctrl Pts',(4.35758061023219,-0.850411922128031,
-6.73937745305371));
#12038=CARTESIAN_POINT('Ctrl Pts',(4.40870126635017,-0.798087647356966,
-6.73414201789298));
#12039=CARTESIAN_POINT('Ctrl Pts',(4.48776191431729,-0.700498792080305,
-6.72496198139348));
#12040=CARTESIAN_POINT('Ctrl Pts',(4.51810399235955,-0.657445553258234,
-6.72107918119728));
#12041=CARTESIAN_POINT('Ctrl Pts',(4.56495733416495,-0.580496367214681,
-6.71453537548096));
#12042=CARTESIAN_POINT('Ctrl Pts',(4.58291176170722,-0.547569142183366,
-6.71184874296286));
#12043=CARTESIAN_POINT('Ctrl Pts',(4.60212436928633,-0.507944779302869,
-6.7087895550371));
#12044=CARTESIAN_POINT('Ctrl Pts',(4.60493284229168,-0.502027309524509,
-6.7083371273702));
#12045=CARTESIAN_POINT('Ctrl Pts',(4.60919777314104,-0.49284406669514,-6.7076421719171));
#12046=CARTESIAN_POINT('Ctrl Pts',(4.61068891838061,-0.489594688234796,
-6.70739764512554));
#12047=CARTESIAN_POINT('Ctrl Pts',(4.61342435445102,-0.483561534248623,
-6.70694623921899));
#12048=CARTESIAN_POINT('Ctrl Pts',(4.61467262886655,-0.480779723499948,
-6.70673913169493));
#12049=CARTESIAN_POINT('Ctrl Pts',(4.6175078359082,-0.474395128736488,-6.706266119389));
#12050=CARTESIAN_POINT('Ctrl Pts',(4.61908752028132,-0.470789209529827,
-6.70600064993203));
#12051=CARTESIAN_POINT('Ctrl Pts',(4.6232013752411,-0.461268989556435,-6.70530401006573));
#12052=CARTESIAN_POINT('Ctrl Pts',(4.62570525320708,-0.455341629173548,
-6.70487456987477));
#12053=CARTESIAN_POINT('Ctrl Pts',(4.64869035976942,-0.399660988058057,
-6.70087782824475));
#12054=CARTESIAN_POINT('Ctrl Pts',(4.66579104353472,-0.348572615305978,
-6.69748732430674));
#12055=CARTESIAN_POINT('Ctrl Pts',(4.68187099567671,-0.286754659145394,
-6.6935126710381));
#12056=CARTESIAN_POINT('Ctrl Pts',(4.68427794973705,-0.276989651486037,
-6.6928885682358));
#12057=CARTESIAN_POINT('Ctrl Pts',(4.70186607582313,-0.201485628112676,
-6.68808434664853));
#12058=CARTESIAN_POINT('Ctrl Pts',(4.71149729214537,-0.13458632785788,-6.68394369326068));
#12059=CARTESIAN_POINT('Ctrl Pts',(4.71665378599857,-0.04440392623186,-6.67820207065805));
#12060=CARTESIAN_POINT('Ctrl Pts',(4.71729392926832,-0.0215436977117833,
-6.67673391753122));
#12061=CARTESIAN_POINT('Ctrl Pts',(4.71724967130154,0.017955038036478,-6.67416473365664));
#12062=CARTESIAN_POINT('Ctrl Pts',(4.71687858043912,0.0345874428860701,
-6.67307297279306));
#12063=CARTESIAN_POINT('Ctrl Pts',(4.71583536023531,0.0585591735798976,
-6.67148258549858));
#12064=CARTESIAN_POINT('Ctrl Pts',(4.7154464293154,0.0659092786016217,-6.67099266275923));
#12065=CARTESIAN_POINT('Ctrl Pts',(4.71464623374949,0.0787494128198078,
-6.67013258806341));
#12066=CARTESIAN_POINT('Ctrl Pts',(4.7142653177287,0.0842411580578814,-6.66976338404987));
#12067=CARTESIAN_POINT('Ctrl Pts',(4.71345193211751,0.0948862163823833,
-6.66904502432509));
#12068=CARTESIAN_POINT('Ctrl Pts',(4.71302399302121,0.100039757154611,-6.66869601721195));
#12069=CARTESIAN_POINT('Ctrl Pts',(4.71179161219089,0.113782817097294,-6.66776193904133));
#12070=CARTESIAN_POINT('Ctrl Pts',(4.71092672101904,0.122366461682962,-6.66717500962747));
#12071=CARTESIAN_POINT('Ctrl Pts',(4.70738854419239,0.153993661534007,-6.66499895785164));
#12072=CARTESIAN_POINT('Ctrl Pts',(4.7041290633129,0.176964937351188,-6.66339191204045));
#12073=CARTESIAN_POINT('Ctrl Pts',(4.6830111624516,0.299628145184901,-6.65466181449661));
#12074=CARTESIAN_POINT('Ctrl Pts',(4.65302867038665,0.396788144129833,-6.64716430093981));
#12075=CARTESIAN_POINT('Ctrl Pts',(4.59855957454331,0.516165541995005,-6.63759317243328));
#12076=CARTESIAN_POINT('Ctrl Pts',(4.58507819413828,0.542954894142923,-6.63542399616074));
#12077=CARTESIAN_POINT('Ctrl Pts',(4.56236899977718,0.5840909832043,-6.6320874458712));
#12078=CARTESIAN_POINT('Ctrl Pts',(4.55382757857985,0.598800951631323,-6.63089319504041));
#12079=CARTESIAN_POINT('Ctrl Pts',(4.54226982419969,0.617748195805423,-6.62935832582027));
#12080=CARTESIAN_POINT('Ctrl Pts',(4.53954038234611,0.622156962455123,-6.62900142903356));
#12081=CARTESIAN_POINT('Ctrl Pts',(4.53503904824843,0.629321641736402,-6.6284220202326));
#12082=CARTESIAN_POINT('Ctrl Pts',(4.53328465282591,0.632088382250458,-6.62819841683938));
#12083=CARTESIAN_POINT('Ctrl Pts',(4.52984123477872,0.637468993913774,-6.62776389981318));
#12084=CARTESIAN_POINT('Ctrl Pts',(4.52815336676141,0.640083538228561,-6.62755291922081));
#12085=CARTESIAN_POINT('Ctrl Pts',(4.52396766556247,0.646511225999585,-6.62703455435523));
#12086=CARTESIAN_POINT('Ctrl Pts',(4.52145798528301,0.650316669868127,-6.6267279379496));
#12087=CARTESIAN_POINT('Ctrl Pts',(4.51411031837267,0.661318466055091,-6.62584199477558));
#12088=CARTESIAN_POINT('Ctrl Pts',(4.50921475402004,0.668476256990736,-6.62526623099818));
#12089=CARTESIAN_POINT('Ctrl Pts',(4.45923985469752,0.73983994907711,-6.61952512930229));
#12090=CARTESIAN_POINT('Ctrl Pts',(4.40792444146934,0.799453061407792,-6.61471497310608));
#12091=CARTESIAN_POINT('Ctrl Pts',(4.31189842067517,0.890754946157779,-6.60651656530318));
#12092=CARTESIAN_POINT('Ctrl Pts',(4.2702293474513,0.925243808395323,-6.60316360161088));
#12093=CARTESIAN_POINT('Ctrl Pts',(4.2099434283504,0.968521427195858,-6.59842486884806));
#12094=CARTESIAN_POINT('Ctrl Pts',(4.19324476206694,0.979870004192287,-6.59712358152529));
#12095=CARTESIAN_POINT('Ctrl Pts',(4.16354265234985,0.998958586717111,-6.59482135233132));
#12096=CARTESIAN_POINT('Ctrl Pts',(4.15066614736092,1.00688773247659,-6.59382721394972));
#12097=CARTESIAN_POINT('Ctrl Pts',(4.13153525485413,1.01816605391762,-6.59235397927314));
#12098=CARTESIAN_POINT('Ctrl Pts',(4.12539723719483,1.02171035340222,-6.59188186529944));
#12099=CARTESIAN_POINT('Ctrl Pts',(4.11447001498192,1.02788925676774,-6.59104218174043));
#12100=CARTESIAN_POINT('Ctrl Pts',(4.1096937173476,1.03054635184734,-6.59067542247206));
#12101=CARTESIAN_POINT('Ctrl Pts',(4.09963200215845,1.03605240924621,-6.5899032766969));
#12102=CARTESIAN_POINT('Ctrl Pts',(4.09434296012218,1.03889438362657,-6.5894976577528));
#12103=CARTESIAN_POINT('Ctrl Pts',(4.08034016452336,1.04628111296678,-6.58842434770627));
#12104=CARTESIAN_POINT('Ctrl Pts',(4.07159101124071,1.0507573759761,-6.58775430185985));
#12105=CARTESIAN_POINT('Ctrl Pts',(4.03310034540623,1.06984607512761,-6.58480828238663));
#12106=CARTESIAN_POINT('Ctrl Pts',(4.00280828435494,1.08330781952285,-6.58249369995613));
#12107=CARTESIAN_POINT('Ctrl Pts',(3.87750347885602,1.13277580274728,-6.57292938312651));
#12108=CARTESIAN_POINT('Ctrl Pts',(3.77859010214468,1.15769365587022,-6.56535491917215));
#12109=CARTESIAN_POINT('Ctrl Pts',(3.65628269370855,1.17214665872541,-6.55644810478756));
#12110=CARTESIAN_POINT('Ctrl Pts',(3.6347668743395,1.174090926378,-6.55490026791335));
#12111=CARTESIAN_POINT('Ctrl Pts',(3.59968418005628,1.17629029007599,-6.55241888923025));
#12112=CARTESIAN_POINT('Ctrl Pts',(3.58614546742989,1.17690471403828,-6.55147156906534));
#12113=CARTESIAN_POINT('Ctrl Pts',(3.56783069258954,1.17741932335509,-6.55020651238288));
#12114=CARTESIAN_POINT('Ctrl Pts',(3.56306204764912,1.17752432728116,-6.54987863483975));
#12115=CARTESIAN_POINT('Ctrl Pts',(3.55510717961657,1.17765114675324,-6.54933433922799));
#12116=CARTESIAN_POINT('Ctrl Pts',(3.55192131552593,1.1776890072353,-6.54911706366381));
#12117=CARTESIAN_POINT('Ctrl Pts',(3.5458902695692,1.17773620333583,-6.5487071410676));
#12118=CARTESIAN_POINT('Ctrl Pts',(3.54304514911707,1.17774815820159,-6.54851434771193));
#12119=CARTESIAN_POINT('Ctrl Pts',(3.53630889816459,1.17775205281308,-6.54805920848759));
#12120=CARTESIAN_POINT('Ctrl Pts',(3.5324177656834,1.17773501935053,-6.54779735067951));
#12121=CARTESIAN_POINT('Ctrl Pts',(3.51879198047609,1.17760783985833,-6.54688383948954));
#12122=CARTESIAN_POINT('Ctrl Pts',(3.50905835341731,1.17739627861934,-6.54623743631779));
#12123=CARTESIAN_POINT('Ctrl Pts',(3.42752961053978,1.17461247194562,-6.5408664805545));
#12124=CARTESIAN_POINT('Ctrl Pts',(3.35609549585743,1.16559632415304,-6.53643623612184));
#12125=CARTESIAN_POINT('Ctrl Pts',(3.22889658181621,1.1375493782972,-6.52837940305496));
#12126=CARTESIAN_POINT('Ctrl Pts',(3.17289044410174,1.12075319097083,-6.52476924843539));
#12127=CARTESIAN_POINT('Ctrl Pts',(3.09863830059703,1.09232107716451,-6.51970054991633));
#12128=CARTESIAN_POINT('Ctrl Pts',(3.0791213085877,1.08423936982468,-6.51834097168394));
#12129=CARTESIAN_POINT('Ctrl Pts',(3.04553384954998,1.06926087191269,-6.51594509405415));
#12130=CARTESIAN_POINT('Ctrl Pts',(3.03136387318905,1.06259986321686,-6.51491641233245));
#12131=CARTESIAN_POINT('Ctrl Pts',(3.01089022307675,1.05247245375225,-6.51340162254873));
#12132=CARTESIAN_POINT('Ctrl Pts',(3.00447845843092,1.04922746061217,-6.51292308451294));
#12133=CARTESIAN_POINT('Ctrl Pts',(2.99323121308099,1.04340532883207,-6.51207610616659));
#12134=CARTESIAN_POINT('Ctrl Pts',(2.98838322470096,1.0408527183706,-6.51170852554223));
#12135=CARTESIAN_POINT('Ctrl Pts',(2.97830145303762,1.03545418118627,-6.5109387818606));
#12136=CARTESIAN_POINT('Ctrl Pts',(2.97307111160399,1.03260219025089,-6.51053641406549));
#12137=CARTESIAN_POINT('Ctrl Pts',(2.95945825676147,1.02504484930612,-6.50948110177823));
#12138=CARTESIAN_POINT('Ctrl Pts',(2.95111146141057,1.02027641701927,-6.50882594338475));
#12139=CARTESIAN_POINT('Ctrl Pts',(2.91593388254755,0.999604615612054,-6.50602953355273));
#12140=CARTESIAN_POINT('Ctrl Pts',(2.88968428059032,0.98274223900862,-6.50385433175206));
#12141=CARTESIAN_POINT('Ctrl Pts',(2.79606961505231,0.917213840555172,-6.49575955666949));
#12142=CARTESIAN_POINT('Ctrl Pts',(2.73324224909032,0.862503727090912,-6.48963448534913));
#12143=CARTESIAN_POINT('Ctrl Pts',(2.64139842627212,0.763652168008503,-6.47975812700154));
#12144=CARTESIAN_POINT('Ctrl Pts',(2.60863848026168,0.723358789502896,-6.47599596749412));
#12145=CARTESIAN_POINT('Ctrl Pts',(2.57461891572294,0.675359998176562,-6.47190411238623));
#12146=CARTESIAN_POINT('Ctrl Pts',(2.57064893501322,0.669652224952945,-6.47142344757296));
#12147=CARTESIAN_POINT('Ctrl Pts',(2.56466630086488,0.660886205418549,-6.47069462164926));
#12148=CARTESIAN_POINT('Ctrl Pts',(2.56261705816145,0.657853295396841,-6.47044415185961));
#12149=CARTESIAN_POINT('Ctrl Pts',(2.55889062886374,0.65228231258221,-6.46998723979864));
#12150=CARTESIAN_POINT('Ctrl Pts',(2.55720912945023,0.649747286320787,-6.46978052222146));
#12151=CARTESIAN_POINT('Ctrl Pts',(2.55343426346913,0.644008154308815,-6.46931520251178));
#12152=CARTESIAN_POINT('Ctrl Pts',(2.55134668006022,0.640800341263827,-6.46905697927665));
#12153=CARTESIAN_POINT('Ctrl Pts',(2.54598982966767,0.632480489507565,-6.46839188563711));
#12154=CARTESIAN_POINT('Ctrl Pts',(2.54274431714432,0.627353183642247,-6.4679865022697));
#12155=CARTESIAN_POINT('Ctrl Pts',(2.52116884812424,0.592677808128442,-6.46527342525284));
#12156=CARTESIAN_POINT('Ctrl Pts',(2.50411366397944,0.562352482531343,-6.46303882045231));
#12157=CARTESIAN_POINT('Ctrl Pts',(2.47566575099091,0.506074137307548,-6.45905477299111));
#12158=CARTESIAN_POINT('Ctrl Pts',(2.46382022129255,0.480382165825438,-6.45729403121127));
#12159=CARTESIAN_POINT('Ctrl Pts',(2.41817938197563,0.371214106629763,-6.44995815463985));
#12160=CARTESIAN_POINT('Ctrl Pts',(2.39309226439797,0.284440647682221,-6.44444801447752));
#12161=CARTESIAN_POINT('Ctrl Pts',(2.37516021319155,0.178000693229838,-6.43744105101478));
#12162=CARTESIAN_POINT('Ctrl Pts',(2.372588483264,0.160277087697721,-6.43626744441922));
#12163=CARTESIAN_POINT('Ctrl Pts',(2.36950518607273,0.134981569568881,-6.43457949758076));
#12164=CARTESIAN_POINT('Ctrl Pts',(2.36866106878908,0.127452145011255,-6.43407544940521));
#12165=CARTESIAN_POINT('Ctrl Pts',(2.36732553725242,0.114403362164892,-6.43319888259013));
#12166=CARTESIAN_POINT('Ctrl Pts',(2.36680031194586,0.108887649588134,-6.43282742309709));
#12167=CARTESIAN_POINT('Ctrl Pts',(2.36586500703955,0.0982721889372516,
-6.43211063109108));
#12168=CARTESIAN_POINT('Ctrl Pts',(2.36544919904447,0.0931730611882645,
-6.43176548495266));
#12169=CARTESIAN_POINT('Ctrl Pts',(2.36444368903899,0.0797643618219554,
-6.43085560770614));
#12170=CARTESIAN_POINT('Ctrl Pts',(2.36390891320464,0.0714510842384667,
-6.43028919239542));
#12171=CARTESIAN_POINT('Ctrl Pts',(2.36232279813214,0.0419045591124454,
-6.42826751666083));
#12172=CARTESIAN_POINT('Ctrl Pts',(2.36175826511778,0.0206504180033991,
-6.42679745648869));
#12173=CARTESIAN_POINT('Ctrl Pts',(2.36178601530212,-0.0332627310663779,
-6.42302618903627));
#12174=CARTESIAN_POINT('Ctrl Pts',(2.36316104713104,-0.0659017181671396,
-6.42070333263085));
#12175=CARTESIAN_POINT('Ctrl Pts',(2.3701139953061,-0.148797490192785,-6.4147096206495));
#12176=CARTESIAN_POINT('Ctrl Pts',(2.37757443760778,-0.198829105981824,
-6.41100142558572));
#12177=CARTESIAN_POINT('Ctrl Pts',(2.38892298615492,-0.251465217744737,
-6.40705015076198));
#12178=CARTESIAN_POINT('Ctrl Pts',(2.38963557288157,-0.254703841678869,
-6.40680684376538));
#12179=CARTESIAN_POINT('Ctrl Pts',(2.39499021098422,-0.278559525092273,
-6.40501337354838));
#12180=CARTESIAN_POINT('Ctrl Pts',(2.40017285158668,-0.299051748802747,
-6.4034656674151));
#12181=CARTESIAN_POINT('Ctrl Pts',(2.41672368711429,-0.357795136622129,
-6.39902385038681));
#12182=CARTESIAN_POINT('Ctrl Pts',(2.42948874950418,-0.395626364350084,
-6.396156346492));
#12183=CARTESIAN_POINT('Ctrl Pts',(2.4464476069998,-0.438553242663619,-6.39294635308094));
#12184=CARTESIAN_POINT('Ctrl Pts',(2.4487904026558,-0.444348003529411,-6.39251399610978));
#12185=CARTESIAN_POINT('Ctrl Pts',(2.45266290994123,-0.453711209549035,
-6.39181727046263));
#12186=CARTESIAN_POINT('Ctrl Pts',(2.45416429175512,-0.457291133409122,
-6.39155133334197));
#12187=CARTESIAN_POINT('Ctrl Pts',(2.45687489219262,-0.463665785809996,
-6.39107867316813));
#12188=CARTESIAN_POINT('Ctrl Pts',(2.45807727400085,-0.46646330958374,-6.39087155685421));
#12189=CARTESIAN_POINT('Ctrl Pts',(2.46073116170004,-0.47257256271065,-6.39041994338628));
#12190=CARTESIAN_POINT('Ctrl Pts',(2.46218707494057,-0.475882287298432,
-6.39017571299449));
#12191=CARTESIAN_POINT('Ctrl Pts',(2.46640075707148,-0.485342793312489,
-6.3894787041054));
#12192=CARTESIAN_POINT('Ctrl Pts',(2.46919617326328,-0.491476797464264,
-6.38902811287098));
#12193=CARTESIAN_POINT('Ctrl Pts',(2.490228286078,-0.536597084265478,-6.38572111742289));
#12194=CARTESIAN_POINT('Ctrl Pts',(2.51053946217682,-0.574586324232129,
-6.38297757773909));
#12195=CARTESIAN_POINT('Ctrl Pts',(2.58258778816675,-0.693212795286867,
-6.37427492586448));
#12196=CARTESIAN_POINT('Ctrl Pts',(2.64207827258558,-0.768675366373853,
-6.36849427554628));
#12197=CARTESIAN_POINT('Ctrl Pts',(2.73018760142353,-0.856085553219501,
-6.36055546273));
#12198=CARTESIAN_POINT('Ctrl Pts',(2.75104123065136,-0.875329876603424,
-6.35871623235301));
#12199=CARTESIAN_POINT('Ctrl Pts',(2.77962509665173,-0.899857051898429,
-6.35623245344694));
#12200=CARTESIAN_POINT('Ctrl Pts',(2.78675349941669,-0.90582865481419,-6.3556159866354));
#12201=CARTESIAN_POINT('Ctrl Pts',(2.79851063216422,-0.915443209235069,
-6.3546035600282));
#12202=CARTESIAN_POINT('Ctrl Pts',(2.8030973890916,-0.919137029965733,-6.3542096417199));
#12203=CARTESIAN_POINT('Ctrl Pts',(2.81202325033869,-0.926215528558153,
-6.35344498986497));
#12204=CARTESIAN_POINT('Ctrl Pts',(2.81635876113683,-0.92960450661454,-6.35307443936028));
#12205=CARTESIAN_POINT('Ctrl Pts',(2.82653800918138,-0.937447107856184,
-6.3522063321698));
#12206=CARTESIAN_POINT('Ctrl Pts',(2.83239993454968,-0.941876635727669,
-6.35170785711019));
#12207=CARTESIAN_POINT('Ctrl Pts',(2.85160822394215,-0.956110877327952,
-6.35007885200092));
#12208=CARTESIAN_POINT('Ctrl Pts',(2.86511950189476,-0.965688622475829,
-6.34893977284582));
#12209=CARTESIAN_POINT('Ctrl Pts',(2.89764471465889,-0.987729253563438,
-6.34621215992179));
#12210=CARTESIAN_POINT('Ctrl Pts',(2.91682583919942,-0.99993239202549,-6.3446148452297));
#12211=CARTESIAN_POINT('Ctrl Pts',(2.99365118278365,-1.04574118241993,-6.33826062215976));
#12212=CARTESIAN_POINT('Ctrl Pts',(3.05374952649696,-1.07497558071424,-6.33337420040919));
#12213=CARTESIAN_POINT('Ctrl Pts',(3.17211340255953,-1.12059163457256,-6.32406524200008));
#12214=CARTESIAN_POINT('Ctrl Pts',(3.22981535992225,-1.13789173094266,-6.31966017815492));
#12215=CARTESIAN_POINT('Ctrl Pts',(3.29839122572907,-1.1528456256141,-6.31473820249754));
#12216=CARTESIAN_POINT('Ctrl Pts',(3.30821829082806,-1.15485741093623,-6.31404032895314));
#12217=CARTESIAN_POINT('Ctrl Pts',(3.32194048650467,-1.15748440969224,-6.31307728914153));
#12218=CARTESIAN_POINT('Ctrl Pts',(3.32581448173988,-1.15820591804602,-6.31280667312941));
#12219=CARTESIAN_POINT('Ctrl Pts',(3.33250390215438,-1.15941707608936,-6.31234165198646));
#12220=CARTESIAN_POINT('Ctrl Pts',(3.33531759190815,-1.1599159420946,-6.31214674552923));
#12221=CARTESIAN_POINT('Ctrl Pts',(3.34125767146775,-1.16094683128152,-6.31173676536307));
#12222=CARTESIAN_POINT('Ctrl Pts',(3.34438444515803,-1.16147647660685,-6.31152183178914));
#12223=CARTESIAN_POINT('Ctrl Pts',(3.35214903886939,-1.16275948397644,-6.31099017890119));
#12224=CARTESIAN_POINT('Ctrl Pts',(3.35678936272616,-1.16349774469293,-6.310674290318));
#12225=CARTESIAN_POINT('Ctrl Pts',(3.37431124288925,-1.16617800709058,-6.30948800825593));
#12226=CARTESIAN_POINT('Ctrl Pts',(3.38722086290756,-1.16793409941775,-6.3086272489041));
#12227=CARTESIAN_POINT('Ctrl Pts',(3.42045728511714,-1.1718947423068,-6.30643902679408));
#12228=CARTESIAN_POINT('Ctrl Pts',(3.44081773059848,-1.17378496306027,-6.30512514279939));
#12229=CARTESIAN_POINT('Ctrl Pts',(3.51895574897153,-1.17899136380083,-6.30014974112011));
#12230=CARTESIAN_POINT('Ctrl Pts',(3.57690171028414,-1.17857830810527,-6.29659662283391));
#12231=CARTESIAN_POINT('Ctrl Pts',(3.70982666257039,-1.16781366500642,-6.28833912627584));
#12232=CARTESIAN_POINT('Ctrl Pts',(3.78429717843459,-1.15450201305926,-6.28362472168193));
#12233=CARTESIAN_POINT('Ctrl Pts',(3.86698072823359,-1.13135840197258,-6.27798958768884));
#12234=CARTESIAN_POINT('Ctrl Pts',(3.87694700090374,-1.12842605038632,-6.2773038095413));
#12235=CARTESIAN_POINT('Ctrl Pts',(3.89329873998452,-1.12337892924114,-6.27616716589239));
#12236=CARTESIAN_POINT('Ctrl Pts',(3.89970733313321,-1.12134057505243,-6.27571875966038));
#12237=CARTESIAN_POINT('Ctrl Pts',(3.91125648179073,-1.1175579667008,-6.27490519380421));
#12238=CARTESIAN_POINT('Ctrl Pts',(3.91640313818159,-1.11583283224943,-6.27454066372616));
#12239=CARTESIAN_POINT('Ctrl Pts',(3.92742383943521,-1.1120538021081,-6.27375573405896));
#12240=CARTESIAN_POINT('Ctrl Pts',(3.93329387769254,-1.10998881389203,-6.27333498128008));
#12241=CARTESIAN_POINT('Ctrl Pts',(3.94933669339718,-1.10420192789361,-6.27217757825071));
#12242=CARTESIAN_POINT('Ctrl Pts',(3.95947470739659,-1.1003861279767,-6.27143786967141));
#12243=CARTESIAN_POINT('Ctrl Pts',(4.0065789668292,-1.08191102047812,-6.26796096808694));
#12244=CARTESIAN_POINT('Ctrl Pts',(4.04282830591753,-1.06553000843682,-6.26516801523436));
#12245=CARTESIAN_POINT('Ctrl Pts',(4.07816929763934,-1.04735427323984,-6.26232527378825));
#12246=CARTESIAN_POINT('',(2.36176890518371,-0.00054653709837472,-6.32657240471885));
#12247=CARTESIAN_POINT('Ctrl Pts',(4.07816926754759,-1.04735428871591,-6.16392277459278));
#12248=CARTESIAN_POINT('Ctrl Pts',(4.07502013789745,-1.04897387378667,-6.1641614381514));
#12249=CARTESIAN_POINT('Ctrl Pts',(4.07186366438915,-1.05057927613111,-6.16439924977879));
#12250=CARTESIAN_POINT('Ctrl Pts',(4.0570580046211,-1.05802566685627,-6.16550837055927));
#12251=CARTESIAN_POINT('Ctrl Pts',(4.04531909202946,-1.06368756380594,-6.16636942124603));
#12252=CARTESIAN_POINT('Ctrl Pts',(4.01492007998935,-1.07773247480256,-6.16855861305748));
#12253=CARTESIAN_POINT('Ctrl Pts',(3.99613067491405,-1.08582657441588,-6.16987315913917));
#12254=CARTESIAN_POINT('Ctrl Pts',(3.92342637088474,-1.11492484038397,-6.17484845673189));
#12255=CARTESIAN_POINT('Ctrl Pts',(3.86819965788022,-1.1324363532321,-6.17840090965472));
#12256=CARTESIAN_POINT('Ctrl Pts',(3.7384689278029,-1.16327636420832,-6.18665754403061));
#12257=CARTESIAN_POINT('Ctrl Pts',(3.66353338008815,-1.17363162470285,-6.19137176861899));
#12258=CARTESIAN_POINT('Ctrl Pts',(3.57774927867308,-1.17717518350043,-6.19700663723372));
#12259=CARTESIAN_POINT('Ctrl Pts',(3.56736567510591,-1.17746656738353,-6.1976923493616));
#12260=CARTESIAN_POINT('Ctrl Pts',(3.55025649072845,-1.17772024828522,-6.19882886956093));
#12261=CARTESIAN_POINT('Ctrl Pts',(3.54353253230921,-1.17776235491761,-6.19927721873989));
#12262=CARTESIAN_POINT('Ctrl Pts',(3.53138144657797,-1.17773439157945,-6.20009067093989));
#12263=CARTESIAN_POINT('Ctrl Pts',(3.52595442626198,-1.17768438768315,-6.2004551445162));
#12264=CARTESIAN_POINT('Ctrl Pts',(3.51430729473924,-1.17749655514891,-6.20123994056512));
#12265=CARTESIAN_POINT('Ctrl Pts',(3.50808756542951,-1.1773469451269,-6.20166061603618));
#12266=CARTESIAN_POINT('Ctrl Pts',(3.49104525481154,-1.17680186774773,-6.20281777272555));
#12267=CARTESIAN_POINT('Ctrl Pts',(3.48022671040027,-1.17630640125359,-6.20355731075585));
#12268=CARTESIAN_POINT('Ctrl Pts',(3.41619802949826,-1.17248850754873,-6.20796492500688));
#12269=CARTESIAN_POINT('Ctrl Pts',(3.3632639245627,-1.16570580990916,-6.21173883281912));
#12270=CARTESIAN_POINT('Ctrl Pts',(3.26388767797339,-1.14604826522759,-6.21906038791314));
#12271=CARTESIAN_POINT('Ctrl Pts',(3.21741347877128,-1.13386368021226,-6.22258574633196));
#12272=CARTESIAN_POINT('Ctrl Pts',(3.1171739077486,-1.10092131694876,-6.2303271628749));
#12273=CARTESIAN_POINT('Ctrl Pts',(3.06391587788669,-1.07898384278524,-6.23453235367495));
#12274=CARTESIAN_POINT('Ctrl Pts',(3.00353542697245,-1.04876900699087,-6.2392667417903));
#12275=CARTESIAN_POINT('Ctrl Pts',(2.99465789381907,-1.04418447178372,-6.23996182432005));
#12276=CARTESIAN_POINT('Ctrl Pts',(2.98236758599149,-1.03763807830931,-6.24092163763437));
#12277=CARTESIAN_POINT('Ctrl Pts',(2.97890497847574,-1.03577140302298,-6.24119177265377));
#12278=CARTESIAN_POINT('Ctrl Pts',(2.97294504273734,-1.03251978678107,-6.24165617245326));
#12279=CARTESIAN_POINT('Ctrl Pts',(2.97044330640134,-1.03114306198956,-6.24185093573545));
#12280=CARTESIAN_POINT('Ctrl Pts',(2.96522844310817,-1.0282485231014,-6.24225651899175));
#12281=CARTESIAN_POINT('Ctrl Pts',(2.96251627435219,-1.02672904104821,-6.24246722634055));
#12282=CARTESIAN_POINT('Ctrl Pts',(2.95585386489402,-1.02296171498635,-6.24298433774796));
#12283=CARTESIAN_POINT('Ctrl Pts',(2.95191050791039,-1.02070168099378,-6.2432899815758));
#12284=CARTESIAN_POINT('Ctrl Pts',(2.94340110036748,-1.01575907333391,-6.2439488309938));
#12285=CARTESIAN_POINT('Ctrl Pts',(2.93883983768375,-1.01306840405904,-6.24430154955885));
#12286=CARTESIAN_POINT('Ctrl Pts',(2.92591943657737,-1.00532877153501,-6.2452998697766));
#12287=CARTESIAN_POINT('Ctrl Pts',(2.91760452837382,-1.00020636171451,-6.24594137364636));
#12288=CARTESIAN_POINT('Ctrl Pts',(2.8179306268496,-0.937078510063803,-6.25363173075393));
#12289=CARTESIAN_POINT('Ctrl Pts',(2.73491309237749,-0.866845794405199,
-6.26008252479646));
#12290=CARTESIAN_POINT('Ctrl Pts',(2.63247693962192,-0.752603676590605,
-6.26973223623096));
#12291=CARTESIAN_POINT('Ctrl Pts',(2.60427004674549,-0.717249100912236,
-6.27262167856772));
#12292=CARTESIAN_POINT('Ctrl Pts',(2.5720154942144,-0.671673499634032,-6.27629178582774));
#12293=CARTESIAN_POINT('Ctrl Pts',(2.56598321513033,-0.662899982391096,
-6.27699583340061));
#12294=CARTESIAN_POINT('Ctrl Pts',(2.55660376281455,-0.648854050060129,
-6.27811976698117));
#12295=CARTESIAN_POINT('Ctrl Pts',(2.55317805315021,-0.643634582245182,
-6.27853672982177));
#12296=CARTESIAN_POINT('Ctrl Pts',(2.54685336424678,-0.633829102451121,
-6.27931890025064));
#12297=CARTESIAN_POINT('Ctrl Pts',(2.54394424947677,-0.629249799094225,
-6.27968372255175));
#12298=CARTESIAN_POINT('Ctrl Pts',(2.53751628278764,-0.618975228331711,
-6.28050133526381));
#12299=CARTESIAN_POINT('Ctrl Pts',(2.53401416656813,-0.613269765260091,
-6.2809547188123));
#12300=CARTESIAN_POINT('Ctrl Pts',(2.52380769317362,-0.596319455365579,
-6.28229999308776));
#12301=CARTESIAN_POINT('Ctrl Pts',(2.51724216183954,-0.58499264371845,-6.28319680468622));
#12302=CARTESIAN_POINT('Ctrl Pts',(2.47459868707184,-0.508513525002157,
-6.28924015643022));
#12303=CARTESIAN_POINT('Ctrl Pts',(2.44458810527291,-0.440186269604555,
-6.29459813975347));
#12304=CARTESIAN_POINT('Ctrl Pts',(2.40233468674374,-0.31230534810237,-6.30445551052623));
#12305=CARTESIAN_POINT('Ctrl Pts',(2.38785279992235,-0.253748219962056,
-6.30890480807214));
#12306=CARTESIAN_POINT('Ctrl Pts',(2.37391599007045,-0.170444927584836,
-6.31498108973219));
#12307=CARTESIAN_POINT('Ctrl Pts',(2.37065634078007,-0.146431277923936,
-6.31670307685991));
#12308=CARTESIAN_POINT('Ctrl Pts',(2.36736115857779,-0.114878645864958,
-6.31891342905543));
#12309=CARTESIAN_POINT('Ctrl Pts',(2.36665386830848,-0.107417403179678,
-6.31943229790962));
#12310=CARTESIAN_POINT('Ctrl Pts',(2.36569356785916,-0.0961425922919509,
-6.32021012063123));
#12311=CARTESIAN_POINT('Ctrl Pts',(2.36538783238512,-0.0923338802041197,
-6.3204717998406));
#12312=CARTESIAN_POINT('Ctrl Pts',(2.36488616062744,-0.0856783441053184,
-6.32092711679869));
#12313=CARTESIAN_POINT('Ctrl Pts',(2.36468202953945,-0.0828322363160884,
-6.32112119594855));
#12314=CARTESIAN_POINT('Ctrl Pts',(2.36429238112494,-0.0771080744679768,
-6.32151026492637));
#12315=CARTESIAN_POINT('Ctrl Pts',(2.36410709099576,-0.0742300846150639,
-6.3217052432612));
#12316=CARTESIAN_POINT('Ctrl Pts',(2.36371711101524,-0.0678047693212115,
-6.32213918163124));
#12317=CARTESIAN_POINT('Ctrl Pts',(2.363517897987,-0.0642571219988517,-6.32237784686789));
#12318=CARTESIAN_POINT('Ctrl Pts',(2.36292394846307,-0.0527497829958561,
-6.3231491442723));
#12319=CARTESIAN_POINT('Ctrl Pts',(2.36259393512665,-0.0447867705160469,
-6.32367845805451));
#12320=CARTESIAN_POINT('Ctrl Pts',(2.361966673931,-0.0247329843330736,-6.32500172323627));
#12321=CARTESIAN_POINT('Ctrl Pts',(2.36177477434794,-0.0126396599709577,
-6.32579080616873));
#12322=CARTESIAN_POINT('Ctrl Pts',(2.36176917656931,-0.000545103328149681,
-6.3265729688034));
#12323=CARTESIAN_POINT('Ctrl Pts',(2.36176917724781,-0.000546567323186017,
-6.32657287412589));
#12324=CARTESIAN_POINT('Ctrl Pts',(2.36171530663473,0.115534480745993,-6.33407991441413));
#12325=CARTESIAN_POINT('Ctrl Pts',(2.37882206593073,0.231003657072712,-6.34096235474007));
#12326=CARTESIAN_POINT('Ctrl Pts',(2.4225690790897,0.375108283706817,-6.35053505199396));
#12327=CARTESIAN_POINT('Ctrl Pts',(2.43402570898826,0.407636583637145,-6.35275989632741));
#12328=CARTESIAN_POINT('Ctrl Pts',(2.4504739962544,0.448517614569015,-6.35566381326407));
#12329=CARTESIAN_POINT('Ctrl Pts',(2.45416514963681,0.45737739523965,-6.3562997502674));
#12330=CARTESIAN_POINT('Ctrl Pts',(2.46032068289413,0.47165812891405,-6.35733601523052));
#12331=CARTESIAN_POINT('Ctrl Pts',(2.46271866441086,0.477107360591116,-6.35773411071914));
#12332=CARTESIAN_POINT('Ctrl Pts',(2.46740263227201,0.487536119556301,-6.35850126305974));
#12333=CARTESIAN_POINT('Ctrl Pts',(2.46968225968352,0.492518346237845,-6.35887009660498));
#12334=CARTESIAN_POINT('Ctrl Pts',(2.47498299868598,0.503892889987843,-6.35971761078906));
#12335=CARTESIAN_POINT('Ctrl Pts',(2.47802705005049,0.510274219808296,-6.36019706385215));
#12336=CARTESIAN_POINT('Ctrl Pts',(2.4879037618546,0.530508174631676,-6.3617302850166));
#12337=CARTESIAN_POINT('Ctrl Pts',(2.49495131712421,0.544253479370657,-6.3627913776444));
#12338=CARTESIAN_POINT('Ctrl Pts',(2.5402995277526,0.628571939037131,-6.36942590602651));
#12339=CARTESIAN_POINT('Ctrl Pts',(2.58545749323482,0.695201083181851,-6.37524264991213));
#12340=CARTESIAN_POINT('Ctrl Pts',(2.66651818748641,0.791878135940975,-6.38449679129754));
#12341=CARTESIAN_POINT('Ctrl Pts',(2.69803786179309,0.825294592956751,-6.3878737559664));
#12342=CARTESIAN_POINT('Ctrl Pts',(2.74670532572128,0.871195998023929,-6.39270801840454));
#12343=CARTESIAN_POINT('Ctrl Pts',(2.7623660740988,0.885194569736173,-6.39421180341642));
#12344=CARTESIAN_POINT('Ctrl Pts',(2.78527100251953,0.904591710158034,-6.39632950736209));
#12345=CARTESIAN_POINT('Ctrl Pts',(2.792215177414,0.910336867578443,-6.39696124695351));
#12346=CARTESIAN_POINT('Ctrl Pts',(2.80312101522292,0.919150744606068,-6.39793666402185));
#12347=CARTESIAN_POINT('Ctrl Pts',(2.8070373148256,0.922274724105697,-6.39828364584724));
#12348=CARTESIAN_POINT('Ctrl Pts',(2.81431192422147,0.928002014933254,-6.39892193742269));
#12349=CARTESIAN_POINT('Ctrl Pts',(2.81766460111428,0.930612309732869,-6.39921369493215));
#12350=CARTESIAN_POINT('Ctrl Pts',(2.82346167656667,0.935075562273203,-6.39971392487481));
#12351=CARTESIAN_POINT('Ctrl Pts',(2.82589930564568,0.93693720732448,-6.39992298851146));
#12352=CARTESIAN_POINT('Ctrl Pts',(2.83063821674679,0.940527143910821,-6.4003269066802));
#12353=CARTESIAN_POINT('Ctrl Pts',(2.83293859276156,0.942256547915393,-6.40052184232947));
#12354=CARTESIAN_POINT('Ctrl Pts',(2.83846767274727,0.946381631088716,-6.40098772851276));
#12355=CARTESIAN_POINT('Ctrl Pts',(2.84170237659095,0.948769264203232,-6.4012581346757));
#12356=CARTESIAN_POINT('Ctrl Pts',(2.85165873670115,0.956039891179337,-6.40208407748998));
#12357=CARTESIAN_POINT('Ctrl Pts',(2.85842005590125,0.960868489329611,-6.40263614518901));
#12358=CARTESIAN_POINT('Ctrl Pts',(2.93276678021822,1.0127840964013,-6.40861779516577));
#12359=CARTESIAN_POINT('Ctrl Pts',(3.00507296977708,1.05273521884625,-6.4136520290829));
#12360=CARTESIAN_POINT('Ctrl Pts',(3.12858205517243,1.10494261304925,-6.42195271818642));
#12361=CARTESIAN_POINT('Ctrl Pts',(3.17746823006922,1.12191176245831,-6.42516744887105));
#12362=CARTESIAN_POINT('Ctrl Pts',(3.24626538962809,1.14082597568257,-6.42972779049516));
#12363=CARTESIAN_POINT('Ctrl Pts',(3.26534963038493,1.14556216770455,-6.43099614802907));
#12364=CARTESIAN_POINT('Ctrl Pts',(3.29900656622579,1.15302571457568,-6.4332452534537));
#12365=CARTESIAN_POINT('Ctrl Pts',(3.31352911292379,1.15595980457719,-6.43421963514288));
#12366=CARTESIAN_POINT('Ctrl Pts',(3.33501843609346,1.15988102066785,-6.43566900905131));
#12367=CARTESIAN_POINT('Ctrl Pts',(3.341945272507,1.16108099720014,-6.43613734425711));
#12368=CARTESIAN_POINT('Ctrl Pts',(3.35426797719213,1.16310226899619,-6.4369727251645));
#12369=CARTESIAN_POINT('Ctrl Pts',(3.3596596379837,1.16394821118643,-6.43733898916408));
#12370=CARTESIAN_POINT('Ctrl Pts',(3.37102273126913,1.16565022304492,-6.43811257552093));
#12371=CARTESIAN_POINT('Ctrl Pts',(3.37699523480088,1.16649794645077,-6.43852014703686));
#12372=CARTESIAN_POINT('Ctrl Pts',(3.39284485414717,1.16862351975635,-6.43960444865519));
#12373=CARTESIAN_POINT('Ctrl Pts',(3.40273193735257,1.16982200608203,-6.44028362177657));
#12374=CARTESIAN_POINT('Ctrl Pts',(3.44694685704018,1.17461344074678,-6.44333404853311));
#12375=CARTESIAN_POINT('Ctrl Pts',(3.48140444965084,1.17682140500423,-6.44574740149083));
#12376=CARTESIAN_POINT('Ctrl Pts',(3.61599202629003,1.17952028646134,-6.45531886249316));
#12377=CARTESIAN_POINT('Ctrl Pts',(3.71592127437108,1.16875744456909,-6.46278229060058));
#12378=CARTESIAN_POINT('Ctrl Pts',(3.83417232556991,1.14049842416938,-6.47157384106521));
#12379=CARTESIAN_POINT('Ctrl Pts',(3.85494173261071,1.13492988848359,-6.47311427078975));
#12380=CARTESIAN_POINT('Ctrl Pts',(3.88849226778399,1.12494228824751,-6.47558513499365));
#12381=CARTESIAN_POINT('Ctrl Pts',(3.90136976960366,1.12086643018572,-6.4765292143405));
#12382=CARTESIAN_POINT('Ctrl Pts',(3.91869067024776,1.11505454241571,-6.47779064581055));
#12383=CARTESIAN_POINT('Ctrl Pts',(3.92319722941423,1.11351192484223,-6.47811806772425));
#12384=CARTESIAN_POINT('Ctrl Pts',(3.93070078377988,1.11089245825476,-6.47866179151212));
#12385=CARTESIAN_POINT('Ctrl Pts',(3.93370295023513,1.10983073311865,-6.47887894750128));
#12386=CARTESIAN_POINT('Ctrl Pts',(3.93937972909166,1.10779718251264,-6.47928878301345));
#12387=CARTESIAN_POINT('Ctrl Pts',(3.942055180102,1.10682782069727,-6.47948160792783));
#12388=CARTESIAN_POINT('Ctrl Pts',(3.94838365694887,1.10450892318519,-6.47993699121781));
#12389=CARTESIAN_POINT('Ctrl Pts',(3.95203358289088,1.10315093683375,-6.48019906004639));
#12390=CARTESIAN_POINT('Ctrl Pts',(3.9648034783201,1.09832754612606,-6.48111416961166));
#12391=CARTESIAN_POINT('Ctrl Pts',(3.97388736391617,1.09476683661903,-6.48176193553076));
#12392=CARTESIAN_POINT('Ctrl Pts',(4.04922328174113,1.06415122726164,-6.48711568660296));
#12393=CARTESIAN_POINT('Ctrl Pts',(4.11293638203291,1.03121853666367,-6.49152981841795));
#12394=CARTESIAN_POINT('Ctrl Pts',(4.22264297488093,0.961180400018604,-6.49958067380963));
#12395=CARTESIAN_POINT('Ctrl Pts',(4.26959081906515,0.92602408902228,-6.50320146259553));
#12396=CARTESIAN_POINT('Ctrl Pts',(4.32967112981816,0.873614567741719,-6.50828371032867));
#12397=CARTESIAN_POINT('Ctrl Pts',(4.34523677994508,0.859279687926859,-6.50964557705863));
#12398=CARTESIAN_POINT('Ctrl Pts',(4.37164880867881,0.833607159183514,-6.51204509365738));
#12399=CARTESIAN_POINT('Ctrl Pts',(4.38267062407157,0.822457425464716,-6.51307509232735));
#12400=CARTESIAN_POINT('Ctrl Pts',(4.39841723920085,0.805878804813921,-6.51459142030952));
#12401=CARTESIAN_POINT('Ctrl Pts',(4.40332034525348,0.800621050155294,-6.51507015636227));
#12402=CARTESIAN_POINT('Ctrl Pts',(4.41187460089195,0.791277999215493,-6.51591731338677));
#12403=CARTESIAN_POINT('Ctrl Pts',(4.41554598760184,0.787211459573994,-6.51628487284406));
#12404=CARTESIAN_POINT('Ctrl Pts',(4.4231481624079,0.77867201796701,-6.51705440082348));
#12405=CARTESIAN_POINT('Ctrl Pts',(4.42707365940531,0.774194635050932,-6.51745657287766));
#12406=CARTESIAN_POINT('Ctrl Pts',(4.43724041894056,0.762419579027643,-6.51851098425855));
#12407=CARTESIAN_POINT('Ctrl Pts',(4.443426573987,0.755075128284217,-6.51916543111938));
#12408=CARTESIAN_POINT('Ctrl Pts',(4.46926795172895,0.723622520857745,-6.52195526744885));
#12409=CARTESIAN_POINT('Ctrl Pts',(4.48805223818473,0.698818326629725,-6.52412441199115));
#12410=CARTESIAN_POINT('Ctrl Pts',(4.56519469614052,0.588104637046068,-6.53368238066644));
#12411=CARTESIAN_POINT('Ctrl Pts',(4.61302577514608,0.495434471449038,-6.5414259457628));
#12412=CARTESIAN_POINT('Ctrl Pts',(4.6554252126742,0.377254909202711,-6.5505078137947));
#12413=CARTESIAN_POINT('Ctrl Pts',(4.66220009675545,0.35658829616128,-6.5520663503187));
#12414=CARTESIAN_POINT('Ctrl Pts',(4.67228065187524,0.32269427835323,-6.55456282921598));
#12415=CARTESIAN_POINT('Ctrl Pts',(4.67593566408856,0.309576748256058,-6.5555147459365));
#12416=CARTESIAN_POINT('Ctrl Pts',(4.68056496445609,0.291774076878011,-6.55678486590864));
#12417=CARTESIAN_POINT('Ctrl Pts',(4.68173924546384,0.28714267862063,-6.55711331252978));
#12418=CARTESIAN_POINT('Ctrl Pts',(4.68364988690451,0.27940982619535,-6.55765827041756));
#12419=CARTESIAN_POINT('Ctrl Pts',(4.68440188776263,0.276312343988887,-6.55787564371449));
#12420=CARTESIAN_POINT('Ctrl Pts',(4.68580086701504,0.27044619243034,-6.55828553519333));
#12421=CARTESIAN_POINT('Ctrl Pts',(4.6864504087604,0.267678175705502,-6.55847820103284));
#12422=CARTESIAN_POINT('Ctrl Pts',(4.68796364454089,0.26112289369182,-6.55893277067281));
#12423=CARTESIAN_POINT('Ctrl Pts',(4.68881864493384,0.257333624866884,-6.55919418915567));
#12424=CARTESIAN_POINT('Ctrl Pts',(4.69176545543255,0.243965987942151,-6.56011190202533));
#12425=CARTESIAN_POINT('Ctrl Pts',(4.6937564683154,0.234365483014759,-6.56076285283522));
#12426=CARTESIAN_POINT('Ctrl Pts',(4.70918494119134,0.154998574411806,-6.56608568560102));
#12427=CARTESIAN_POINT('Ctrl Pts',(4.71640577698327,0.0841623742297525,
-6.57047008952881));
#12428=CARTESIAN_POINT('Ctrl Pts',(4.71785165203879,-0.0458290387227297,
-6.57851129554207));
#12429=CARTESIAN_POINT('Ctrl Pts',(4.71408332509042,-0.104719280449985,
-6.58215306769525));
#12430=CARTESIAN_POINT('Ctrl Pts',(4.70298425418913,-0.184104733424839,
-6.58726211292166));
#12431=CARTESIAN_POINT('Ctrl Pts',(4.69947654534109,-0.205047220625451,
-6.58862855706507));
#12432=CARTESIAN_POINT('Ctrl Pts',(4.69239019521921,-0.241309477263978,
-6.59103540804927));
#12433=CARTESIAN_POINT('Ctrl Pts',(4.68906706402577,-0.256673853135453,
-6.59206809745574));
#12434=CARTESIAN_POINT('Ctrl Pts',(4.68377569653301,-0.278968785689635,
-6.5935876572805));
#12435=CARTESIAN_POINT('Ctrl Pts',(4.6820497073416,-0.285955503031096,-6.59406688760917));
#12436=CARTESIAN_POINT('Ctrl Pts',(4.67889692076402,-0.298233396502753,
-6.59491460918908));
#12437=CARTESIAN_POINT('Ctrl Pts',(4.67749701009548,-0.303531302804515,
-6.59528223511535));
#12438=CARTESIAN_POINT('Ctrl Pts',(4.67449974632466,-0.314562073954441,
-6.59605159448137));
#12439=CARTESIAN_POINT('Ctrl Pts',(4.67289581355544,-0.320292973682849,
-6.59645352939703));
#12440=CARTESIAN_POINT('Ctrl Pts',(4.66859483546785,-0.335223568166869,
-6.59750662742625));
#12441=CARTESIAN_POINT('Ctrl Pts',(4.66582881910959,-0.344402765041082,
-6.59815998793711));
#12442=CARTESIAN_POINT('Ctrl Pts',(4.65365848927878,-0.383075250196805,
-6.60093845193831));
#12443=CARTESIAN_POINT('Ctrl Pts',(4.64320611574455,-0.412223110009007,
-6.6030969666943));
#12444=CARTESIAN_POINT('Ctrl Pts',(4.60051707690937,-0.517957341431438,
-6.61117231157706));
#12445=CARTESIAN_POINT('Ctrl Pts',(4.5613549439675,-0.591476687592265,-6.61729559025054));
#12446=CARTESIAN_POINT('Ctrl Pts',(4.4855554575964,-0.703441735428664,-6.62719319371163));
#12447=CARTESIAN_POINT('Ctrl Pts',(4.45347712905797,-0.744645613169313,
-6.63097701400828));
#12448=CARTESIAN_POINT('Ctrl Pts',(4.4141403374804,-0.788784548749866,-6.63508921453577));
#12449=CARTESIAN_POINT('Ctrl Pts',(4.40946568440461,-0.793937226733229,
-6.63557019747927));
#12450=CARTESIAN_POINT('Ctrl Pts',(4.40226179869619,-0.801737746749021,
-6.63629938053248));
#12451=CARTESIAN_POINT('Ctrl Pts',(4.39976552033298,-0.80441561159858,-6.63654989308485));
#12452=CARTESIAN_POINT('Ctrl Pts',(4.39517249770622,-0.809296911723115,
-6.63700681164602));
#12453=CARTESIAN_POINT('Ctrl Pts',(4.3930796968975,-0.811503873317242,-6.63721349352151));
#12454=CARTESIAN_POINT('Ctrl Pts',(4.38833551473673,-0.816468189299387,
-6.63767864080093));
#12455=CARTESIAN_POINT('Ctrl Pts',(4.38567923454699,-0.819220750508467,
-6.63793672817168));
#12456=CARTESIAN_POINT('Ctrl Pts',(4.3787787185151,-0.826302016088787,-6.63860130412161));
#12457=CARTESIAN_POINT('Ctrl Pts',(4.37451432475022,-0.830611044921556,
-6.63900630920203));
#12458=CARTESIAN_POINT('Ctrl Pts',(4.34565856595261,-0.859322008509864,
-6.64171055390627));
#12459=CARTESIAN_POINT('Ctrl Pts',(4.3200315506661,-0.882664134852977,-6.64393724589545));
#12460=CARTESIAN_POINT('Ctrl Pts',(4.2717270343421,-0.922910097270403,-6.6479100790801));
#12461=CARTESIAN_POINT('Ctrl Pts',(4.24940087593044,-0.940191200882933,
-6.64966740446288));
#12462=CARTESIAN_POINT('Ctrl Pts',(4.18750710597177,-0.984635972691225,
-6.654391835549));
#12463=CARTESIAN_POINT('Ctrl Pts',(4.14686698557342,-1.01021033045519,-6.6573419860796));
#12464=CARTESIAN_POINT('Ctrl Pts',(4.09596916778885,-1.03805549725572,-6.66097008034091));
#12465=CARTESIAN_POINT('Ctrl Pts',(4.08709787329504,-1.04276234184578,-6.66160001813117));
#12466=CARTESIAN_POINT('Ctrl Pts',(4.07816925191529,-1.04735429675555,-6.66223230003384));
#12467=CARTESIAN_POINT('Origin',(3.53951905042299,8.32667268468867E-16,
0.924367114736157));
#12468=CARTESIAN_POINT('',(4.07816926754786,-1.04735428871577,-7.26048212650804));
#12469=CARTESIAN_POINT('',(4.0781692089456,-1.04735431885469,-7.16215973101906));
#12470=CARTESIAN_POINT('',(4.07816926754759,-1.04735428871592,0.924367114736157));
#12471=CARTESIAN_POINT('',(2.36176955567229,0.00102997123974061,-6.92455466901993));
#12472=CARTESIAN_POINT('Ctrl Pts',(4.07816926754783,-1.04735428871579,-7.26048212650804));
#12473=CARTESIAN_POINT('Ctrl Pts',(4.0791210384006,-1.04686479668619,-7.26040895432542));
#12474=CARTESIAN_POINT('Ctrl Pts',(4.08007214743775,-1.0463740045061,-7.26033586072063));
#12475=CARTESIAN_POINT('Ctrl Pts',(4.08372394638214,-1.04448329195444,-7.26005532686991));
#12476=CARTESIAN_POINT('Ctrl Pts',(4.08641986423175,-1.04307421425932,-7.25984846229205));
#12477=CARTESIAN_POINT('Ctrl Pts',(4.09234881626624,-1.03994601750304,-7.25939404491509));
#12478=CARTESIAN_POINT('Ctrl Pts',(4.09557930866954,-1.03822225916838,-7.25914678372801));
#12479=CARTESIAN_POINT('Ctrl Pts',(4.10492562876973,-1.03317901863033,-7.25843224090554));
#12480=CARTESIAN_POINT('Ctrl Pts',(4.11102027058487,-1.02982029719037,-7.25796732132046));
#12481=CARTESIAN_POINT('Ctrl Pts',(4.16258002015432,-1.00080730824881,-7.2540398349102));
#12482=CARTESIAN_POINT('Ctrl Pts',(4.20632906893002,-0.972206821970832,
-7.25074380492524));
#12483=CARTESIAN_POINT('Ctrl Pts',(4.31449867956874,-0.890743150276272,
-7.24230877133553));
#12484=CARTESIAN_POINT('Ctrl Pts',(4.37546338937657,-0.833794612940169,
-7.23724602807653));
#12485=CARTESIAN_POINT('Ctrl Pts',(4.45008209734152,-0.747608828442086,
-7.22997481502585));
#12486=CARTESIAN_POINT('Ctrl Pts',(4.46932267187858,-0.723539212705974,
-7.22798191619663));
#12487=CARTESIAN_POINT('Ctrl Pts',(4.49327538620863,-0.691039458935407,
-7.22532121204929));
#12488=CARTESIAN_POINT('Ctrl Pts',(4.49885993192031,-0.683265501877888,
-7.2246869698913));
#12489=CARTESIAN_POINT('Ctrl Pts',(4.50776034052246,-0.670551452851053,
-7.22365274462778));
#12490=CARTESIAN_POINT('Ctrl Pts',(4.51113468905718,-0.665652683716904,
-7.22325497685624));
#12491=CARTESIAN_POINT('Ctrl Pts',(4.51754704970258,-0.656190783863797,
-7.22248796033129));
#12492=CARTESIAN_POINT('Ctrl Pts',(4.52059060355455,-0.651631581567085,
-7.22211893133012));
#12493=CARTESIAN_POINT('Ctrl Pts',(4.52756107757768,-0.641030373930713,
-7.22126204035052));
#12494=CARTESIAN_POINT('Ctrl Pts',(4.53146456088762,-0.634973297076931,
-7.22077333133698));
#12495=CARTESIAN_POINT('Ctrl Pts',(4.54373056030214,-0.615550863422892,
-7.21920879819117));
#12496=CARTESIAN_POINT('Ctrl Pts',(4.55188009666416,-0.6020537288065,-7.2181253392048));
#12497=CARTESIAN_POINT('Ctrl Pts',(4.57040407276885,-0.569934558620777,
-7.21555456661155));
#12498=CARTESIAN_POINT('Ctrl Pts',(4.58054845669689,-0.551186908442242,
-7.21405977016025));
#12499=CARTESIAN_POINT('Ctrl Pts',(4.61698809842442,-0.479245130209868,
-7.20834463453967));
#12500=CARTESIAN_POINT('Ctrl Pts',(4.63975718209956,-0.424370209527562,
-7.20402195141923));
#12501=CARTESIAN_POINT('Ctrl Pts',(4.68031292177284,-0.301081408911668,
-7.19450082427979));
#12502=CARTESIAN_POINT('Ctrl Pts',(4.69628223715173,-0.23229590519864,-7.18930747221862));
#12503=CARTESIAN_POINT('Ctrl Pts',(4.70736193492338,-0.152756788635022,
-7.18367885848958));
#12504=CARTESIAN_POINT('Ctrl Pts',(4.70859595856498,-0.143006426131493,
-7.18299538101601));
#12505=CARTESIAN_POINT('Ctrl Pts',(4.71014773044312,-0.129378031055884,
-7.1820501629168));
#12506=CARTESIAN_POINT('Ctrl Pts',(4.71056849564459,-0.125512466811791,
-7.18178319216913));
#12507=CARTESIAN_POINT('Ctrl Pts',(4.71126390343153,-0.118815624456901,
-7.18132272118901));
#12508=CARTESIAN_POINT('Ctrl Pts',(4.71154744425036,-0.115985333850374,
-7.1811287417708));
#12509=CARTESIAN_POINT('Ctrl Pts',(4.71212691884321,-0.10998184297856,-7.18071865482951));
#12510=CARTESIAN_POINT('Ctrl Pts',(4.71242023242729,-0.106808410875968,
-7.18050269838268));
#12511=CARTESIAN_POINT('Ctrl Pts',(4.71312072562801,-0.0988785091499942,
-7.17996500435443));
#12512=CARTESIAN_POINT('Ctrl Pts',(4.71351187940819,-0.0941206197330737,
-7.17964413933385));
#12513=CARTESIAN_POINT('Ctrl Pts',(4.71490461659455,-0.0758175651574341,
-7.17841607212677));
#12514=CARTESIAN_POINT('Ctrl Pts',(4.71570084347704,-0.0622572163110699,
-7.17751940029991));
#12515=CARTESIAN_POINT('Ctrl Pts',(4.71715802779972,-0.0270365754443105,
-7.17521758072504));
#12516=CARTESIAN_POINT('Ctrl Pts',(4.71745617129102,-0.00536577729133605,
-7.17382785174512));
#12517=CARTESIAN_POINT('Ctrl Pts',(4.71573566097996,0.118920575617957,-7.16594793532118));
#12518=CARTESIAN_POINT('Ctrl Pts',(4.7009090513346,0.220914048676916,-7.1597954908354));
#12519=CARTESIAN_POINT('Ctrl Pts',(4.66431207532299,0.350672797991655,-7.15120964144321));
#12520=CARTESIAN_POINT('Ctrl Pts',(4.65431106422306,0.381273179406102,-7.14913014551336));
#12521=CARTESIAN_POINT('Ctrl Pts',(4.63967459309447,0.420532210610792,-7.14636981466399));
#12522=CARTESIAN_POINT('Ctrl Pts',(4.63616623923376,0.429598058892855,-7.14572585942135));
#12523=CARTESIAN_POINT('Ctrl Pts',(4.63031871311958,0.444169933965177,-7.14467971145538));
#12524=CARTESIAN_POINT('Ctrl Pts',(4.62804906182708,0.449703509457974,-7.14427983136713));
#12525=CARTESIAN_POINT('Ctrl Pts',(4.62362239022782,0.460266176901633,-7.14351139261523));
#12526=CARTESIAN_POINT('Ctrl Pts',(4.62147226990143,0.465298005693713,-7.14314307315783));
#12527=CARTESIAN_POINT('Ctrl Pts',(4.61643773921654,0.476856494180382,-7.14229171841119));
#12528=CARTESIAN_POINT('Ctrl Pts',(4.61352894725653,0.483372233315901,-7.14180787135677));
#12529=CARTESIAN_POINT('Ctrl Pts',(4.60416435443203,0.503847170335354,-7.14027477490588));
#12530=CARTESIAN_POINT('Ctrl Pts',(4.5974944618875,0.517706079155251,-7.13921831706065));
#12531=CARTESIAN_POINT('Ctrl Pts',(4.58124366558678,0.549846119485413,-7.13672284330316));
#12532=CARTESIAN_POINT('Ctrl Pts',(4.57145005041813,0.568013425182072,-7.13527692622006));
#12533=CARTESIAN_POINT('Ctrl Pts',(4.53327934984958,0.63457225533011,-7.12984584248786));
#12534=CARTESIAN_POINT('Ctrl Pts',(4.50193633311551,0.681170461710787,-7.12576922185289));
#12535=CARTESIAN_POINT('Ctrl Pts',(4.4210017810568,0.784702493667794,-7.11613628728554));
#12536=CARTESIAN_POINT('Ctrl Pts',(4.36901626240151,0.839467732045456,-7.11056922925221));
#12537=CARTESIAN_POINT('Ctrl Pts',(4.30494733946576,0.895156807276934,-7.10462289367839));
#12538=CARTESIAN_POINT('Ctrl Pts',(4.29766696994318,0.901331194321186,-7.10395929873762));
#12539=CARTESIAN_POINT('Ctrl Pts',(4.28733913469973,0.909876405250098,-7.10303570768108));
#12540=CARTESIAN_POINT('Ctrl Pts',(4.28435409219315,0.912321606057675,-7.10277081078597));
#12541=CARTESIAN_POINT('Ctrl Pts',(4.27893459410847,0.916716664978687,-7.10229364718935));
#12542=CARTESIAN_POINT('Ctrl Pts',(4.27650431216894,0.918671603386434,-7.1020810283009));
#12543=CARTESIAN_POINT('Ctrl Pts',(4.27151367795629,0.922653559735491,-7.10164722793083));
#12544=CARTESIAN_POINT('Ctrl Pts',(4.26895261695194,0.924679619495199,-7.10142611262159));
#12545=CARTESIAN_POINT('Ctrl Pts',(4.26234095325326,0.929865555141514,-7.10085902767194));
#12546=CARTESIAN_POINT('Ctrl Pts',(4.25827799028721,0.933009669095838,-7.10051413941098));
#12547=CARTESIAN_POINT('Ctrl Pts',(4.24102359068131,0.946182340578814,-7.09906397122429));
#12548=CARTESIAN_POINT('Ctrl Pts',(4.22764112376203,0.955959058714413,-7.09797470867935));
#12549=CARTESIAN_POINT('Ctrl Pts',(4.1904146663823,0.981968279526118,-7.09502693918456));
#12550=CARTESIAN_POINT('Ctrl Pts',(4.16617292585347,0.997613130239746,-7.09319681941355));
#12551=CARTESIAN_POINT('Ctrl Pts',(4.06396078936841,1.05837992662433,-7.08573714744645));
#12552=CARTESIAN_POINT('Ctrl Pts',(3.98151966398361,1.09537351101818,-7.08029034884683));
#12553=CARTESIAN_POINT('Ctrl Pts',(3.86374415862517,1.1327377199476,-7.0724330627609));
#12554=CARTESIAN_POINT('Ctrl Pts',(3.83140697363367,1.14149804262041,-7.07027151766898));
#12555=CARTESIAN_POINT('Ctrl Pts',(3.7891187116076,1.1510397069154,-7.06741640472314));
#12556=CARTESIAN_POINT('Ctrl Pts',(3.77946813094281,1.15309012085085,-7.06676300706239));
#12557=CARTESIAN_POINT('Ctrl Pts',(3.76389662643314,1.15619458442182,-7.06570526355605));
#12558=CARTESIAN_POINT('Ctrl Pts',(3.75799126644132,1.1573249769293,-7.06530332651568));
#12559=CARTESIAN_POINT('Ctrl Pts',(3.74670380254696,1.15939613203936,-7.06453342886018));
#12560=CARTESIAN_POINT('Ctrl Pts',(3.74132328686276,1.16034475951355,-7.06416572599855));
#12561=CARTESIAN_POINT('Ctrl Pts',(3.72896423821972,1.16243519633773,-7.06331939722583));
#12562=CARTESIAN_POINT('Ctrl Pts',(3.7219816897657,1.16355165176923,-7.06283999164924));
#12563=CARTESIAN_POINT('Ctrl Pts',(3.70012532011317,1.16684474223184,-7.06133524645699));
#12564=CARTESIAN_POINT('Ctrl Pts',(3.68522011240307,1.16879946555535,-7.06030307214294));
#12565=CARTESIAN_POINT('Ctrl Pts',(3.65037241594901,1.1726926020889,-7.05787485732478));
#12566=CARTESIAN_POINT('Ctrl Pts',(3.63041024933091,1.17440841101419,-7.0564724128042));
#12567=CARTESIAN_POINT('Ctrl Pts',(3.55717262922423,1.17882503985399,-7.05128454953918));
#12568=CARTESIAN_POINT('Ctrl Pts',(3.50377923600831,1.17841489720657,-7.04741645188211));
#12569=CARTESIAN_POINT('Ctrl Pts',(3.37128271906969,1.16838321756274,-7.03768549736953));
#12570=CARTESIAN_POINT('Ctrl Pts',(3.29276967058799,1.15435673735584,-7.03179312721365));
#12571=CARTESIAN_POINT('Ctrl Pts',(3.20799161631081,1.13015868902606,-7.02562057644877));
#12572=CARTESIAN_POINT('Ctrl Pts',(3.19974327642594,1.12770631634214,-7.02502226540288));
#12573=CARTESIAN_POINT('Ctrl Pts',(3.18718404317643,1.12382192790666,-7.02411543887595));
#12574=CARTESIAN_POINT('Ctrl Pts',(3.18285352568081,1.12245507176932,-7.02380352383687));
#12575=CARTESIAN_POINT('Ctrl Pts',(3.17557192389653,1.12011035848703,-7.02328046749271));
#12576=CARTESIAN_POINT('Ctrl Pts',(3.17261663866611,1.11914581140252,-7.02306857708582));
#12577=CARTESIAN_POINT('Ctrl Pts',(3.16654985692893,1.1171391184539,-7.02263445641438));
#12578=CARTESIAN_POINT('Ctrl Pts',(3.16343884642749,1.11609565455025,-7.02241230380538));
#12579=CARTESIAN_POINT('Ctrl Pts',(3.15540058745813,1.11336211637116,-7.02183940157568));
#12580=CARTESIAN_POINT('Ctrl Pts',(3.15048005177301,1.11165230886274,-7.02148977618183));
#12581=CARTESIAN_POINT('Ctrl Pts',(3.12964028181421,1.10425550228127,-7.0200129248423));
#12582=CARTESIAN_POINT('Ctrl Pts',(3.11383222540537,1.0982584478319,-7.01890235942144));
#12583=CARTESIAN_POINT('Ctrl Pts',(3.07047355563768,1.08073263222544,-7.01586891152624));
#12584=CARTESIAN_POINT('Ctrl Pts',(3.04322286992921,1.06849288819651,-7.01397664954022));
#12585=CARTESIAN_POINT('Ctrl Pts',(2.92067289526724,1.00774758908265,-7.00540645995481));
#12586=CARTESIAN_POINT('Ctrl Pts',(2.83179755056081,0.947447136530567,-6.99896834281064));
#12587=CARTESIAN_POINT('Ctrl Pts',(2.73802478613671,0.863173903915375,-6.99080402974186));
#12588=CARTESIAN_POINT('Ctrl Pts',(2.72408796947361,0.850020193533559,-6.98955063881296));
#12589=CARTESIAN_POINT('Ctrl Pts',(2.70479918924047,0.830904180454798,-6.98775394633782));
#12590=CARTESIAN_POINT('Ctrl Pts',(2.69917714512367,0.825217838336029,-6.98722247997151));
#12591=CARTESIAN_POINT('Ctrl Pts',(2.6897436626013,0.815480095705618,-6.98631708987481));
#12592=CARTESIAN_POINT('Ctrl Pts',(2.68590217489836,0.811458085335159,-6.98594447207879));
#12593=CARTESIAN_POINT('Ctrl Pts',(2.67819411719149,0.803272498089551,-6.98518871210472));
#12594=CARTESIAN_POINT('Ctrl Pts',(2.67432890548019,0.799107851257122,-6.98480552677368));
#12595=CARTESIAN_POINT('Ctrl Pts',(2.66540850215684,0.789355803408201,-6.98391121726921));
#12596=CARTESIAN_POINT('Ctrl Pts',(2.66037654132012,0.783747586331053,-6.98339914477914));
#12597=CARTESIAN_POINT('Ctrl Pts',(2.64222170240549,0.763118832124705,-6.98152333159484));
#12598=CARTESIAN_POINT('Ctrl Pts',(2.62942778510317,0.747814607760834,-6.98014637455723));
#12599=CARTESIAN_POINT('Ctrl Pts',(2.59874059627809,0.709151862477085,-6.97670125298433));
#12600=CARTESIAN_POINT('Ctrl Pts',(2.58132305717579,0.685434650845956,-6.97461647779052));
#12601=CARTESIAN_POINT('Ctrl Pts',(2.53484419726017,0.616906754337731,-6.96867491154743));
#12602=CARTESIAN_POINT('Ctrl Pts',(2.50791691668799,0.570737906001056,-6.96476271389434));
#12603=CARTESIAN_POINT('Ctrl Pts',(2.45676075446857,0.467497000174545,-6.95630659854012));
#12604=CARTESIAN_POINT('Ctrl Pts',(2.4337093016752,0.410006441491091,-6.95177275174832));
#12605=CARTESIAN_POINT('Ctrl Pts',(2.412293817439,0.341406839854758,-6.94673332944894));
#12606=CARTESIAN_POINT('Ctrl Pts',(2.40943139879548,0.331809090270396,-6.94603654360019));
#12607=CARTESIAN_POINT('Ctrl Pts',(2.40561440271821,0.31838784525321,-6.9450747514714));
#12608=CARTESIAN_POINT('Ctrl Pts',(2.40455614928163,0.314594634788478,-6.94480431328668));
#12609=CARTESIAN_POINT('Ctrl Pts',(2.40276302248338,0.308040512244304,-6.94433951461768));
#12610=CARTESIAN_POINT('Ctrl Pts',(2.4020191409051,0.305282132676973,-6.94414465389109));
#12611=CARTESIAN_POINT('Ctrl Pts',(2.40047052317772,0.299455466884699,-6.94373467133754));
#12612=CARTESIAN_POINT('Ctrl Pts',(2.39966813213276,0.296386586367043,-6.94351969017118));
#12613=CARTESIAN_POINT('Ctrl Pts',(2.39770710240917,0.288760536575892,-6.94298775343229));
#12614=CARTESIAN_POINT('Ctrl Pts',(2.39656332223055,0.284199537950749,-6.94267163054727));
#12615=CARTESIAN_POINT('Ctrl Pts',(2.39415621230736,0.274351200446754,-6.94199314472811));
#12616=CARTESIAN_POINT('Ctrl Pts',(2.3929021048578,0.269061693552751,-6.94163127155982));
#12617=CARTESIAN_POINT('Ctrl Pts',(2.38941377332809,0.253881329908542,-6.94059949593436));
#12618=CARTESIAN_POINT('Ctrl Pts',(2.38727054037059,0.243969802280411,-6.93993403143119));
#12619=CARTESIAN_POINT('Ctrl Pts',(2.3697068138731,0.157343976556934,-6.934179407255));
#12620=CARTESIAN_POINT('Ctrl Pts',(2.36183797518918,0.0792913967190124,
-6.92940337711709));
#12621=CARTESIAN_POINT('Ctrl Pts',(2.36176950122289,0.00103046541328306,
-6.92455479479514));
#12622=CARTESIAN_POINT('Ctrl Pts',(2.36176950078553,0.00102996541417458,
-6.92455476381816));
#12623=CARTESIAN_POINT('Ctrl Pts',(2.36170919468074,-0.067929134354621,
-6.92028246753168));
#12624=CARTESIAN_POINT('Ctrl Pts',(2.36770518372916,-0.1367539347171,-6.915970531133));
#12625=CARTESIAN_POINT('Ctrl Pts',(2.38139014680442,-0.214309562451292,
-6.91082537945449));
#12626=CARTESIAN_POINT('Ctrl Pts',(2.38321387131569,-0.223940772383019,
-6.91018151456286));
#12627=CARTESIAN_POINT('Ctrl Pts',(2.38643756776599,-0.239874597967229,
-6.90910753605252));
#12628=CARTESIAN_POINT('Ctrl Pts',(2.38776954649811,-0.246190588509361,
-6.90867952474163));
#12629=CARTESIAN_POINT('Ctrl Pts',(2.39026544663821,-0.25756188507796,-6.90790462094745));
#12630=CARTESIAN_POINT('Ctrl Pts',(2.3914109839286,-0.262621089513881,-6.9075583114395));
#12631=CARTESIAN_POINT('Ctrl Pts',(2.39382185310142,-0.272951236309381,
-6.90684794636779));
#12632=CARTESIAN_POINT('Ctrl Pts',(2.39509022643722,-0.278221333662394,
-6.90648380227523));
#12633=CARTESIAN_POINT('Ctrl Pts',(2.39791732375754,-0.289621417142105,
-6.90569223386097));
#12634=CARTESIAN_POINT('Ctrl Pts',(2.39948913248429,-0.295747951984234,
-6.90526440286357));
#12635=CARTESIAN_POINT('Ctrl Pts',(2.40393089073505,-0.312499138139667,
-6.90408779205807));
#12636=CARTESIAN_POINT('Ctrl Pts',(2.40690047373151,-0.323096464302741,
-6.90333585776163));
#12637=CARTESIAN_POINT('Ctrl Pts',(2.42482907262387,-0.383789859677081,
-6.89898436493865));
#12638=CARTESIAN_POINT('Ctrl Pts',(2.4429600617432,-0.432880355212411,-6.8952835756504));
#12639=CARTESIAN_POINT('Ctrl Pts',(2.4838735253723,-0.524414922717426,-6.88803953382313));
#12640=CARTESIAN_POINT('Ctrl Pts',(2.50611729994515,-0.566991061716404,
-6.88451543417852));
#12641=CARTESIAN_POINT('Ctrl Pts',(2.56116444011136,-0.658296552316439,
-6.87669277199488));
#12642=CARTESIAN_POINT('Ctrl Pts',(2.59514384381577,-0.706179144703532,
-6.87240518397654));
#12643=CARTESIAN_POINT('Ctrl Pts',(2.63871565185895,-0.758776422832698,
-6.86762062593331));
#12644=CARTESIAN_POINT('Ctrl Pts',(2.64497122427565,-0.76614138671602,-6.86694892914909));
#12645=CARTESIAN_POINT('Ctrl Pts',(2.65410555721875,-0.776631212399946,
-6.86599072269893));
#12646=CARTESIAN_POINT('Ctrl Pts',(2.65691149273527,-0.779818565141312,
-6.86569936452814));
#12647=CARTESIAN_POINT('Ctrl Pts',(2.66178738811554,-0.785297220839857,
-6.86519830526048));
#12648=CARTESIAN_POINT('Ctrl Pts',(2.6638492132091,-0.787595666053827,-6.86498802206589));
#12649=CARTESIAN_POINT('Ctrl Pts',(2.66820043557348,-0.792408035160965,
-6.86454761792684));
#12650=CARTESIAN_POINT('Ctrl Pts',(2.67049169991478,-0.794920176859078,
-6.86431763847893));
#12651=CARTESIAN_POINT('Ctrl Pts',(2.67668437976571,-0.801651053360571,
-6.86370111310438));
#12652=CARTESIAN_POINT('Ctrl Pts',(2.68060590459111,-0.805851283730036,
-6.86331603163618));
#12653=CARTESIAN_POINT('Ctrl Pts',(2.69859871933711,-0.824842298223499,
-6.86157235238685));
#12654=CARTESIAN_POINT('Ctrl Pts',(2.71302329995988,-0.839295368444953,
-6.86023816056863));
#12655=CARTESIAN_POINT('Ctrl Pts',(2.78597322101274,-0.908683528060233,
-6.85375137573298));
#12656=CARTESIAN_POINT('Ctrl Pts',(2.8496366286983,-0.957915354664559,-6.84887499095558));
#12657=CARTESIAN_POINT('Ctrl Pts',(2.95440713323276,-1.02303224210467,-6.8412091100522));
#12658=CARTESIAN_POINT('Ctrl Pts',(2.99221324381584,-1.04374653801709,-6.8385081516993));
#12659=CARTESIAN_POINT('Ctrl Pts',(3.04690171233199,-1.06992121100906,-6.83461753571593));
#12660=CARTESIAN_POINT('Ctrl Pts',(3.06290328524702,-1.07714465325082,-6.83348127574796));
#12661=CARTESIAN_POINT('Ctrl Pts',(3.09143455460048,-1.08926402428989,-6.83145454376817));
#12662=CARTESIAN_POINT('Ctrl Pts',(3.10389805971806,-1.09430807292105,-6.83056895845158));
#12663=CARTESIAN_POINT('Ctrl Pts',(3.12257297279339,-1.10149632303885,-6.82924034775368));
#12664=CARTESIAN_POINT('Ctrl Pts',(3.12872067800373,-1.10380382116081,-6.82880271045113));
#12665=CARTESIAN_POINT('Ctrl Pts',(3.14000647019486,-1.10793252248344,-6.82799866813231));
#12666=CARTESIAN_POINT('Ctrl Pts',(3.14513855047203,-1.10976970389853,-6.82763279955168));
#12667=CARTESIAN_POINT('Ctrl Pts',(3.15600984688852,-1.1135764768967,-6.8268571828388));
#12668=CARTESIAN_POINT('Ctrl Pts',(3.16175188380064,-1.11553746890858,-6.82644716597567));
#12669=CARTESIAN_POINT('Ctrl Pts',(3.17710907756102,-1.12065001472731,-6.82534950274754));
#12670=CARTESIAN_POINT('Ctrl Pts',(3.18674994830207,-1.12372211576038,-6.82465930570032));
#12671=CARTESIAN_POINT('Ctrl Pts',(3.2306282311633,-1.13708380167775,-6.82151218747376));
#12672=CARTESIAN_POINT('Ctrl Pts',(3.26528047917392,-1.14593448819666,-6.81900995488147));
#12673=CARTESIAN_POINT('Ctrl Pts',(3.38624125856184,-1.17102886747839,-6.81021398054998));
#12674=CARTESIAN_POINT('Ctrl Pts',(3.47392299217035,-1.1791932018851,-6.8037069410587));
#12675=CARTESIAN_POINT('Ctrl Pts',(3.60371246515373,-1.17675037546062,-6.79424928101347));
#12676=CARTESIAN_POINT('Ctrl Pts',(3.64567538323102,-1.17370945192453,-6.79122406196703));
#12677=CARTESIAN_POINT('Ctrl Pts',(3.6940468309022,-1.16758779123739,-6.78783531294426));
#12678=CARTESIAN_POINT('Ctrl Pts',(3.70069650445169,-1.16668844117385,-6.78737165789985));
#12679=CARTESIAN_POINT('Ctrl Pts',(3.7109106955437,-1.16521800227792,-6.78666321539333));
#12680=CARTESIAN_POINT('Ctrl Pts',(3.71448074850584,-1.16468729448425,-6.78641630807778));
#12681=CARTESIAN_POINT('Ctrl Pts',(3.72105872643431,-1.16367851399729,-6.78596274375536));
#12682=CARTESIAN_POINT('Ctrl Pts',(3.72406723659236,-1.16320518622926,-6.78575583940993));
#12683=CARTESIAN_POINT('Ctrl Pts',(3.7309147060906,-1.16210064126571,-6.78528611865612));
#12684=CARTESIAN_POINT('Ctrl Pts',(3.73475239962943,-1.16146206906641,-6.78502371378005));
#12685=CARTESIAN_POINT('Ctrl Pts',(3.74477504862178,-1.15974327189991,-6.78434047062667));
#12686=CARTESIAN_POINT('Ctrl Pts',(3.75095475131992,-1.15863256907437,-6.78392125720717));
#12687=CARTESIAN_POINT('Ctrl Pts',(3.79708553285239,-1.14995991974874,-6.78080526553379));
#12688=CARTESIAN_POINT('Ctrl Pts',(3.83663459613673,-1.14038214217488,-6.77820869735128));
#12689=CARTESIAN_POINT('Ctrl Pts',(3.94425947164555,-1.10833675414791,-6.7711557365467));
#12690=CARTESIAN_POINT('Ctrl Pts',(4.01089912620436,-1.08167765371538,-6.76679557453375));
#12691=CARTESIAN_POINT('Ctrl Pts',(4.07586091965954,-1.0485390526759,-6.76222984462527));
#12692=CARTESIAN_POINT('Ctrl Pts',(4.07701560047057,-1.04794761518503,-6.76214858706782));
#12693=CARTESIAN_POINT('Ctrl Pts',(4.0781692678987,-1.04735428853534,-6.76206729648848));
#12694=CARTESIAN_POINT('Ctrl Pts',(4.07816925191529,-1.04735429675555,-6.66223230003384));
#12695=CARTESIAN_POINT('Ctrl Pts',(4.03969408049091,-1.06714192631356,-6.66495692610531));
#12696=CARTESIAN_POINT('Ctrl Pts',(4.00015451341866,-1.0847961500492,-6.66772673241389));
#12697=CARTESIAN_POINT('Ctrl Pts',(3.94961087810461,-1.10410010970873,-6.67128271102149));
#12698=CARTESIAN_POINT('Ctrl Pts',(3.93944078089483,-1.10782442476969,-6.67199887128965));
#12699=CARTESIAN_POINT('Ctrl Pts',(3.92334981969789,-1.11346652953801,-6.67313367573815));
#12700=CARTESIAN_POINT('Ctrl Pts',(3.91746247746872,-1.11547861265525,-6.67354923123327));
#12701=CARTESIAN_POINT('Ctrl Pts',(3.90641021242486,-1.11915834125073,-6.67433014449681));
#12702=CARTESIAN_POINT('Ctrl Pts',(3.9012491479838,-1.12083712125192,-6.67469512841656));
#12703=CARTESIAN_POINT('Ctrl Pts',(3.8896683945488,-1.12451576686303,-6.67551491441929));
#12704=CARTESIAN_POINT('Ctrl Pts',(3.88324285425023,-1.12649643432913,-6.6759703241808));
#12705=CARTESIAN_POINT('Ctrl Pts',(3.86684900013226,-1.13139650577913,-6.67713381126026));
#12706=CARTESIAN_POINT('Ctrl Pts',(3.85685855264548,-1.13423920652473,-6.67784431832386));
#12707=CARTESIAN_POINT('Ctrl Pts',(3.77397218326361,-1.15664307375816,-6.68375271513853));
#12708=CARTESIAN_POINT('Ctrl Pts',(3.69940161201151,-1.16928403529077,-6.68917232137838));
#12709=CARTESIAN_POINT('Ctrl Pts',(3.56647119885207,-1.17886067955666,-6.69892168937668));
#12710=CARTESIAN_POINT('Ctrl Pts',(3.50856621911921,-1.17876252662703,-6.70319260695171));
#12711=CARTESIAN_POINT('Ctrl Pts',(3.430476630254,-1.17287014583568,-6.70884754199157));
#12712=CARTESIAN_POINT('Ctrl Pts',(3.41009381814368,-1.17079624066649,-6.71031328272101));
#12713=CARTESIAN_POINT('Ctrl Pts',(3.3768353038047,-1.16653299596295,-6.7126780057569));
#12714=CARTESIAN_POINT('Ctrl Pts',(3.36392403236121,-1.16465945968854,-6.71358930928048));
#12715=CARTESIAN_POINT('Ctrl Pts',(3.34640590602214,-1.1618194659259,-6.71481430947922));
#12716=CARTESIAN_POINT('Ctrl Pts',(3.34177035121634,-1.16103945315861,-6.71513736493399));
#12717=CARTESIAN_POINT('Ctrl Pts',(3.33401534805295,-1.15968674565955,-6.7156758392496));
#12718=CARTESIAN_POINT('Ctrl Pts',(3.330893357844,-1.15912917352665,-6.71589207864268));
#12719=CARTESIAN_POINT('Ctrl Pts',(3.32496359592468,-1.15804541331727,-6.71630172199128));
#12720=CARTESIAN_POINT('Ctrl Pts',(3.32215543508724,-1.15752161169072,-6.71649526149435));
#12721=CARTESIAN_POINT('Ctrl Pts',(3.31548077415606,-1.15625145174104,-6.71695425751133));
#12722=CARTESIAN_POINT('Ctrl Pts',(3.31161602595741,-1.155495902818,-6.7172192056744));
#12723=CARTESIAN_POINT('Ctrl Pts',(3.29793503437833,-1.15274999179229,-6.7181544379576));
#12724=CARTESIAN_POINT('Ctrl Pts',(3.28814013888731,-1.15065374441439,-6.71881913911782));
#12725=CARTESIAN_POINT('Ctrl Pts',(3.21947976052878,-1.13504081276552,-6.72345183954457));
#12726=CARTESIAN_POINT('Ctrl Pts',(3.16169609695336,-1.1171367409232,-6.72721468055645));
#12727=CARTESIAN_POINT('Ctrl Pts',(3.0558610259697,-1.07518610689265,-6.7342672712723));
#12728=CARTESIAN_POINT('Ctrl Pts',(3.00758619799352,-1.05213946569287,-6.73755358868724));
#12729=CARTESIAN_POINT('Ctrl Pts',(2.92123351878949,-1.00344747065451,-6.74378862857377));
#12730=CARTESIAN_POINT('Ctrl Pts',(2.88276793149337,-0.978703761563427,
-6.7467114903992));
#12731=CARTESIAN_POINT('Ctrl Pts',(2.83741459217629,-0.945649557057543,
-6.75040308936541));
#12732=CARTESIAN_POINT('Ctrl Pts',(2.82907137834889,-0.939397598930528,
-6.7510929208828));
#12733=CARTESIAN_POINT('Ctrl Pts',(2.81595303325433,-0.92929269168857,-6.75219538589434));
#12734=CARTESIAN_POINT('Ctrl Pts',(2.81112298626219,-0.925511674339759,
-6.75260522442358));
#12735=CARTESIAN_POINT('Ctrl Pts',(2.80206687151045,-0.918307639487769,
-6.75338122221944));
#12736=CARTESIAN_POINT('Ctrl Pts',(2.79783453391576,-0.914892733165022,
-6.75374705493866));
#12737=CARTESIAN_POINT('Ctrl Pts',(2.78832200767073,-0.907108063804068,
-6.75457659830966));
#12738=CARTESIAN_POINT('Ctrl Pts',(2.7830560466221,-0.902721306331306,-6.75504098096405));
#12739=CARTESIAN_POINT('Ctrl Pts',(2.76723079188693,-0.889302524766589,
-6.75645249151779));
#12740=CARTESIAN_POINT('Ctrl Pts',(2.75679308935315,-0.880129635948533,
-6.75740529730052));
#12741=CARTESIAN_POINT('Ctrl Pts',(2.67239925143129,-0.803273702268906,
-6.76529445937801));
#12742=CARTESIAN_POINT('Ctrl Pts',(2.60721341766611,-0.72659719171487,-6.77263362982777));
#12743=CARTESIAN_POINT('Ctrl Pts',(2.54760172196587,-0.63504080914287,-6.7806444360294));
#12744=CARTESIAN_POINT('Ctrl Pts',(2.54275563879319,-0.627406980593619,
-6.78130681115992));
#12745=CARTESIAN_POINT('Ctrl Pts',(2.51416970121923,-0.581209487116651,
-6.78527972789266));
#12746=CARTESIAN_POINT('Ctrl Pts',(2.49257972503752,-0.541354463291943,
-6.78856125460678));
#12747=CARTESIAN_POINT('Ctrl Pts',(2.46923364269699,-0.491607065996209,
-6.79240971705387));
#12748=CARTESIAN_POINT('Ctrl Pts',(2.46523764919929,-0.482812434938268,
-6.79308098821138));
#12749=CARTESIAN_POINT('Ctrl Pts',(2.45966922551096,-0.470145577907281,
-6.79403387539043));
#12750=CARTESIAN_POINT('Ctrl Pts',(2.45800862003142,-0.466312876813195,
-6.79432038729489));
#12751=CARTESIAN_POINT('Ctrl Pts',(2.45516024036512,-0.459641708385756,
-6.79481585096563));
#12752=CARTESIAN_POINT('Ctrl Pts',(2.45396314725701,-0.456807301865322,
-6.79502534908458));
#12753=CARTESIAN_POINT('Ctrl Pts',(2.45145430405074,-0.45080145079258,-6.79546708942839));
#12754=CARTESIAN_POINT('Ctrl Pts',(2.45014529747735,-0.447628939508743,
-6.79569917014659));
#12755=CARTESIAN_POINT('Ctrl Pts',(2.4466266519131,-0.438994287205734,-6.79632752076504));
#12756=CARTESIAN_POINT('Ctrl Pts',(2.44444406783868,-0.433521124072911,
-6.79672222760861));
#12757=CARTESIAN_POINT('Ctrl Pts',(2.4343161268973,-0.407559158618024,-6.79857869023566));
#12758=CARTESIAN_POINT('Ctrl Pts',(2.42690358519853,-0.386865538044714,
-6.80001203097592));
#12759=CARTESIAN_POINT('Ctrl Pts',(2.41324450231184,-0.345085114794105,
-6.80283692026412));
#12760=CARTESIAN_POINT('Ctrl Pts',(2.40700078244525,-0.324007038712493,
-6.80422790288981));
#12761=CARTESIAN_POINT('Ctrl Pts',(2.38504935955152,-0.241486362180716,
-6.80958467523989));
#12762=CARTESIAN_POINT('Ctrl Pts',(2.37372360218986,-0.178989729123073,
-6.81345784811891));
#12763=CARTESIAN_POINT('Ctrl Pts',(2.36369347475816,-0.0775462282988194,
-6.81981413563133));
#12764=CARTESIAN_POINT('Ctrl Pts',(2.36178645437343,-0.0390484374729072,
-6.82224090627389));
#12765=CARTESIAN_POINT('Ctrl Pts',(2.3617584524301,0.0233528855997684,-6.82625508664994));
#12766=CARTESIAN_POINT('Ctrl Pts',(2.3624741030455,0.0472276289898454,-6.82780978548872));
#12767=CARTESIAN_POINT('Ctrl Pts',(2.36444120900201,0.0797697700894638,
-6.82996265995066));
#12768=CARTESIAN_POINT('Ctrl Pts',(2.36506422404484,0.088470354637313,-6.83054154617317));
#12769=CARTESIAN_POINT('Ctrl Pts',(2.36621188892993,0.10233421586873,-6.83146955726326));
#12770=CARTESIAN_POINT('Ctrl Pts',(2.36667412925588,0.107502448255194,-6.83181674632096));
#12771=CARTESIAN_POINT('Ctrl Pts',(2.36769610319958,0.11813648966522,-6.83253375246205));
#12772=CARTESIAN_POINT('Ctrl Pts',(2.36825996220806,0.123601765149962,-6.83290368905072));
#12773=CARTESIAN_POINT('Ctrl Pts',(2.36966153568733,0.136314658528128,-6.83376765044031));
#12774=CARTESIAN_POINT('Ctrl Pts',(2.37052838903993,0.143558769729832,-6.83426256783966));
#12775=CARTESIAN_POINT('Ctrl Pts',(2.37354584110022,0.166932044275687,-6.83586813280142));
#12776=CARTESIAN_POINT('Ctrl Pts',(2.3759633270335,0.183024219701473,-6.83698699192357));
#12777=CARTESIAN_POINT('Ctrl Pts',(2.38246764859101,0.220953666794613,-6.83965737353814));
#12778=CARTESIAN_POINT('Ctrl Pts',(2.38684038647574,0.242734952476235,-6.84121719054443));
#12779=CARTESIAN_POINT('Ctrl Pts',(2.41664227400825,0.37210790352346,-6.85064031129608));
#12780=CARTESIAN_POINT('Ctrl Pts',(2.45649638177561,0.475786202878335,-6.85892347298615));
#12781=CARTESIAN_POINT('Ctrl Pts',(2.52185312925952,0.593316987607398,-6.86857015164366));
#12782=CARTESIAN_POINT('Ctrl Pts',(2.53413294163859,0.613895704616208,-6.87026668762828));
#12783=CARTESIAN_POINT('Ctrl Pts',(2.5502586990682,0.639136071292022,-6.87234428553934));
#12784=CARTESIAN_POINT('Ctrl Pts',(2.55352301263909,0.64416052165229,-6.87275768961468));
#12785=CARTESIAN_POINT('Ctrl Pts',(2.5587482993456,0.65207052099037,-6.87340797241401));
#12786=CARTESIAN_POINT('Ctrl Pts',(2.56068393865322,0.654972560705993,-6.87364643346443));
#12787=CARTESIAN_POINT('Ctrl Pts',(2.56417156785656,0.660151454470522,-6.87407171460712));
#12788=CARTESIAN_POINT('Ctrl Pts',(2.56571864891025,0.662431455184437,-6.87425884400697));
#12789=CARTESIAN_POINT('Ctrl Pts',(2.56947155445387,0.667920715522432,-6.87470915837135));
#12790=CARTESIAN_POINT('Ctrl Pts',(2.57168531122946,0.671124489960972,-6.87497181124606));
#12791=CARTESIAN_POINT('Ctrl Pts',(2.57856179719177,0.680971431693616,-6.87577875659032));
#12792=CARTESIAN_POINT('Ctrl Pts',(2.58327745414761,0.687577596972359,-6.87631965809008));
#12793=CARTESIAN_POINT('Ctrl Pts',(2.594474469119,0.702925465070551,-6.8775765737132));
#12794=CARTESIAN_POINT('Ctrl Pts',(2.6010095271337,0.711627264318275,-6.87828940948526));
#12795=CARTESIAN_POINT('Ctrl Pts',(2.6246683207623,0.74223737859779,-6.88080259418332));
#12796=CARTESIAN_POINT('Ctrl Pts',(2.64244709400461,0.763629688795714,-6.88256956757008));
#12797=CARTESIAN_POINT('Ctrl Pts',(2.71624717849137,0.846290733441035,-6.88953014948902));
#12798=CARTESIAN_POINT('Ctrl Pts',(2.77791685332837,0.902190278146503,-6.89456020945228));
#12799=CARTESIAN_POINT('Ctrl Pts',(2.8779799133711,0.975260739708032,-6.90238144938915));
#12800=CARTESIAN_POINT('Ctrl Pts',(2.91223774222761,0.99763978986436,-6.90500497567985));
#12801=CARTESIAN_POINT('Ctrl Pts',(2.95665397386629,1.02346145575756,-6.90838408444585));
#12802=CARTESIAN_POINT('Ctrl Pts',(2.96579034400363,1.02861091220321,-6.90907794112124));
#12803=CARTESIAN_POINT('Ctrl Pts',(2.98038922446982,1.0365841455794,-6.91018535130848));
#12804=CARTESIAN_POINT('Ctrl Pts',(2.98580732021764,1.03948841770918,-6.9105960657593));
#12805=CARTESIAN_POINT('Ctrl Pts',(2.99557789382863,1.0446276933287,-6.91133633763614));
#12806=CARTESIAN_POINT('Ctrl Pts',(2.999922062018,1.0468782586212,-6.91166534227625));
#12807=CARTESIAN_POINT('Ctrl Pts',(3.01013540744032,1.05208898392355,-6.91243860675864));
#12808=CARTESIAN_POINT('Ctrl Pts',(3.01601554545276,1.05502717917947,-6.91288361435874));
#12809=CARTESIAN_POINT('Ctrl Pts',(3.03314434600629,1.06340766834748,-6.91417956492516));
#12810=CARTESIAN_POINT('Ctrl Pts',(3.04445512022817,1.06872021340993,-6.91503489968446));
#12811=CARTESIAN_POINT('Ctrl Pts',(3.07026111078137,1.08034343267464,-6.91698610640284));
#12812=CARTESIAN_POINT('Ctrl Pts',(3.0848029204116,1.08654412999859,-6.91808544202488));
#12813=CARTESIAN_POINT('Ctrl Pts',(3.13347979615136,1.106151872226,-6.92176556801476));
#12814=CARTESIAN_POINT('Ctrl Pts',(3.16811338083593,1.11825633481821,-6.92438515878998));
#12815=CARTESIAN_POINT('Ctrl Pts',(3.27713711834445,1.15073639310091,-6.9326184293187));
#12816=CARTESIAN_POINT('Ctrl Pts',(3.35300009215083,1.16543915224477,-6.93834205555534));
#12817=CARTESIAN_POINT('Ctrl Pts',(3.46160203977756,1.17560504884084,-6.94623244178478));
#12818=CARTESIAN_POINT('Ctrl Pts',(3.49356229339287,1.17728784614667,-6.94851554194323));
#12819=CARTESIAN_POINT('Ctrl Pts',(3.53205527235309,1.17774429433506,-6.95119004652786));
#12820=CARTESIAN_POINT('Ctrl Pts',(3.53855693738647,1.17776755344958,-6.95163919166778));
#12821=CARTESIAN_POINT('Ctrl Pts',(3.54866271551492,1.17772002000042,-6.95233294898447));
#12822=CARTESIAN_POINT('Ctrl Pts',(3.55226675154519,1.17768652412811,-6.95257950139132));
#12823=CARTESIAN_POINT('Ctrl Pts',(3.55891582329761,1.17759420117772,-6.95303270350876));
#12824=CARTESIAN_POINT('Ctrl Pts',(3.56196078344325,1.17754010820978,-6.95323959798634));
#12825=CARTESIAN_POINT('Ctrl Pts',(3.56890033084387,1.17738990092643,-6.95370965989493));
#12826=CARTESIAN_POINT('Ctrl Pts',(3.57279467737905,1.17728627452348,-6.95397241289479));
#12827=CARTESIAN_POINT('Ctrl Pts',(3.58480836779236,1.17690693688837,-6.95477997857616));
#12828=CARTESIAN_POINT('Ctrl Pts',(3.59292563546801,1.17656653277554,-6.95532139276072));
#12829=CARTESIAN_POINT('Ctrl Pts',(3.61191920870908,1.17557304421458,-6.95657969502754));
#12830=CARTESIAN_POINT('Ctrl Pts',(3.62279142004709,1.17485296792975,-6.95729339513135));
#12831=CARTESIAN_POINT('Ctrl Pts',(3.66142100468109,1.17175553079635,-6.95981077564493));
#12832=CARTESIAN_POINT('Ctrl Pts',(3.68910375097065,1.16854428311075,-6.96158096037175));
#12833=CARTESIAN_POINT('Ctrl Pts',(3.79898141687525,1.151828962299,-6.96856178832686));
#12834=CARTESIAN_POINT('Ctrl Pts',(3.87975351181944,1.13060683134617,-6.97360820901913));
#12835=CARTESIAN_POINT('Ctrl Pts',(3.99554955308146,1.0866360613769,-6.98142920784409));
#12836=CARTESIAN_POINT('Ctrl Pts',(4.03271244296891,1.07028103207164,-6.9840330768067));
#12837=CARTESIAN_POINT('Ctrl Pts',(4.07830420868544,1.04733717994058,-6.98739015706453));
#12838=CARTESIAN_POINT('Ctrl Pts',(4.08759038698651,1.04250775236297,-6.98808266737241));
#12839=CARTESIAN_POINT('Ctrl Pts',(4.10222241145279,1.03464859994552,-6.98918842348921));
#12840=CARTESIAN_POINT('Ctrl Pts',(4.10761118408278,1.03169962835317,-6.98959884501701));
#12841=CARTESIAN_POINT('Ctrl Pts',(4.11725047536827,1.026326169348,-6.99033886629625));
#12842=CARTESIAN_POINT('Ctrl Pts',(4.1215094498028,1.02391707625673,-6.99066791565676));
#12843=CARTESIAN_POINT('Ctrl Pts',(4.13145976732477,1.01820653131191,-6.99144164850299));
#12844=CARTESIAN_POINT('Ctrl Pts',(4.13713865422664,1.01488381544195,-6.99188708269975));
#12845=CARTESIAN_POINT('Ctrl Pts',(4.15354724550633,1.00509767556964,-6.99318552368948));
#12846=CARTESIAN_POINT('Ctrl Pts',(4.16420176897901,0.998510611830281,-6.99404294828922));
#12847=CARTESIAN_POINT('Ctrl Pts',(4.1881008433109,0.983202997381192,-6.99599966527891));
#12848=CARTESIAN_POINT('Ctrl Pts',(4.20127817750515,0.974382518504581,-6.99710244965141));
#12849=CARTESIAN_POINT('Ctrl Pts',(4.24446813913542,0.944192296356771,-7.00079823258044));
#12850=CARTESIAN_POINT('Ctrl Pts',(4.27365368339299,0.921682269978761,-7.0034303986974));
#12851=CARTESIAN_POINT('Ctrl Pts',(4.3666215747848,0.842758117476609,-7.0122580986104));
#12852=CARTESIAN_POINT('Ctrl Pts',(4.4253428181045,0.78080430182532,-7.01859655327805));
#12853=CARTESIAN_POINT('Ctrl Pts',(4.49173489557294,0.69352905887114,-7.02646820873037));
#12854=CARTESIAN_POINT('Ctrl Pts',(4.50598314550552,0.673531681459298,-7.02820756241506));
#12855=CARTESIAN_POINT('Ctrl Pts',(4.52294516082613,0.648077620395582,-7.03032959292079));
#12856=CARTESIAN_POINT('Ctrl Pts',(4.52625468912475,0.643027448770807,-7.03074623642977));
#12857=CARTESIAN_POINT('Ctrl Pts',(4.53142055666271,0.635010792467661,-7.03140046871349));
#12858=CARTESIAN_POINT('Ctrl Pts',(4.53330270842835,0.632061188902619,-7.03163967101463));
#12859=CARTESIAN_POINT('Ctrl Pts',(4.53664249492721,0.626775462534022,-7.03206556867885));
#12860=CARTESIAN_POINT('Ctrl Pts',(4.53810507870295,0.624442622155051,-7.03225257927809));
#12861=CARTESIAN_POINT('Ctrl Pts',(4.54160793173517,0.618811744674869,-7.03270170007058));
#12862=CARTESIAN_POINT('Ctrl Pts',(4.54364010875641,0.615508734854622,-7.03296328610699));
#12863=CARTESIAN_POINT('Ctrl Pts',(4.54983152899528,0.605333203400713,-7.03376363905737));
#12864=CARTESIAN_POINT('Ctrl Pts',(4.55393691031919,0.598427945324766,-7.03429909447342));
#12865=CARTESIAN_POINT('Ctrl Pts',(4.56336416527044,0.58219545329873,-7.03554129993238));
#12866=CARTESIAN_POINT('Ctrl Pts',(4.56862984534281,0.572836237231097,-7.03624497275124));
#12867=CARTESIAN_POINT('Ctrl Pts',(4.58680310738221,0.53947546330884,-7.03871387024338));
#12868=CARTESIAN_POINT('Ctrl Pts',(4.59900565958248,0.515098048178396,-7.04044697458996));
#12869=CARTESIAN_POINT('Ctrl Pts',(4.64375868190631,0.417359329041283,-7.04720422796433));
#12870=CARTESIAN_POINT('Ctrl Pts',(4.66962187985426,0.341177737989694,-7.0520714402714));
#12871=CARTESIAN_POINT('Ctrl Pts',(4.69738058053782,0.219988313203584,-7.05989752168927));
#12872=CARTESIAN_POINT('Ctrl Pts',(4.70480147631856,0.176506033451226,-7.06271819697244));
#12873=CARTESIAN_POINT('Ctrl Pts',(4.71095973806301,0.122203362351113,-7.0663110198783));
#12874=CARTESIAN_POINT('Ctrl Pts',(4.7120099783872,0.11167792246834,-7.06701054922194));
#12875=CARTESIAN_POINT('Ctrl Pts',(4.71345306976491,0.0949355685228497,
-7.06812888491756));
#12876=CARTESIAN_POINT('Ctrl Pts',(4.71393863073535,0.0887270579131143,
-7.06854481798648));
#12877=CARTESIAN_POINT('Ctrl Pts',(4.71475512596359,0.0771017389255085,
-7.06932606683925));
#12878=CARTESIAN_POINT('Ctrl Pts',(4.71509790381717,0.0716859062987276,
-7.0696910056985));
#12879=CARTESIAN_POINT('Ctrl Pts',(4.71578111806654,0.0595626924295782,
-7.0705102004321));
#12880=CARTESIAN_POINT('Ctrl Pts',(4.71610163264545,0.0528544235359496,
-7.0709650600379));
#12881=CARTESIAN_POINT('Ctrl Pts',(4.71688184619523,0.0329559973079337,
-7.07231912300433));
#12882=CARTESIAN_POINT('Ctrl Pts',(4.71717720794089,0.0197608227562213,
-7.0732233445949));
#12883=CARTESIAN_POINT('Ctrl Pts',(4.71772531631624,-0.0785835143482757,
-7.08001209986993));
#12884=CARTESIAN_POINT('Ctrl Pts',(4.70896457929958,-0.16351529553302,-7.08617926684367));
#12885=CARTESIAN_POINT('Ctrl Pts',(4.67647328173662,-0.315159851093711,
-7.09755692516775));
#12886=CARTESIAN_POINT('Ctrl Pts',(4.65574570538109,-0.382139350420601,
-7.10271206375049));
#12887=CARTESIAN_POINT('Ctrl Pts',(4.62546688419015,-0.455970112022877,
-7.10830532817737));
#12888=CARTESIAN_POINT('Ctrl Pts',(4.62162824007426,-0.465006621511712,
-7.10898814851061));
#12889=CARTESIAN_POINT('Ctrl Pts',(4.6161054547918,-0.477568866689485,-7.10993387306767));
#12890=CARTESIAN_POINT('Ctrl Pts',(4.61451621964331,-0.481135527432326,
-7.11020198279427));
#12891=CARTESIAN_POINT('Ctrl Pts',(4.61173710184475,-0.487290082821082,
-7.11066385324795));
#12892=CARTESIAN_POINT('Ctrl Pts',(4.61055552751744,-0.489881658958593,
-7.11085810016822));
#12893=CARTESIAN_POINT('Ctrl Pts',(4.60803437035533,-0.495358651147113,
-7.11126807298457));
#12894=CARTESIAN_POINT('Ctrl Pts',(4.6066924752041,-0.4982429769944,-7.11148365144671));
#12895=CARTESIAN_POINT('Ctrl Pts',(4.60331869858652,-0.505418553060139,
-7.11201924163671));
#12896=CARTESIAN_POINT('Ctrl Pts',(4.60127249679907,-0.509703076545849,
-7.11233839510334));
#12897=CARTESIAN_POINT('Ctrl Pts',(4.59335598893426,-0.526024828496433,
-7.11355216653634));
#12898=CARTESIAN_POINT('Ctrl Pts',(4.58730617461557,-0.537974528177732,
-7.11443656459233));
#12899=CARTESIAN_POINT('Ctrl Pts',(4.57113500721997,-0.568607931362771,
-7.11669939343489));
#12900=CARTESIAN_POINT('Ctrl Pts',(4.56070926585022,-0.587126149222905,
-7.11806305040252));
#12901=CARTESIAN_POINT('Ctrl Pts',(4.52564812402616,-0.645639374330876,
-7.12239065165006));
#12902=CARTESIAN_POINT('Ctrl Pts',(4.49911919740118,-0.684447799843941,
-7.12529115394666));
#12903=CARTESIAN_POINT('Ctrl Pts',(4.42208324700518,-0.78382395189669,-7.13306862470912));
#12904=CARTESIAN_POINT('Ctrl Pts',(4.36770706680266,-0.841072046630359,
-7.13794684798209));
#12905=CARTESIAN_POINT('Ctrl Pts',(4.29629525084763,-0.902565557050582,
-7.1440881164435));
#12906=CARTESIAN_POINT('Ctrl Pts',(4.28436468504494,-0.912436160314251,
-7.14510563663329));
#12907=CARTESIAN_POINT('Ctrl Pts',(4.2667028192457,-0.926471215205673,-7.14660186467681));
#12908=CARTESIAN_POINT('Ctrl Pts',(4.26112273061399,-0.930823974402834,
-7.1470731528378));
#12909=CARTESIAN_POINT('Ctrl Pts',(4.25115276647287,-0.938457536113191,
-7.14791288009413));
#12910=CARTESIAN_POINT('Ctrl Pts',(4.24677854591947,-0.941758513211628,
-7.14828052128374));
#12911=CARTESIAN_POINT('Ctrl Pts',(4.23760693701277,-0.948579871057561,
-7.14904984236514));
#12912=CARTESIAN_POINT('Ctrl Pts',(4.23280559823294,-0.952094653679381,
-7.14945172326379));
#12913=CARTESIAN_POINT('Ctrl Pts',(4.22020251971272,-0.96117475787509,-7.15050452211094));
#12914=CARTESIAN_POINT('Ctrl Pts',(4.21235925589059,-0.966681410308054,
-7.15115763514999));
#12915=CARTESIAN_POINT('Ctrl Pts',(4.17613138693082,-0.991462023976714,
-7.15416566124351));
#12916=CARTESIAN_POINT('Ctrl Pts',(4.14698278190948,-1.00958388109635,-7.15656247583159));
#12917=CARTESIAN_POINT('Ctrl Pts',(4.10424251179752,-1.03363422219343,-7.16004652232032));
#12918=CARTESIAN_POINT('Ctrl Pts',(4.09126744113973,-1.04061795015813,-7.16110026873543));
#12919=CARTESIAN_POINT('Ctrl Pts',(4.0781692089456,-1.04735431885469,-7.16215973101906));
#12920=CARTESIAN_POINT('Origin',(3.53951905042299,8.32667268468867E-16,
0.924367114736157));
#12921=CARTESIAN_POINT('',(4.07816960641416,-1.04735411443809,-7.76226461992607));
#12922=CARTESIAN_POINT('',(4.07816926754758,-1.04735428871592,-7.66392024962001));
#12923=CARTESIAN_POINT('',(4.07816926754759,-1.04735428871592,0.924367114736157));
#12924=CARTESIAN_POINT('Ctrl Pts',(4.07816960641408,-1.04735411443813,-7.76226461992608));
#12925=CARTESIAN_POINT('Ctrl Pts',(4.14556688893452,-1.01269192788493,-7.75682161009484));
#12926=CARTESIAN_POINT('Ctrl Pts',(4.20950448577251,-0.971582581204844,
-7.75120889432629));
#12927=CARTESIAN_POINT('Ctrl Pts',(4.29235791872549,-0.906205453315994,
-7.7435124974742));
#12928=CARTESIAN_POINT('Ctrl Pts',(4.31494024023408,-0.886959356333163,
-7.74136708228466));
#12929=CARTESIAN_POINT('Ctrl Pts',(4.34512879996207,-0.859195473604848,
-7.73845527776039));
#12930=CARTESIAN_POINT('Ctrl Pts',(4.35337322174209,-0.85139023921627,-7.73765531120893));
#12931=CARTESIAN_POINT('Ctrl Pts',(4.36750977062185,-0.83761372868248,-7.73627714661413));
#12932=CARTESIAN_POINT('Ctrl Pts',(4.37345324343183,-0.831696557019306,
-7.73569566060694));
#12933=CARTESIAN_POINT('Ctrl Pts',(4.38209990431143,-0.822902266345793,
-7.73484732040817));
#12934=CARTESIAN_POINT('Ctrl Pts',(4.38485248793398,-0.820074396539185,
-7.73457689649046));
#12935=CARTESIAN_POINT('Ctrl Pts',(4.38970713354745,-0.815036555907846,
-7.7340993984581));
#12936=CARTESIAN_POINT('Ctrl Pts',(4.39181488219016,-0.812832196743304,
-7.73389189753237));
#12937=CARTESIAN_POINT('Ctrl Pts',(4.3963701542494,-0.808030928655589,-7.73344305606354));
#12938=CARTESIAN_POINT('Ctrl Pts',(4.39881445139993,-0.805431071227729,
-7.73320195612856));
#12939=CARTESIAN_POINT('Ctrl Pts',(4.40556957504016,-0.798180283170265,
-7.7325347899299));
#12940=CARTESIAN_POINT('Ctrl Pts',(4.40985478988405,-0.793505501344605,
-7.73211058469992));
#12941=CARTESIAN_POINT('Ctrl Pts',(4.43356395906844,-0.767217800467252,
-7.72975649443369));
#12942=CARTESIAN_POINT('Ctrl Pts',(4.45222236381671,-0.744924445941719,
-7.72787705318411));
#12943=CARTESIAN_POINT('Ctrl Pts',(4.53468386509084,-0.638641745695555,
-7.71931978289575));
#12944=CARTESIAN_POINT('Ctrl Pts',(4.58784769191558,-0.547015653763979,
-7.71301198460183));
#12945=CARTESIAN_POINT('Ctrl Pts',(4.63643928222183,-0.429345949587526,
-7.70490609887472));
#12946=CARTESIAN_POINT('Ctrl Pts',(4.64421094666931,-0.408934795361378,
-7.70350188756853));
#12947=CARTESIAN_POINT('Ctrl Pts',(4.65670621506438,-0.373156647211704,
-7.70103459210921));
#12948=CARTESIAN_POINT('Ctrl Pts',(4.66169104429829,-0.35788688164406,-7.69997978330874));
#12949=CARTESIAN_POINT('Ctrl Pts',(4.66847301687645,-0.33557517637653,-7.69843363712351));
#12950=CARTESIAN_POINT('Ctrl Pts',(4.67051986224482,-0.328610585780765,
-7.69795032981678));
#12951=CARTESIAN_POINT('Ctrl Pts',(4.67400126517393,-0.316346805770901,
-7.69709788943068));
#12952=CARTESIAN_POINT('Ctrl Pts',(4.67546341213067,-0.311055626011664,
-7.69672965287915));
#12953=CARTESIAN_POINT('Ctrl Pts',(4.67842674805309,-0.300032377602288,
-7.69596146357307));
#12954=CARTESIAN_POINT('Ctrl Pts',(4.67992177291725,-0.294298827124975,
-7.69556132559128));
#12955=CARTESIAN_POINT('Ctrl Pts',(4.68369246471328,-0.27937761272359,-7.69451836812927));
#12956=CARTESIAN_POINT('Ctrl Pts',(4.68590071255792,-0.270173514823771,
-7.69387342952474));
#12957=CARTESIAN_POINT('Ctrl Pts',(4.69459483236595,-0.231908560928371,
-7.69118494549031));
#12958=CARTESIAN_POINT('Ctrl Pts',(4.70008791690094,-0.202635820551755,
-7.68911065875982));
#12959=CARTESIAN_POINT('Ctrl Pts',(4.72096561249892,-0.0622027350810218,
-7.67906958150976));
#12960=CARTESIAN_POINT('Ctrl Pts',(4.72151870365948,0.0505470770343604,
-7.67066829831299));
#12961=CARTESIAN_POINT('Ctrl Pts',(4.70251539861179,0.187682554051796,-7.66071514207197));
#12962=CARTESIAN_POINT('Ctrl Pts',(4.69803931440612,0.213579701841117,-7.65885146117777));
#12963=CARTESIAN_POINT('Ctrl Pts',(4.69148657916122,0.245156184020468,-7.65661514843368));
#12964=CARTESIAN_POINT('Ctrl Pts',(4.69022836973812,0.250995633504863,-7.65620312203101));
#12965=CARTESIAN_POINT('Ctrl Pts',(4.68817342071676,0.260192434492154,-7.65555689540233));
#12966=CARTESIAN_POINT('Ctrl Pts',(4.68740628344853,0.263556192095195,-7.65532110619441));
#12967=CARTESIAN_POINT('Ctrl Pts',(4.68592805367901,0.269909057829779,-7.65487693049772));
#12968=CARTESIAN_POINT('Ctrl Pts',(4.68522005173237,0.272898732269683,-7.65466838725027));
#12969=CARTESIAN_POINT('Ctrl Pts',(4.68354671871649,0.279843401665547,-7.65418504824056));
#12970=CARTESIAN_POINT('Ctrl Pts',(4.6825725709175,0.283796204686188,-7.65391075220427));
#12971=CARTESIAN_POINT('Ctrl Pts',(4.67930457805331,0.296766904017365,-7.65301311455201));
#12972=CARTESIAN_POINT('Ctrl Pts',(4.67692428956788,0.305762946693021,-7.65239442003223));
#12973=CARTESIAN_POINT('Ctrl Pts',(4.65250890940407,0.393804922296951,-7.64636902511804));
#12974=CARTESIAN_POINT('Ctrl Pts',(4.62237270312612,0.470383641490296,-7.64135285622537));
#12975=CARTESIAN_POINT('Ctrl Pts',(4.55015983196625,0.609301078279215,-7.63166113997555));
#12976=CARTESIAN_POINT('Ctrl Pts',(4.50962003393686,0.671970707722357,-7.62701651962438));
#12977=CARTESIAN_POINT('Ctrl Pts',(4.45539595190987,0.740562445376185,-7.62129362756211));
#12978=CARTESIAN_POINT('Ctrl Pts',(4.44718649577451,0.750601772713224,-7.62043872537782));
#12979=CARTESIAN_POINT('Ctrl Pts',(4.4345060383587,0.765596399152738,-7.61913414032792));
#12980=CARTESIAN_POINT('Ctrl Pts',(4.43015576195676,0.77065284010654,-7.61868930563029));
#12981=CARTESIAN_POINT('Ctrl Pts',(4.42219024726662,0.779753836696831,-7.61787953296758));
#12982=CARTESIAN_POINT('Ctrl Pts',(4.41858954630701,0.783810914165555,-7.61751519731575));
#12983=CARTESIAN_POINT('Ctrl Pts',(4.41077109874536,0.792498682785925,-7.61672765773584));
#12984=CARTESIAN_POINT('Ctrl Pts',(4.40654419752674,0.797120872638972,-7.61630407910134));
#12985=CARTESIAN_POINT('Ctrl Pts',(4.39497423766218,0.809571920341705,-7.61515039278713));
#12986=CARTESIAN_POINT('Ctrl Pts',(4.38756084819705,0.817334305891291,-7.61441733018609));
#12987=CARTESIAN_POINT('Ctrl Pts',(4.34734595271497,0.858306196982865,-7.61047206654441));
#12988=CARTESIAN_POINT('Ctrl Pts',(4.3127021477042,0.889640785273998,-7.6071801280333));
#12989=CARTESIAN_POINT('Ctrl Pts',(4.21524262469063,0.967789587261133,-7.59819413757494));
#12990=CARTESIAN_POINT('Ctrl Pts',(4.1494648353104,1.0105363052994,-7.59239258528162));
#12991=CARTESIAN_POINT('Ctrl Pts',(4.04493593915915,1.06451921182557,-7.58383579205721));
#12992=CARTESIAN_POINT('Ctrl Pts',(4.00903992169192,1.08083219033206,-7.58100676178135));
#12993=CARTESIAN_POINT('Ctrl Pts',(3.96623188831529,1.09774999937062,-7.577808417719));
#12994=CARTESIAN_POINT('Ctrl Pts',(3.96005322310931,1.10013177475018,-7.57735096065689));
#12995=CARTESIAN_POINT('Ctrl Pts',(3.95049372172519,1.10372450057733,-7.57664996040968));
#12996=CARTESIAN_POINT('Ctrl Pts',(3.94712700566097,1.10497226631243,-7.57640436445649));
#12997=CARTESIAN_POINT('Ctrl Pts',(3.94089232620351,1.10725057799854,-7.57595199754452));
#12998=CARTESIAN_POINT('Ctrl Pts',(3.93802607329534,1.10828538836894,-7.57574498964887));
#12999=CARTESIAN_POINT('Ctrl Pts',(3.9314678314928,1.11062439470798,-7.5752734931914));
#13000=CARTESIAN_POINT('Ctrl Pts',(3.927773329516,1.11192131420009,-7.57500942905415));
#13001=CARTESIAN_POINT('Ctrl Pts',(3.91805844771433,1.11527730648662,-7.57431894286253));
#13002=CARTESIAN_POINT('Ctrl Pts',(3.91202763390589,1.11730609292246,-7.57389420224471));
#13003=CARTESIAN_POINT('Ctrl Pts',(3.86192002569974,1.13371164791394,-7.57039511874947));
#13004=CARTESIAN_POINT('Ctrl Pts',(3.81704039864237,1.14552497512976,-7.56745157925536));
#13005=CARTESIAN_POINT('Ctrl Pts',(3.71741807104378,1.16554645724494,-7.56109875264762));
#13006=CARTESIAN_POINT('Ctrl Pts',(3.66256090604426,1.17260715137597,-7.55771426052089));
#13007=CARTESIAN_POINT('Ctrl Pts',(3.55145784837768,1.17902230863197,-7.55078820078201));
#13008=CARTESIAN_POINT('Ctrl Pts',(3.49535288270694,1.17825480126588,-7.54725328098998));
#13009=CARTESIAN_POINT('Ctrl Pts',(3.42515159458367,1.17227261902852,-7.54265367479405));
#13010=CARTESIAN_POINT('Ctrl Pts',(3.41080757898879,1.17078449593913,-7.54170480659726));
#13011=CARTESIAN_POINT('Ctrl Pts',(3.38959066704497,1.16818873714807,-7.54028620263621));
#13012=CARTESIAN_POINT('Ctrl Pts',(3.38269408681089,1.16728290189347,-7.53982271421798));
#13013=CARTESIAN_POINT('Ctrl Pts',(3.37040931943457,1.16555851848352,-7.53899269576496));
#13014=CARTESIAN_POINT('Ctrl Pts',(3.36501798355633,1.16476355415321,-7.53862691011797));
#13015=CARTESIAN_POINT('Ctrl Pts',(3.35362916747868,1.16300340239256,-7.53785090376922));
#13016=CARTESIAN_POINT('Ctrl Pts',(3.34763326671612,1.16202917613298,-7.53744041047483));
#13017=CARTESIAN_POINT('Ctrl Pts',(3.33163964535706,1.15930334075905,-7.53634010672077));
#13018=CARTESIAN_POINT('Ctrl Pts',(3.32165676842966,1.15746883234305,-7.53564772395708));
#13019=CARTESIAN_POINT('Ctrl Pts',(3.27596070484942,1.14845937836228,-7.53245180078064));
#13020=CARTESIAN_POINT('Ctrl Pts',(3.24057212085304,1.13975970599746,-7.52990108477408));
#13021=CARTESIAN_POINT('Ctrl Pts',(3.12211405006214,1.10474229777203,-7.52110011411212));
#13022=CARTESIAN_POINT('Ctrl Pts',(3.0415842270428,1.07085959932035,-7.51464409387036));
#13023=CARTESIAN_POINT('Ctrl Pts',(2.94066112215654,1.01453236404436,-7.5062237636216));
#13024=CARTESIAN_POINT('Ctrl Pts',(2.91629388640277,0.999748642053308,-7.50416536506393));
#13025=CARTESIAN_POINT('Ctrl Pts',(2.87875349053625,0.975066160459048,-7.50097804434586));
#13026=CARTESIAN_POINT('Ctrl Pts',(2.86521121123606,0.965750562022281,-7.49982482722649));
#13027=CARTESIAN_POINT('Ctrl Pts',(2.84770921187083,0.953163388533873,-7.49833428488007));
#13028=CARTESIAN_POINT('Ctrl Pts',(2.84357033802254,0.950145615199158,-7.49798179332134));
#13029=CARTESIAN_POINT('Ctrl Pts',(2.83682787805081,0.945161795954031,-7.49740772525638));
#13030=CARTESIAN_POINT('Ctrl Pts',(2.83421259342468,0.943211803698645,-7.49718509412854));
#13031=CARTESIAN_POINT('Ctrl Pts',(2.82911093237284,0.939374850850652,-7.49675093831355));
#13032=CARTESIAN_POINT('Ctrl Pts',(2.82662390715178,0.937488837088095,-7.49653935625221));
#13033=CARTESIAN_POINT('Ctrl Pts',(2.82107232016178,0.933243973189096,-7.49606713477346));
#13034=CARTESIAN_POINT('Ctrl Pts',(2.81801179095989,0.930879849017439,-7.49580685619984));
#13035=CARTESIAN_POINT('Ctrl Pts',(2.80739828943548,0.922597595576172,-7.49490420832118));
#13036=CARTESIAN_POINT('Ctrl Pts',(2.79990579484172,0.916602083041674,-7.49426692723583));
#13037=CARTESIAN_POINT('Ctrl Pts',(2.73473396053334,0.863131884636884,-7.48871467942003));
#13038=CARTESIAN_POINT('Ctrl Pts',(2.68161143822556,0.810353882608565,-7.4841193203172));
#13039=CARTESIAN_POINT('Ctrl Pts',(2.58219490917316,0.690762617566794,-7.47449950292365));
#13040=CARTESIAN_POINT('Ctrl Pts',(2.53708382043786,0.623493270004544,-7.46948785952424));
#13041=CARTESIAN_POINT('Ctrl Pts',(2.49304658496915,0.540521511846388,-7.46334177058802));
#13042=CARTESIAN_POINT('Ctrl Pts',(2.48707455503482,0.528799288291251,-7.46247473973934));
#13043=CARTESIAN_POINT('Ctrl Pts',(2.47835580874302,0.510952673090671,-7.46115539102211));
#13044=CARTESIAN_POINT('Ctrl Pts',(2.47546289825003,0.504900546175978,-7.46070809240338));
#13045=CARTESIAN_POINT('Ctrl Pts',(2.4703233806384,0.493908021405485,-7.45989570768715));
#13046=CARTESIAN_POINT('Ctrl Pts',(2.46805890613414,0.488976146055614,-7.45953124269526));
#13047=CARTESIAN_POINT('Ctrl Pts',(2.46326615766888,0.478344697240547,-7.45874552669394));
#13048=CARTESIAN_POINT('Ctrl Pts',(2.46074890777709,0.472640365706225,-7.45832391593644));
#13049=CARTESIAN_POINT('Ctrl Pts',(2.45407147222019,0.457177376545754,-7.45718080115945));
#13050=CARTESIAN_POINT('Ctrl Pts',(2.44999773135078,0.447382253977575,-7.45645643231889));
#13051=CARTESIAN_POINT('Ctrl Pts',(2.42950247694841,0.396161552753347,-7.45266618120069));
#13052=CARTESIAN_POINT('Ctrl Pts',(2.41531137661965,0.353888396322722,-7.44952797532048));
#13053=CARTESIAN_POINT('Ctrl Pts',(2.38405264448443,0.239681402833478,-7.44102609144474));
#13054=CARTESIAN_POINT('Ctrl Pts',(2.37130027080308,0.166772635025084,-7.43556544492163));
#13055=CARTESIAN_POINT('Ctrl Pts',(2.36298973644776,0.0620364063141323,
-7.42789490259095));
#13056=CARTESIAN_POINT('Ctrl Pts',(2.36175857158196,0.0308262828120917,
-7.42563304031908));
#13057=CARTESIAN_POINT('Ctrl Pts',(2.36177491127275,-0.0175518500710472,
-7.42219527426652));
#13058=CARTESIAN_POINT('Ctrl Pts',(2.3621554818096,-0.0347048538431212,
-7.42098975325048));
#13059=CARTESIAN_POINT('Ctrl Pts',(2.36314819822653,-0.0572345130445356,
-7.41942898196717));
#13060=CARTESIAN_POINT('Ctrl Pts',(2.36342273796347,-0.0626229830538355,
-7.41905739414851));
#13061=CARTESIAN_POINT('Ctrl Pts',(2.36392615809165,-0.0713263799025043,
-7.41846016669743));
#13062=CARTESIAN_POINT('Ctrl Pts',(2.36413204959821,-0.0746424809090667,
-7.41823330994137));
#13063=CARTESIAN_POINT('Ctrl Pts',(2.36455857239887,-0.081072063061075,
-7.41779486145195));
#13064=CARTESIAN_POINT('Ctrl Pts',(2.36477755038012,-0.0841855846151045,
-7.41758318788287));
#13065=CARTESIAN_POINT('Ctrl Pts',(2.3653381693077,-0.0917281502064954,
-7.41707189533858));
#13066=CARTESIAN_POINT('Ctrl Pts',(2.3656925002255,-0.0961562621719395,
-7.41677296861253));
#13067=CARTESIAN_POINT('Ctrl Pts',(2.3670347256975,-0.11181537776369,-7.4157199435097));
#13068=CARTESIAN_POINT('Ctrl Pts',(2.36815885684629,-0.123034508608218,
-7.41497290254353));
#13069=CARTESIAN_POINT('Ctrl Pts',(2.37135628342574,-0.150904988387344,
-7.41313170964893));
#13070=CARTESIAN_POINT('Ctrl Pts',(2.37362466863601,-0.167531834464555,
-7.41204630573908));
#13071=CARTESIAN_POINT('Ctrl Pts',(2.38513347139392,-0.240250300839454,
-7.40733432865442));
#13072=CARTESIAN_POINT('Ctrl Pts',(2.39807300964722,-0.295682575766201,
-7.40383180037847));
#13073=CARTESIAN_POINT('Ctrl Pts',(2.43758343936905,-0.42264185021791,-7.39560658305977));
#13074=CARTESIAN_POINT('Ctrl Pts',(2.46718873488503,-0.492944241335636,
-7.39088332970528));
#13075=CARTESIAN_POINT('Ctrl Pts',(2.5107463763192,-0.573552821775649,-7.38491289294547));
#13076=CARTESIAN_POINT('Ctrl Pts',(2.51839536227356,-0.587062544660563,
-7.38389276839869));
#13077=CARTESIAN_POINT('Ctrl Pts',(2.52992074156787,-0.606511758666798,
-7.382393372298));
#13078=CARTESIAN_POINT('Ctrl Pts',(2.53358749158466,-0.612574039532877,
-7.38192156487214));
#13079=CARTESIAN_POINT('Ctrl Pts',(2.54018795301456,-0.623267575890443,
-7.38108119440569));
#13080=CARTESIAN_POINT('Ctrl Pts',(2.54309974828614,-0.627912164240503,
-7.38071343288301));
#13081=CARTESIAN_POINT('Ctrl Pts',(2.54923839092688,-0.63755365117648,-7.37994414556265));
#13082=CARTESIAN_POINT('Ctrl Pts',(2.55247087385164,-0.642546759069216,
-7.37954242060587));
#13083=CARTESIAN_POINT('Ctrl Pts',(2.5610026075107,-0.655509132505916,-7.37849066869931));
#13084=CARTESIAN_POINT('Ctrl Pts',(2.56636132769273,-0.663438534579768,
-7.37783845531848));
#13085=CARTESIAN_POINT('Ctrl Pts',(2.59128342030557,-0.699364544516707,
-7.37484205455371));
#13086=CARTESIAN_POINT('Ctrl Pts',(2.61196048694143,-0.726564710922545,
-7.37245636668347));
#13087=CARTESIAN_POINT('Ctrl Pts',(2.676135566738,-0.803774249584545,-7.36532512157706));
#13088=CARTESIAN_POINT('Ctrl Pts',(2.72270194348722,-0.851053525663398,
-7.36047455959067));
#13089=CARTESIAN_POINT('Ctrl Pts',(2.81915164222707,-0.933735967846705,
-7.35115138795128));
#13090=CARTESIAN_POINT('Ctrl Pts',(2.86831396420381,-0.969678949547176,
-7.3466963901952));
#13091=CARTESIAN_POINT('Ctrl Pts',(2.92854601322085,-1.00692954776905,-7.34173031180666));
#13092=CARTESIAN_POINT('Ctrl Pts',(2.93712241950821,-1.01208373267619,-7.34103419675094));
#13093=CARTESIAN_POINT('Ctrl Pts',(2.94916336320602,-1.01911271225521,-7.34007317421425));
#13094=CARTESIAN_POINT('Ctrl Pts',(2.95257290143136,-1.02108020106437,-7.33980284581708));
#13095=CARTESIAN_POINT('Ctrl Pts',(2.95847352604694,-1.02444586023953,-7.33933818447485));
#13096=CARTESIAN_POINT('Ctrl Pts',(2.96095992581449,-1.02585211494429,-7.33914335195661));
#13097=CARTESIAN_POINT('Ctrl Pts',(2.96621850301783,-1.02880105427373,-7.33873336778936));
#13098=CARTESIAN_POINT('Ctrl Pts',(2.9689918426367,-1.03034160963548,-7.33851835712587));
#13099=CARTESIAN_POINT('Ctrl Pts',(2.97589300031738,-1.03413870848479,-7.33798624460505));
#13100=CARTESIAN_POINT('Ctrl Pts',(2.98002823316944,-1.03638179259591,-7.33766997664737));
#13101=CARTESIAN_POINT('Ctrl Pts',(2.99570141204313,-1.04476228211655,-7.33648055482144));
#13102=CARTESIAN_POINT('Ctrl Pts',(3.00732830167183,-1.05073255008836,-7.33561710094718));
#13103=CARTESIAN_POINT('Ctrl Pts',(3.03747289894531,-1.06558264308977,-7.33342042466545));
#13104=CARTESIAN_POINT('Ctrl Pts',(3.05612833523825,-1.07417420566003,-7.33210091350839));
#13105=CARTESIAN_POINT('Ctrl Pts',(3.12808628594222,-1.10505902904771,-7.32712667699415));
#13106=CARTESIAN_POINT('Ctrl Pts',(3.18278021541193,-1.12390861700971,-7.32357945695171));
#13107=CARTESIAN_POINT('Ctrl Pts',(3.31157466755809,-1.15794101315003,-7.31533086677878));
#13108=CARTESIAN_POINT('Ctrl Pts',(3.38618237176527,-1.17015883026993,-7.31061934435885));
#13109=CARTESIAN_POINT('Ctrl Pts',(3.47180595062898,-1.1758477448179,-7.30498743434305));
#13110=CARTESIAN_POINT('Ctrl Pts',(3.48217994915853,-1.17639925159406,-7.30430166016472));
#13111=CARTESIAN_POINT('Ctrl Pts',(3.49927920361848,-1.17708157826402,-7.30316502173826));
#13112=CARTESIAN_POINT('Ctrl Pts',(3.50600083752436,-1.17729215295732,-7.3027166167198));
#13113=CARTESIAN_POINT('Ctrl Pts',(3.51815048893182,-1.17756864402106,-7.30190305216002));
#13114=CARTESIAN_POINT('Ctrl Pts',(3.52357789664097,-1.17765462030809,-7.30153852215557));
#13115=CARTESIAN_POINT('Ctrl Pts',(3.53522806363121,-1.17775862201109,-7.30075359163784));
#13116=CARTESIAN_POINT('Ctrl Pts',(3.54145073621434,-1.17776485357393,-7.3003328379277));
#13117=CARTESIAN_POINT('Ctrl Pts',(3.55850502094474,-1.17764677740409,-7.29917542968816));
#13118=CARTESIAN_POINT('Ctrl Pts',(3.56933510123431,-1.17742234942754,-7.29843571678396));
#13119=CARTESIAN_POINT('Ctrl Pts',(3.63347263269487,-1.17520780571752,-7.29402578887434));
#13120=CARTESIAN_POINT('Ctrl Pts',(3.68659052806748,-1.16974748147788,-7.29024961513138));
#13121=CARTESIAN_POINT('Ctrl Pts',(3.78641748207615,-1.15257824430726,-7.2829285458542));
#13122=CARTESIAN_POINT('Ctrl Pts',(3.83314291179909,-1.14156911274191,-7.27940612396363));
#13123=CARTESIAN_POINT('Ctrl Pts',(3.90607884860877,-1.11960926775308,-7.27381761678875));
#13124=CARTESIAN_POINT('Ctrl Pts',(3.93279312957075,-1.11050735745112,-7.27175135618686));
#13125=CARTESIAN_POINT('Ctrl Pts',(3.99152812727448,-1.08810993835968,-7.2671937460092));
#13126=CARTESIAN_POINT('Ctrl Pts',(4.02334381197907,-1.07434144438989,-7.26471485313204));
#13127=CARTESIAN_POINT('Ctrl Pts',(4.05996151990547,-1.0565374849183,-7.26188482376515));
#13128=CARTESIAN_POINT('Ctrl Pts',(4.06539366050339,-1.05384425766796,-7.26146562114232));
#13129=CARTESIAN_POINT('Ctrl Pts',(4.07326404666124,-1.04986615046214,-7.26085942367658));
#13130=CARTESIAN_POINT('Ctrl Pts',(4.075718850527,-1.0486145286122,-7.26067051467021));
#13131=CARTESIAN_POINT('Ctrl Pts',(4.07816926754783,-1.04735428871579,-7.26048212650804));
#13132=CARTESIAN_POINT('',(2.36176959049357,0.00105055091081243,-7.32538762190826));
#13133=CARTESIAN_POINT('Ctrl Pts',(4.0781692089456,-1.04735431885469,-7.16215973101906));
#13134=CARTESIAN_POINT('Ctrl Pts',(4.03189278705024,-1.07115409849092,-7.165902840997));
#13135=CARTESIAN_POINT('Ctrl Pts',(3.98407925293551,-1.09186616169668,-7.16972076716216));
#13136=CARTESIAN_POINT('Ctrl Pts',(3.87851241723449,-1.12950442731467,-7.17794547881627));
#13137=CARTESIAN_POINT('Ctrl Pts',(3.82052010221274,-1.14531070155958,-7.18234059192762));
#13138=CARTESIAN_POINT('Ctrl Pts',(3.75171322921099,-1.15852036697102,-7.18725395155754));
#13139=CARTESIAN_POINT('Ctrl Pts',(3.7418317223724,-1.16028677905324,-7.18795233897041));
#13140=CARTESIAN_POINT('Ctrl Pts',(3.72804002897374,-1.16257061613521,-7.18891594365121));
#13141=CARTESIAN_POINT('Ctrl Pts',(3.72414833940331,-1.16319500670419,-7.18918661931587));
#13142=CARTESIAN_POINT('Ctrl Pts',(3.71742991545244,-1.16423835687664,-7.18965169543354));
#13143=CARTESIAN_POINT('Ctrl Pts',(3.71460468655344,-1.16466658232457,-7.18984659768361));
#13144=CARTESIAN_POINT('Ctrl Pts',(3.7086416525481,-1.16554822248687,-7.19025651077819));
#13145=CARTESIAN_POINT('Ctrl Pts',(3.70550352445459,-1.16599925742052,-7.19047138184478));
#13146=CARTESIAN_POINT('Ctrl Pts',(3.69771303154502,-1.16708687592374,-7.19100277904636));
#13147=CARTESIAN_POINT('Ctrl Pts',(3.69305854551136,-1.16770832699178,-7.19131847589845));
#13148=CARTESIAN_POINT('Ctrl Pts',(3.67549554654422,-1.16994644914826,-7.19250338905063));
#13149=CARTESIAN_POINT('Ctrl Pts',(3.66256370115544,-1.17137711680587,-7.19336299894246));
#13150=CARTESIAN_POINT('Ctrl Pts',(3.62929399595669,-1.17450070512467,-7.19554767394808));
#13151=CARTESIAN_POINT('Ctrl Pts',(3.60893046682664,-1.17587992628015,-7.19685921455894));
#13152=CARTESIAN_POINT('Ctrl Pts',(3.53068438219167,-1.17913956742849,-7.20183513682557));
#13153=CARTESIAN_POINT('Ctrl Pts',(3.47272613017931,-1.17727978250984,-7.20539074087249));
#13154=CARTESIAN_POINT('Ctrl Pts',(3.34005273553033,-1.16318935857027,-7.21365188002389));
#13155=CARTESIAN_POINT('Ctrl Pts',(3.26591996851086,-1.14801464601014,-7.21836738543932));
#13156=CARTESIAN_POINT('Ctrl Pts',(3.18382284931931,-1.1228015053018,-7.22400382123348));
#13157=CARTESIAN_POINT('Ctrl Pts',(3.17393206868165,-1.11962009421629,-7.22468967317676));
#13158=CARTESIAN_POINT('Ctrl Pts',(3.15771100241562,-1.11416466427672,-7.22582637733591));
#13159=CARTESIAN_POINT('Ctrl Pts',(3.15135567252948,-1.11196648940518,-7.22627476926045));
#13160=CARTESIAN_POINT('Ctrl Pts',(3.13990583621995,-1.10789611302313,-7.22708826712923));
#13161=CARTESIAN_POINT('Ctrl Pts',(3.13480474936594,-1.10604287939175,-7.22745274330312));
#13162=CARTESIAN_POINT('Ctrl Pts',(3.12963152328319,-1.10412285813431,-7.22782450567117));
#13163=CARTESIAN_POINT('Ctrl Pts',(3.12954632443391,-1.10409122571667,-7.22783062888601));
#13164=CARTESIAN_POINT('Ctrl Pts',(3.12934456579987,-1.1040162906975,-7.2278451306125));
#13165=CARTESIAN_POINT('Ctrl Pts',(3.1292280092276,-1.10397297950452,-7.22785350940733));
#13166=CARTESIAN_POINT('Ctrl Pts',(3.12900184752818,-1.10388889943817,-7.22786976942748));
#13167=CARTESIAN_POINT('Ctrl Pts',(3.12889224160648,-1.10384813269604,-7.22787765058237));
#13168=CARTESIAN_POINT('Ctrl Pts',(3.12867952544058,-1.1037689791426,-7.2278929477204));
#13169=CARTESIAN_POINT('Ctrl Pts',(3.12857641449611,-1.10373059420437,-7.22790036364171));
#13170=CARTESIAN_POINT('Ctrl Pts',(3.12837626508327,-1.10365605298337,-7.22791476042095));
#13171=CARTESIAN_POINT('Ctrl Pts',(3.12827922599752,-1.10361989834827,-7.22792174122452));
#13172=CARTESIAN_POINT('Ctrl Pts',(3.12809082732742,-1.10354967683723,-7.22793529574844));
#13173=CARTESIAN_POINT('Ctrl Pts',(3.12799946720125,-1.10351561141296,-7.22794186942074));
#13174=CARTESIAN_POINT('Ctrl Pts',(3.12782206150752,-1.10344943710745,-7.22795463568569));
#13175=CARTESIAN_POINT('Ctrl Pts',(3.1277360154572,-1.10341732950375,-7.22796082823634));
#13176=CARTESIAN_POINT('Ctrl Pts',(3.12756889889575,-1.10335494862061,-7.22797285643134));
#13177=CARTESIAN_POINT('Ctrl Pts',(3.12748782796089,-1.10332467646893,-7.22797869203847));
#13178=CARTESIAN_POINT('Ctrl Pts',(3.12733034659614,-1.10326585263539,-7.22799002882429));
#13179=CARTESIAN_POINT('Ctrl Pts',(3.12725393579239,-1.1032373019493,-7.2279955299701));
#13180=CARTESIAN_POINT('Ctrl Pts',(3.12710548182472,-1.103181814957,-7.22800621874234));
#13181=CARTESIAN_POINT('Ctrl Pts',(3.12703343832857,-1.10315487953001,-7.22801140633984));
#13182=CARTESIAN_POINT('Ctrl Pts',(3.12689344658147,-1.10310252416426,-7.2280214874744));
#13183=CARTESIAN_POINT('Ctrl Pts',(3.12682549803937,-1.10307710500405,-7.22802638098567));
#13184=CARTESIAN_POINT('Ctrl Pts',(3.12669344271404,-1.10302768995398,-7.22803589206598));
#13185=CARTESIAN_POINT('Ctrl Pts',(3.12662933567708,-1.1030036947547,-7.22804050961189));
#13186=CARTESIAN_POINT('Ctrl Pts',(3.12650472736896,-1.10295704160498,-7.22804948563811));
#13187=CARTESIAN_POINT('Ctrl Pts',(3.12644422586398,-1.10293438426287,-7.22805384409857));
#13188=CARTESIAN_POINT('Ctrl Pts',(3.12632660874939,-1.10289032653477,-7.22806231768533));
#13189=CARTESIAN_POINT('Ctrl Pts',(3.12626949293543,-1.10286892668916,-7.22806643279382));
#13190=CARTESIAN_POINT('Ctrl Pts',(3.12615844224776,-1.10282730897758,-7.22807443434771));
#13191=CARTESIAN_POINT('Ctrl Pts',(3.12610450719502,-1.10280709159188,-7.22807832077715));
#13192=CARTESIAN_POINT('Ctrl Pts',(3.12599962686868,-1.10276776875449,-7.2280858786627));
#13193=CARTESIAN_POINT('Ctrl Pts',(3.12594868143424,-1.10274866372848,-7.22808955010477));
#13194=CARTESIAN_POINT('Ctrl Pts',(3.12584960193837,-1.10271150013656,-7.22809669079727));
#13195=CARTESIAN_POINT('Ctrl Pts',(3.12580146773137,-1.10269344194785,-7.22810016003541));
#13196=CARTESIAN_POINT('Ctrl Pts',(3.12570784407525,-1.10265831079342,-7.22810690826171));
#13197=CARTESIAN_POINT('Ctrl Pts',(3.12566235450039,-1.10264123816444,-7.22811018723868));
#13198=CARTESIAN_POINT('Ctrl Pts',(3.12557386441292,-1.10260802082552,-7.22811656610591));
#13199=CARTESIAN_POINT('Ctrl Pts',(3.12553086379293,-1.10259187641686,-7.22811966598589));
#13200=CARTESIAN_POINT('Ctrl Pts',(3.12544720606644,-1.10256046187832,-7.22812569709862));
#13201=CARTESIAN_POINT('Ctrl Pts',(3.12540654885501,-1.10254519201314,-7.22812862832288));
#13202=CARTESIAN_POINT('Ctrl Pts',(3.12532744174252,-1.10251547630215,-7.22813433189665));
#13203=CARTESIAN_POINT('Ctrl Pts',(3.125288991759,-1.10250103069625,-7.22813710423782));
#13204=CARTESIAN_POINT('Ctrl Pts',(3.12521417163555,-1.10247291641225,-7.228142499194));
#13205=CARTESIAN_POINT('Ctrl Pts',(3.12517780141175,-1.10245924794408,-7.22814512180231));
#13206=CARTESIAN_POINT('Ctrl Pts',(3.12510702140893,-1.10243264377458,-7.22815022586499));
#13207=CARTESIAN_POINT('Ctrl Pts',(3.12507261155463,-1.10241970826029,-7.2281527073134));
#13208=CARTESIAN_POINT('Ctrl Pts',(3.11889598244139,-1.1000974307304,-7.22859814908234));
#13209=CARTESIAN_POINT('Ctrl Pts',(3.11277328018497,-1.09773683867651,-7.22904279728506));
#13210=CARTESIAN_POINT('Ctrl Pts',(3.09417800232924,-1.09038839598744,-7.23040288465889));
#13211=CARTESIAN_POINT('Ctrl Pts',(3.08177111956379,-1.08523836512921,-7.23132366536547));
#13212=CARTESIAN_POINT('Ctrl Pts',(3.0533827131784,-1.07288107754954,-7.2334622600049));
#13213=CARTESIAN_POINT('Ctrl Pts',(3.03746893453555,-1.06552708577844,-7.23468474647203));
#13214=CARTESIAN_POINT('Ctrl Pts',(2.98311807810975,-1.03892286713517,-7.23894323940753));
#13215=CARTESIAN_POINT('Ctrl Pts',(2.94557760240269,-1.01792713896474,-7.24203281457939));
#13216=CARTESIAN_POINT('Ctrl Pts',(2.84281118088179,-0.952828748158203,
-7.25088773410883));
#13217=CARTESIAN_POINT('Ctrl Pts',(2.78073700149172,-0.904176119073045,
-7.25673434805639));
#13218=CARTESIAN_POINT('Ctrl Pts',(2.70817999179209,-0.834535718238671,
-7.26392979663895));
#13219=CARTESIAN_POINT('Ctrl Pts',(2.69280760370369,-0.818934899488915,
-7.26547700626055));
#13220=CARTESIAN_POINT('Ctrl Pts',(2.67386610554319,-0.798607959978751,
-7.26740314335034));
#13221=CARTESIAN_POINT('Ctrl Pts',(2.66988637399968,-0.794272438414205,
-7.26780898769877));
#13222=CARTESIAN_POINT('Ctrl Pts',(2.66363852330199,-0.787362770106394,
-7.26844771183));
#13223=CARTESIAN_POINT('Ctrl Pts',(2.6613489314276,-0.784808302965292,-7.26868212141593));
#13224=CARTESIAN_POINT('Ctrl Pts',(2.65702659302985,-0.779943328058985,
-7.26912523605247));
#13225=CARTESIAN_POINT('Ctrl Pts',(2.65499175622809,-0.777634874722648,
-7.26933408643254));
#13226=CARTESIAN_POINT('Ctrl Pts',(2.65021416581738,-0.772171844661248,
-7.26982507869239));
#13227=CARTESIAN_POINT('Ctrl Pts',(2.64747912575672,-0.769010604350966,
-7.27010666044162));
#13228=CARTESIAN_POINT('Ctrl Pts',(2.6387274723152,-0.758785666865766,-7.27100955505673));
#13229=CARTESIAN_POINT('Ctrl Pts',(2.63277730435533,-0.751665201079264,
-7.27162632253638));
#13230=CARTESIAN_POINT('Ctrl Pts',(2.58552534371156,-0.693741840681457,
-7.2765548998223));
#13231=CARTESIAN_POINT('Ctrl Pts',(2.54843557126951,-0.639638675217191,
-7.28061942503178));
#13232=CARTESIAN_POINT('Ctrl Pts',(2.49345074093151,-0.543064549221617,
-7.28749797029545));
#13233=CARTESIAN_POINT('Ctrl Pts',(2.47319423423252,-0.502124718753124,
-7.29031099425505));
#13234=CARTESIAN_POINT('Ctrl Pts',(2.43636275694106,-0.415339709853604,
-7.29622383666118));
#13235=CARTESIAN_POINT('Ctrl Pts',(2.42015456135697,-0.369436279673885,
-7.29932508744073));
#13236=CARTESIAN_POINT('Ctrl Pts',(2.40386173285749,-0.312241895559978,
-7.30323258168735));
#13237=CARTESIAN_POINT('Ctrl Pts',(2.40103634525039,-0.301777503336854,
-7.30394910241728));
#13238=CARTESIAN_POINT('Ctrl Pts',(2.39680104595856,-0.285184410987463,
-7.30508848591029));
#13239=CARTESIAN_POINT('Ctrl Pts',(2.39529505447766,-0.27908068818422,-7.30550828587332));
#13240=CARTESIAN_POINT('Ctrl Pts',(2.39258140445568,-0.267691045082041,
-7.30629304079023));
#13241=CARTESIAN_POINT('Ctrl Pts',(2.39136123629985,-0.262408253565323,
-7.30665758760299));
#13242=CARTESIAN_POINT('Ctrl Pts',(2.38904289480896,-0.252045022624808,
-7.30737388973229));
#13243=CARTESIAN_POINT('Ctrl Pts',(2.3879417898328,-0.246965360854379,-7.30772554289584));
#13244=CARTESIAN_POINT('Ctrl Pts',(2.38554040392649,-0.235521834293679,
-7.30851905507155));
#13245=CARTESIAN_POINT('Ctrl Pts',(2.38425908114074,-0.229154208867454,
-7.30896150021165));
#13246=CARTESIAN_POINT('Ctrl Pts',(2.38115766622933,-0.213053982500291,
-7.31008260582606));
#13247=CARTESIAN_POINT('Ctrl Pts',(2.37940754428838,-0.203308580360016,
-7.31076341986982));
#13248=CARTESIAN_POINT('Ctrl Pts',(2.36706479407936,-0.129221253194858,
-7.31595686887277));
#13249=CARTESIAN_POINT('Ctrl Pts',(2.36171133875935,-0.0641335218267783,
-7.32063005701069));
#13250=CARTESIAN_POINT('Ctrl Pts',(2.36176951954998,0.00105120331072818,
-7.32538754544545));
#13251=CARTESIAN_POINT('Ctrl Pts',(2.36176951897595,0.00105055998136013,
-7.32538749849224));
#13252=CARTESIAN_POINT('Ctrl Pts',(2.36184243587445,0.0827953861394267,
-7.33135362058476));
#13253=CARTESIAN_POINT('Ctrl Pts',(2.37042547558946,0.164315098730552,-7.33742953962348));
#13254=CARTESIAN_POINT('Ctrl Pts',(2.38948890391776,0.254221795642659,-7.34393441290863));
#13255=CARTESIAN_POINT('Ctrl Pts',(2.39172231424939,0.264122561087035,-7.34464772615235));
#13256=CARTESIAN_POINT('Ctrl Pts',(2.39534885736636,0.279283395544758,-7.34573413890476));
#13257=CARTESIAN_POINT('Ctrl Pts',(2.39665086308174,0.284564500223568,-7.34611147720832));
#13258=CARTESIAN_POINT('Ctrl Pts',(2.39914707353257,0.294395898268841,-7.34681164566584));
#13259=CARTESIAN_POINT('Ctrl Pts',(2.40033203985735,0.298948402640113,-7.3471349434781));
#13260=CARTESIAN_POINT('Ctrl Pts',(2.40236167494422,0.306558685530069,-7.3476737087491));
#13261=CARTESIAN_POINT('Ctrl Pts',(2.40319146806741,0.309620333042458,-7.34788999859804));
#13262=CARTESIAN_POINT('Ctrl Pts',(2.40479184859045,0.315432078538282,-7.34829965056871));
#13263=CARTESIAN_POINT('Ctrl Pts',(2.40556008301194,0.318182776749839,-7.3484931487926));
#13264=CARTESIAN_POINT('Ctrl Pts',(2.40741068161247,0.324717093114046,-7.34895193787748));
#13265=CARTESIAN_POINT('Ctrl Pts',(2.4085020274289,0.328498164516393,-7.34921672146595));
#13266=CARTESIAN_POINT('Ctrl Pts',(2.41243382993525,0.341868374897534,-7.35015079328584));
#13267=CARTESIAN_POINT('Ctrl Pts',(2.41537754522886,0.351427051522242,-7.35081451658718));
#13268=CARTESIAN_POINT('Ctrl Pts',(2.43718135149746,0.419148071552181,-7.35549551203285));
#13269=CARTESIAN_POINT('Ctrl Pts',(2.46042628962904,0.47580906762492,-7.35930230538704));
#13270=CARTESIAN_POINT('Ctrl Pts',(2.50974391247105,0.573581496989081,-7.36608482172921));
#13271=CARTESIAN_POINT('Ctrl Pts',(2.53415507307774,0.615366299254801,-7.36906087915854));
#13272=CARTESIAN_POINT('Ctrl Pts',(2.5874105310899,0.694856085767757,-7.37505996221279));
#13273=CARTESIAN_POINT('Ctrl Pts',(2.61610060199798,0.732552522774052,-7.37807526913517));
#13274=CARTESIAN_POINT('Ctrl Pts',(2.65452626388713,0.777185089491855,-7.3819373798523));
#13275=CARTESIAN_POINT('Ctrl Pts',(2.66220270022906,0.785840252081935,-7.38270091629134));
#13276=CARTESIAN_POINT('Ctrl Pts',(2.67361826217614,0.798335507435076,-7.38382565087836));
#13277=CARTESIAN_POINT('Ctrl Pts',(2.67725824097824,0.802265574746541,-7.38418273850289));
#13278=CARTESIAN_POINT('Ctrl Pts',(2.68467733332273,0.810167115032765,-7.38490755162201));
#13279=CARTESIAN_POINT('Ctrl Pts',(2.68845761549258,0.814137302804437,-7.38527532129913));
#13280=CARTESIAN_POINT('Ctrl Pts',(2.69639413052852,0.822356833620065,-7.38604432634151));
#13281=CARTESIAN_POINT('Ctrl Pts',(2.70055508116586,0.826601384226098,-7.3864457588098));
#13282=CARTESIAN_POINT('Ctrl Pts',(2.71148723228862,0.83758560221194,-7.38749607367599));
#13283=CARTESIAN_POINT('Ctrl Pts',(2.7183085103172,0.844274583515395,-7.38814713204762));
#13284=CARTESIAN_POINT('Ctrl Pts',(2.74734697110669,0.872064969480325,-7.39090150189392));
#13285=CARTESIAN_POINT('Ctrl Pts',(2.77030007837068,0.892376484648271,-7.39303750174718));
#13286=CARTESIAN_POINT('Ctrl Pts',(2.88013590131762,0.982183056159513,-7.40308156844346));
#13287=CARTESIAN_POINT('Ctrl Pts',(2.97577712964786,1.04002794298598,-7.41140986004234));
#13288=CARTESIAN_POINT('Ctrl Pts',(3.10217961238231,1.09385298051383,-7.42128595344743));
#13289=CARTESIAN_POINT('Ctrl Pts',(3.12659832350609,1.10330269731129,-7.42314259493292));
#13290=CARTESIAN_POINT('Ctrl Pts',(3.15696084240543,1.11390307356102,-7.42537276390583));
#13291=CARTESIAN_POINT('Ctrl Pts',(3.16262307306998,1.11583164762738,-7.42578536431569));
#13292=CARTESIAN_POINT('Ctrl Pts',(3.17157548421258,1.11880494616473,-7.42643226240809));
#13293=CARTESIAN_POINT('Ctrl Pts',(3.17485588956654,1.11987845562197,-7.42666815477586));
#13294=CARTESIAN_POINT('Ctrl Pts',(3.18106425277223,1.12187996416063,-7.42711236553682));
#13295=CARTESIAN_POINT('Ctrl Pts',(3.18399109949272,1.12281092454739,-7.42732084183016));
#13296=CARTESIAN_POINT('Ctrl Pts',(3.19080166391844,1.1249479025798,-7.4278038177268));
#13297=CARTESIAN_POINT('Ctrl Pts',(3.19468802725204,1.12614526854072,-7.42807781966024));
#13298=CARTESIAN_POINT('Ctrl Pts',(3.20746497842382,1.13000942817179,-7.42897362701713));
#13299=CARTESIAN_POINT('Ctrl Pts',(3.21638116451142,1.13259133599541,-7.42959081085674));
#13300=CARTESIAN_POINT('Ctrl Pts',(3.30461931651397,1.15701604834792,-7.4356292015358));
#13301=CARTESIAN_POINT('Ctrl Pts',(3.38600528911636,1.17059883606947,-7.44065760695193));
#13302=CARTESIAN_POINT('Ctrl Pts',(3.51974568914811,1.17871783523835,-7.44895191517728));
#13303=CARTESIAN_POINT('Ctrl Pts',(3.5714860429165,1.1784499308291,-7.45216626088356));
#13304=CARTESIAN_POINT('Ctrl Pts',(3.64264827103797,1.17339077961384,-7.45672610473294));
#13305=CARTESIAN_POINT('Ctrl Pts',(3.66221938496886,1.17150591989179,-7.45799436912116));
#13306=CARTESIAN_POINT('Ctrl Pts',(3.69643933009624,1.16734337435549,-7.46024332415843));
#13307=CARTESIAN_POINT('Ctrl Pts',(3.71110966822755,1.16527728710072,-7.46121764982164));
#13308=CARTESIAN_POINT('Ctrl Pts',(3.7326780250518,1.16182360605822,-7.46266695613577));
#13309=CARTESIAN_POINT('Ctrl Pts',(3.73960921142448,1.16064999244261,-7.46313528068593));
#13310=CARTESIAN_POINT('Ctrl Pts',(3.75190200106858,1.15845514817542,-7.46397064963821));
#13311=CARTESIAN_POINT('Ctrl Pts',(3.75726783860394,1.15745855718234,-7.46433691241976));
#13312=CARTESIAN_POINT('Ctrl Pts',(3.76854971247594,1.15528196079142,-7.46511050347151));
#13313=CARTESIAN_POINT('Ctrl Pts',(3.77446398089755,1.15409372686963,-7.4655180809496));
#13314=CARTESIAN_POINT('Ctrl Pts',(3.79011800887891,1.15082336639973,-7.46660241557859));
#13315=CARTESIAN_POINT('Ctrl Pts',(3.79984075402518,1.14866307449062,-7.46728161601366));
#13316=CARTESIAN_POINT('Ctrl Pts',(3.84313430712023,1.13846581172964,-7.4703323530194));
#13317=CARTESIAN_POINT('Ctrl Pts',(3.87636647093499,1.12907928138577,-7.47274599948933));
#13318=CARTESIAN_POINT('Ctrl Pts',(4.00417984980738,1.08683286897286,-7.48231748144728));
#13319=CARTESIAN_POINT('Ctrl Pts',(4.09482696600384,1.04342893878017,-7.48978057988738));
#13320=CARTESIAN_POINT('Ctrl Pts',(4.1969291888781,0.977429846577178,-7.49857178806097));
#13321=CARTESIAN_POINT('Ctrl Pts',(4.21466129290306,0.965266936998673,-7.50011219556277));
#13322=CARTESIAN_POINT('Ctrl Pts',(4.24297525080469,0.944683454289842,-7.50258302830171));
#13323=CARTESIAN_POINT('Ctrl Pts',(4.2537621954935,0.936554442277191,-7.50352709800399));
#13324=CARTESIAN_POINT('Ctrl Pts',(4.2681615103941,0.925309632067565,-7.5047885187767));
#13325=CARTESIAN_POINT('Ctrl Pts',(4.27189780453866,0.922355198471373,-7.50511593942487));
#13326=CARTESIAN_POINT('Ctrl Pts',(4.27810189143184,0.917387916457647,-7.50565966168908));
#13327=CARTESIAN_POINT('Ctrl Pts',(4.28057959369621,0.915387608734789,-7.50587681741037));
#13328=CARTESIAN_POINT('Ctrl Pts',(4.28525603837566,0.911580772474331,-7.50628665285588));
#13329=CARTESIAN_POINT('Ctrl Pts',(4.28745639145432,0.909776288037184,-7.50647947796868));
#13330=CARTESIAN_POINT('Ctrl Pts',(4.29265243748205,0.905483478180304,-7.50693486227134));
#13331=CARTESIAN_POINT('Ctrl Pts',(4.29564239483926,0.902988215348579,-7.50719693190891));
#13332=CARTESIAN_POINT('Ctrl Pts',(4.30607926643327,0.894189957352579,-7.50811204707535));
#13333=CARTESIAN_POINT('Ctrl Pts',(4.31346043548588,0.887809096722862,-7.50875981770221));
#13334=CARTESIAN_POINT('Ctrl Pts',(4.37431224652546,0.833868285022994,-7.51411346174223));
#13335=CARTESIAN_POINT('Ctrl Pts',(4.42343279309649,0.781610747760335,-7.51852749624356));
#13336=CARTESIAN_POINT('Ctrl Pts',(4.5035778386305,0.679055847571457,-7.52657831834167));
#13337=CARTESIAN_POINT('Ctrl Pts',(4.53615057322714,0.630278622722896,-7.53019917419818));
#13338=CARTESIAN_POINT('Ctrl Pts',(4.57536544014826,0.560860934983936,-7.53528150761178));
#13339=CARTESIAN_POINT('Ctrl Pts',(4.58527339946112,0.54216279213002,-7.53664338901217));
#13340=CARTESIAN_POINT('Ctrl Pts',(4.60163643890632,0.509163517637524,-7.53904292912152));
#13341=CARTESIAN_POINT('Ctrl Pts',(4.60831949937232,0.494981209105619,-7.54007293641988));
#13342=CARTESIAN_POINT('Ctrl Pts',(4.61765134721941,0.474107052982491,-7.54158927476668));
#13343=CARTESIAN_POINT('Ctrl Pts',(4.62052523363759,0.467517245781826,-7.54206801240573));
#13344=CARTESIAN_POINT('Ctrl Pts',(4.62548259047749,0.455859921671493,-7.54291517124143));
#13345=CARTESIAN_POINT('Ctrl Pts',(4.62759138696171,0.450803357623126,-7.54328273091139));
#13346=CARTESIAN_POINT('Ctrl Pts',(4.63191835474615,0.440220716113297,-7.54405225834637));
#13347=CARTESIAN_POINT('Ctrl Pts',(4.63413004550781,0.434692174044824,-7.54445442963685));
#13348=CARTESIAN_POINT('Ctrl Pts',(4.63979860265615,0.420204921372195,-7.54550883678833));
#13349=CARTESIAN_POINT('Ctrl Pts',(4.6431879363808,0.411220439311926,-7.54616328015078));
#13350=CARTESIAN_POINT('Ctrl Pts',(4.65708892325133,0.37296128711295,-7.54895307983373));
#13351=CARTESIAN_POINT('Ctrl Pts',(4.66654768156233,0.343320108195707,-7.55112219011722));
#13352=CARTESIAN_POINT('Ctrl Pts',(4.70244830288698,0.213244596650607,-7.56068015706712));
#13353=CARTESIAN_POINT('Ctrl Pts',(4.71671304202461,0.109938252689443,-7.56842376183125));
#13354=CARTESIAN_POINT('Ctrl Pts',(4.71736622886991,-0.0156158618247626,
-7.57750567089768));
#13355=CARTESIAN_POINT('Ctrl Pts',(4.716877212013,-0.0373591426470613,-7.57906420987694));
#13356=CARTESIAN_POINT('Ctrl Pts',(4.71510343489739,-0.0726759822207703,
-7.58156069224452));
#13357=CARTESIAN_POINT('Ctrl Pts',(4.714184670166,-0.0862621879796819,-7.58251261002496));
#13358=CARTESIAN_POINT('Ctrl Pts',(4.7126254698977,-0.104590718879772,-7.58378273117153));
#13359=CARTESIAN_POINT('Ctrl Pts',(4.71219151337433,-0.10934892088687,-7.58411117793075));
#13360=CARTESIAN_POINT('Ctrl Pts',(4.71141979816182,-0.117276849438524,
-7.5846561359849));
#13361=CARTESIAN_POINT('Ctrl Pts',(4.71109811025182,-0.120448035470747,
-7.58487350931117));
#13362=CARTESIAN_POINT('Ctrl Pts',(4.71046512540397,-0.126445385579752,
-7.58528340079781));
#13363=CARTESIAN_POINT('Ctrl Pts',(4.71015646290111,-0.129271787298657,
-7.58547606661611));
#13364=CARTESIAN_POINT('Ctrl Pts',(4.70940188344247,-0.135957009251804,
-7.58593063614728));
#13365=CARTESIAN_POINT('Ctrl Pts',(4.70894710163209,-0.13981482562664,-7.58619205454313));
#13366=CARTESIAN_POINT('Ctrl Pts',(4.70727727039615,-0.153401175759362,
-7.58710976702059));
#13367=CARTESIAN_POINT('Ctrl Pts',(4.70595980233641,-0.163117039810494,
-7.58776071753037));
#13368=CARTESIAN_POINT('Ctrl Pts',(4.69409596646019,-0.243094686519461,
-7.5930835628376));
#13369=CARTESIAN_POINT('Ctrl Pts',(4.67733126855029,-0.312296423694265,
-7.59746797797777));
#13370=CARTESIAN_POINT('Ctrl Pts',(4.63543425501089,-0.435359471362672,
-7.60550918761953));
#13371=CARTESIAN_POINT('Ctrl Pts',(4.61228242720532,-0.489638728645046,
-7.60915095186344));
#13372=CARTESIAN_POINT('Ctrl Pts',(4.5753970519282,-0.560805312091225,-7.61425998699209));
#13373=CARTESIAN_POINT('Ctrl Pts',(4.56511975651704,-0.579386695731533,
-7.61562642941479));
#13374=CARTESIAN_POINT('Ctrl Pts',(4.54636948148894,-0.611223649158535,
-7.61803327764238));
#13375=CARTESIAN_POINT('Ctrl Pts',(4.53812260221285,-0.624606314666664,
-7.61906596603792));
#13376=CARTESIAN_POINT('Ctrl Pts',(4.5257132296598,-0.64386947151939,-7.62058552464857));
#13377=CARTESIAN_POINT('Ctrl Pts',(4.52176048484166,-0.649883540476997,
-7.62106475479168));
#13378=CARTESIAN_POINT('Ctrl Pts',(4.51470139804205,-0.660412355350961,
-7.62191247615958));
#13379=CARTESIAN_POINT('Ctrl Pts',(4.51161817041951,-0.664942395535229,
-7.62228010206081));
#13380=CARTESIAN_POINT('Ctrl Pts',(4.50512077440949,-0.674346935256228,
-7.62304946148975));
#13381=CARTESIAN_POINT('Ctrl Pts',(4.50170105535977,-0.679217391996296,
-7.62345139649413));
#13382=CARTESIAN_POINT('Ctrl Pts',(4.49267641491328,-0.691865599419147,
-7.62450449501469));
#13383=CARTESIAN_POINT('Ctrl Pts',(4.48701327534066,-0.699601067371228,
-7.62515785593197));
#13384=CARTESIAN_POINT('Ctrl Pts',(4.46266664202129,-0.73201903260682,-7.62793632418563));
#13385=CARTESIAN_POINT('Ctrl Pts',(4.44310978148363,-0.756027000026072,
-7.6300948429159));
#13386=CARTESIAN_POINT('Ctrl Pts',(4.36766627637729,-0.841527648912774,
-7.63817018883987));
#13387=CARTESIAN_POINT('Ctrl Pts',(4.30626961959595,-0.897823380166583,
-7.64429346404369));
#13388=CARTESIAN_POINT('Ctrl Pts',(4.19752946974113,-0.9781806811457,-7.65419106255317));
#13389=CARTESIAN_POINT('Ctrl Pts',(4.1535672243875,-1.00636042093365,-7.65797488144446));
#13390=CARTESIAN_POINT('Ctrl Pts',(4.10178348345933,-1.03489234583026,-7.66208708064864));
#13391=CARTESIAN_POINT('Ctrl Pts',(4.0956605067869,-1.0381956205251,-7.66256806356824));
#13392=CARTESIAN_POINT('Ctrl Pts',(4.08627127854972,-1.04315409470419,-7.66329724659285));
#13393=CARTESIAN_POINT('Ctrl Pts',(4.08302611141962,-1.04484857267568,-7.66354775914025));
#13394=CARTESIAN_POINT('Ctrl Pts',(4.07923865954719,-1.04680378662507,-7.66383833136182));
#13395=CARTESIAN_POINT('Ctrl Pts',(4.07870406858489,-1.04707924263269,-7.66387930335525));
#13396=CARTESIAN_POINT('Ctrl Pts',(4.07816926754758,-1.04735428871592,-7.66392024962001));
#13397=CARTESIAN_POINT('Origin',(3.53951905042299,8.32667268468867E-16,
0.924367114736157));
#13398=CARTESIAN_POINT('',(4.07816941731682,-1.04735421169017,-8.2621380879065));
#13399=CARTESIAN_POINT('',(4.0781691572555,-1.0473543454387,-8.16230176652656));
#13400=CARTESIAN_POINT('',(4.07816926754759,-1.04735428871592,0.924367114736157));
#13401=CARTESIAN_POINT('',(2.36176950623101,-0.000671540642540941,-7.92526768877284));
#13402=CARTESIAN_POINT('Ctrl Pts',(4.07816941731679,-1.04735421169019,-8.2621380879065));
#13403=CARTESIAN_POINT('Ctrl Pts',(4.09787021646655,-1.03722216412531,-8.26074508697215));
#13404=CARTESIAN_POINT('Ctrl Pts',(4.11729263674474,-1.02653040785042,-8.25934001281429));
#13405=CARTESIAN_POINT('Ctrl Pts',(4.15925528987737,-1.00186036158223,-8.25621923947244));
#13406=CARTESIAN_POINT('Ctrl Pts',(4.18163663589062,-0.987664937537115,
-8.25449844096451));
#13407=CARTESIAN_POINT('Ctrl Pts',(4.21101323274282,-0.967611987992991,
-8.25215165275585));
#13408=CARTESIAN_POINT('Ctrl Pts',(4.21844791336526,-0.962409989382561,
-8.25154987201976));
#13409=CARTESIAN_POINT('Ctrl Pts',(4.23056803536388,-0.953719285308015,
-8.25055542681309));
#13410=CARTESIAN_POINT('Ctrl Pts',(4.23528903781803,-0.950280641344982,
-8.25016466424955));
#13411=CARTESIAN_POINT('Ctrl Pts',(4.24442501643088,-0.943521677708989,
-8.24940169185106));
#13412=CARTESIAN_POINT('Ctrl Pts',(4.24884259995885,-0.940205125230167,
-8.24902963348167));
#13413=CARTESIAN_POINT('Ctrl Pts',(4.25918530220381,-0.932325840442442,
-8.24815103840464));
#13414=CARTESIAN_POINT('Ctrl Pts',(4.26509055981882,-0.927737552864946,
-8.24764351655232));
#13415=CARTESIAN_POINT('Ctrl Pts',(4.28452728992103,-0.912336449667722,
-8.24595312015627));
#13416=CARTESIAN_POINT('Ctrl Pts',(4.29786335948661,-0.901281824969567,
-8.24476077574491));
#13417=CARTESIAN_POINT('Ctrl Pts',(4.32917328033652,-0.874141216498856,
-8.24188072854002));
#13418=CARTESIAN_POINT('Ctrl Pts',(4.34690567509686,-0.857789816166167,
-8.24018286891336));
#13419=CARTESIAN_POINT('Ctrl Pts',(4.41057444698654,-0.795355415259501,
-8.23383374641222));
#13420=CARTESIAN_POINT('Ctrl Pts',(4.45316769001884,-0.746037725967231,
-8.22906555558485));
#13421=CARTESIAN_POINT('Ctrl Pts',(4.4929673045481,-0.691402906601309,-8.22410538503906));
#13422=CARTESIAN_POINT('Ctrl Pts',(4.49446062887,-0.689338911076299,-8.22391845959956));
#13423=CARTESIAN_POINT('Ctrl Pts',(4.51123550305327,-0.665994431249304,
-8.22180954230394));
#13424=CARTESIAN_POINT('Ctrl Pts',(4.52581001751704,-0.64421397816899,-8.21989101172835));
#13425=CARTESIAN_POINT('Ctrl Pts',(4.54703476143244,-0.610084333994029,
-8.2169742089834));
#13426=CARTESIAN_POINT('Ctrl Pts',(4.55421115809595,-0.598072532699133,
-8.21596398108153));
#13427=CARTESIAN_POINT('Ctrl Pts',(4.57273307190567,-0.565777214057839,
-8.21329574267617));
#13428=CARTESIAN_POINT('Ctrl Pts',(4.58369592508163,-0.545279651801057,
-8.2116513246021));
#13429=CARTESIAN_POINT('Ctrl Pts',(4.59671901417798,-0.519094725044495,
-8.20962316698562));
#13430=CARTESIAN_POINT('Ctrl Pts',(4.59935112062951,-0.513699409882844,
-8.20920906439331));
#13431=CARTESIAN_POINT('Ctrl Pts',(4.60343368236609,-0.505165978886334,
-8.20856032695725));
#13432=CARTESIAN_POINT('Ctrl Pts',(4.60491172633417,-0.502041290312482,
-8.2083240830048));
#13433=CARTESIAN_POINT('Ctrl Pts',(4.60767681181786,-0.496128500068766,
-8.2078795633681));
#13434=CARTESIAN_POINT('Ctrl Pts',(4.60896669700945,-0.493341892863146,
-8.20767112709396));
#13435=CARTESIAN_POINT('Ctrl Pts',(4.61196606337652,-0.486795158866127,
-8.20718386526916));
#13436=CARTESIAN_POINT('Ctrl Pts',(4.61366668204815,-0.483031043566971,
-8.20690557419312));
#13437=CARTESIAN_POINT('Ctrl Pts',(4.61916902760897,-0.47067949178062,-8.20599823306855));
#13438=CARTESIAN_POINT('Ctrl Pts',(4.62288796597554,-0.462055260417316,
-8.20537390274077));
#13439=CARTESIAN_POINT('Ctrl Pts',(4.64294164298617,-0.413977066192752,
-8.20193920370032));
#13440=CARTESIAN_POINT('Ctrl Pts',(4.65722622700692,-0.373697611893329,
-8.19923096705546));
#13441=CARTESIAN_POINT('Ctrl Pts',(4.67693768935054,-0.306767431839981,
-8.1948687038696));
#13442=CARTESIAN_POINT('Ctrl Pts',(4.68368616563274,-0.280551408272435,
-8.1931934384416));
#13443=CARTESIAN_POINT('Ctrl Pts',(4.70740820313345,-0.173200991391785,
-8.1863922214657));
#13444=CARTESIAN_POINT('Ctrl Pts',(4.71669733160403,-0.0906249788242832,
-8.18127545668112));
#13445=CARTESIAN_POINT('Ctrl Pts',(4.71733465130768,0.00607210071476501,
-8.17497260465963));
#13446=CARTESIAN_POINT('Ctrl Pts',(4.71718206071303,0.0199064941922861,
-8.17406405520422));
#13447=CARTESIAN_POINT('Ctrl Pts',(4.71658679466932,0.0406800681975707,
-8.17268803815387));
#13448=CARTESIAN_POINT('Ctrl Pts',(4.7163263134372,0.0476235736809692,-8.17222613817922));
#13449=CARTESIAN_POINT('Ctrl Pts',(4.71576774865549,0.059667051544863,-8.17142136979478));
#13450=CARTESIAN_POINT('Ctrl Pts',(4.7154978924116,0.0647681938443807,-8.17107937850627));
#13451=CARTESIAN_POINT('Ctrl Pts',(4.71486582255102,0.0754041951773591,
-8.17036389758792));
#13452=CARTESIAN_POINT('Ctrl Pts',(4.71449767778961,0.0809385620458983,
-8.16999023309416));
#13453=CARTESIAN_POINT('Ctrl Pts',(4.71353168187364,0.0940602300973112,
-8.16910094754776));
#13454=CARTESIAN_POINT('Ctrl Pts',(4.71289935663556,0.101644665258518,-8.16858427303211));
#13455=CARTESIAN_POINT('Ctrl Pts',(4.71051362700583,0.127259257566909,-8.16683003091132));
#13456=CARTESIAN_POINT('Ctrl Pts',(4.70841784309341,0.145254144319727,-8.16558198331525));
#13457=CARTESIAN_POINT('Ctrl Pts',(4.69797423765539,0.219897833869709,-8.16033683817268));
#13458=CARTESIAN_POINT('Ctrl Pts',(4.68591705833291,0.275941005798534,-8.15622925892115));
#13459=CARTESIAN_POINT('Ctrl Pts',(4.65124613749381,0.394380512588343,-8.14723060275528));
#13460=CARTESIAN_POINT('Ctrl Pts',(4.62733914904783,0.456202370662872,-8.14233132241669));
#13461=CARTESIAN_POINT('Ctrl Pts',(4.58531584570611,0.542487404669705,-8.1354028620356));
#13462=CARTESIAN_POINT('Ctrl Pts',(4.57125063138831,0.568782738265171,-8.13327973969102));
#13463=CARTESIAN_POINT('Ctrl Pts',(4.5529786859207,0.600029490407156,-8.13076583666157));
#13464=CARTESIAN_POINT('Ctrl Pts',(4.5497110809275,0.605514564812551,-8.13032490205492));
#13465=CARTESIAN_POINT('Ctrl Pts',(4.54454276796691,0.614031914759355,-8.12964108833851));
#13466=CARTESIAN_POINT('Ctrl Pts',(4.54267263049038,0.617082458691369,-8.12939635403739));
#13467=CARTESIAN_POINT('Ctrl Pts',(4.53918332728128,0.622716380763,-8.12894476272226));
#13468=CARTESIAN_POINT('Ctrl Pts',(4.53756803697222,0.625301989516149,-8.12873767564058));
#13469=CARTESIAN_POINT('Ctrl Pts',(4.5338461826726,0.631208429122032,-8.12826496249736));
#13470=CARTESIAN_POINT('Ctrl Pts',(4.53173301154942,0.634525006115584,-8.12799976961665));
#13471=CARTESIAN_POINT('Ctrl Pts',(4.52510067518684,0.644820164778107,-8.12717712876888));
#13472=CARTESIAN_POINT('Ctrl Pts',(4.52052408291728,0.651761704785397,-8.12662326431956));
#13473=CARTESIAN_POINT('Ctrl Pts',(4.50959642653452,0.667960295516328,-8.12533121790871));
#13474=CARTESIAN_POINT('Ctrl Pts',(4.50318566832801,0.677176300338191,-8.12459646287379));
#13475=CARTESIAN_POINT('Ctrl Pts',(4.47965573977095,0.709991529513571,-8.12197599025489));
#13476=CARTESIAN_POINT('Ctrl Pts',(4.46179255421233,0.733046239508686,-8.12012678473544));
#13477=CARTESIAN_POINT('Ctrl Pts',(4.38267794540693,0.827677232508278,-8.11239186556977));
#13478=CARTESIAN_POINT('Ctrl Pts',(4.31381708871012,0.892428961517595,-8.10670250495221));
#13479=CARTESIAN_POINT('Ctrl Pts',(4.21404835231191,0.965913324493517,-8.09878935867756));
#13480=CARTESIAN_POINT('Ctrl Pts',(4.18946207780677,0.982625136534703,-8.09686488413498));
#13481=CARTESIAN_POINT('Ctrl Pts',(4.15625276492076,1.00340623377441,-8.09428243244944));
#13482=CARTESIAN_POINT('Ctrl Pts',(4.14817390793684,1.00832722883727,-8.09365550825484));
#13483=CARTESIAN_POINT('Ctrl Pts',(4.13494073765065,1.01617083752472,-8.09263026103577));
#13484=CARTESIAN_POINT('Ctrl Pts',(4.12982199816092,1.01915287586252,-8.09223408111743));
#13485=CARTESIAN_POINT('Ctrl Pts',(4.11991668644993,1.02482378287332,-8.09146807789496));
#13486=CARTESIAN_POINT('Ctrl Pts',(4.11513337252015,1.02751805448563,-8.09109845941313));
#13487=CARTESIAN_POINT('Ctrl Pts',(4.10397935484342,1.0336983914267,-8.09023713035922));
#13488=CARTESIAN_POINT('Ctrl Pts',(4.09759495359104,1.03715914011266,-8.08974454451684));
#13489=CARTESIAN_POINT('Ctrl Pts',(4.07697376475947,1.0480915990565,-8.08815463417633));
#13490=CARTESIAN_POINT('Ctrl Pts',(4.06261636887136,1.05533062173797,-8.08704932136377));
#13491=CARTESIAN_POINT('Ctrl Pts',(4.02839318888358,1.07171604991502,-8.08441720446404));
#13492=CARTESIAN_POINT('Ctrl Pts',(4.00841250153652,1.08060725582464,-8.08288242384131));
#13493=CARTESIAN_POINT('Ctrl Pts',(3.89033799969225,1.12925785405858,-8.07382352804963));
#13494=CARTESIAN_POINT('Ctrl Pts',(3.78749306257316,1.15620092709752,-8.06591575437205));
#13495=CARTESIAN_POINT('Ctrl Pts',(3.65399016608896,1.17252468732886,-8.05621716720229));
#13496=CARTESIAN_POINT('Ctrl Pts',(3.62539875270154,1.17496500395357,-8.05417630264844));
#13497=CARTESIAN_POINT('Ctrl Pts',(3.59043539084954,1.17666583411506,-8.05174571652767));
#13498=CARTESIAN_POINT('Ctrl Pts',(3.58412394903756,1.17692198820975,-8.05130954715574));
#13499=CARTESIAN_POINT('Ctrl Pts',(3.574249754385,1.17724319220592,-8.0506315236999));
#13500=CARTESIAN_POINT('Ctrl Pts',(3.57068836230364,1.17734286859734,-8.05038786295831));
#13501=CARTESIAN_POINT('Ctrl Pts',(3.56407672093481,1.17749789370034,-8.04993722490762));
#13502=CARTESIAN_POINT('Ctrl Pts',(3.5610267183482,1.17755755247908,-8.04973002613013));
#13503=CARTESIAN_POINT('Ctrl Pts',(3.55402248454749,1.17766733428773,-8.04925573862796));
#13504=CARTESIAN_POINT('Ctrl Pts',(3.55006820246112,1.17770939385604,-8.04898909433009));
#13505=CARTESIAN_POINT('Ctrl Pts',(3.53768450464758,1.17777873588606,-8.04815732900005));
#13506=CARTESIAN_POINT('Ctrl Pts',(3.52925473588557,1.17773544148328,-8.04759590619492));
#13507=CARTESIAN_POINT('Ctrl Pts',(3.45128289249397,1.17649772056819,-8.04244112333659));
#13508=CARTESIAN_POINT('Ctrl Pts',(3.38196370783951,1.16923549712724,-8.03813430385383));
#13509=CARTESIAN_POINT('Ctrl Pts',(3.2306501769793,1.13967216950146,-8.02859508682647));
#13510=CARTESIAN_POINT('Ctrl Pts',(3.14961756253098,1.1145525457017,-8.0233788516996));
#13511=CARTESIAN_POINT('Ctrl Pts',(3.05930782627813,1.07549189626892,-8.01696511213609));
#13512=CARTESIAN_POINT('Ctrl Pts',(3.0467350499965,1.06978948491779,-8.01605847737323));
#13513=CARTESIAN_POINT('Ctrl Pts',(3.02799590737272,1.06088986949967,-8.01468487936058));
#13514=CARTESIAN_POINT('Ctrl Pts',(3.02175255572325,1.05785684032362,-8.01422345592586));
#13515=CARTESIAN_POINT('Ctrl Pts',(3.01096323863144,1.05249697973298,-8.01341928456777));
#13516=CARTESIAN_POINT('Ctrl Pts',(3.00640487540771,1.05019541682962,-8.01307741052808));
#13517=CARTESIAN_POINT('Ctrl Pts',(2.99702371536533,1.0453819598403,-8.01236935998165));
#13518=CARTESIAN_POINT('Ctrl Pts',(2.99220306726012,1.04286616753549,-8.01200305458771));
#13519=CARTESIAN_POINT('Ctrl Pts',(2.98088294371363,1.03685833125116,-8.01113695637178));
#13520=CARTESIAN_POINT('Ctrl Pts',(2.97439858270958,1.03333844963125,-8.01063619906663));
#13521=CARTESIAN_POINT('Ctrl Pts',(2.96071676443277,1.02574430249559,-8.00956954865645));
#13522=CARTESIAN_POINT('Ctrl Pts',(2.95352832332996,1.0216546980689,-8.0090031338202));
#13523=CARTESIAN_POINT('Ctrl Pts',(2.93405081734917,1.01030048393135,-8.00745172348554));
#13524=CARTESIAN_POINT('Ctrl Pts',(2.92185014566977,1.00288780164954,-8.00646156960118));
#13525=CARTESIAN_POINT('Ctrl Pts',(2.88317667090131,0.978417801883694,-8.00326279267926));
#13526=CARTESIAN_POINT('Ctrl Pts',(2.85725382311953,0.960520995304603,-8.00102578860465));
#13527=CARTESIAN_POINT('Ctrl Pts',(2.7904468856044,0.910328395448378,-7.99501370419639));
#13528=CARTESIAN_POINT('Ctrl Pts',(2.75093575032511,0.876323348329264,-7.99119351040912));
#13529=CARTESIAN_POINT('Ctrl Pts',(2.67128798005187,0.79801339596437,-7.98299678873544));
#13530=CARTESIAN_POINT('Ctrl Pts',(2.63200077614562,0.753035574767279,-7.9786309147343));
#13531=CARTESIAN_POINT('Ctrl Pts',(2.59026036599144,0.697211792060864,-7.97374251517666));
#13532=CARTESIAN_POINT('Ctrl Pts',(2.58433744388942,0.689075067245759,-7.97304228689874));
#13533=CARTESIAN_POINT('Ctrl Pts',(2.57623802634225,0.677643197491073,-7.97207653876398));
#13534=CARTESIAN_POINT('Ctrl Pts',(2.57397290368347,0.67441179860419,-7.9718055305378));
#13535=CARTESIAN_POINT('Ctrl Pts',(2.57009478155914,0.668819723883629,-7.97134001853496));
#13536=CARTESIAN_POINT('Ctrl Pts',(2.56847407562655,0.666464472785826,-7.97114501103933));
#13537=CARTESIAN_POINT('Ctrl Pts',(2.56507464085285,0.661485602260752,-7.97073503515564));
#13538=CARTESIAN_POINT('Ctrl Pts',(2.56329789826379,0.658860661934902,-7.97052020574611));
#13539=CARTESIAN_POINT('Ctrl Pts',(2.55891811024194,0.652333397869032,-7.96998917513778));
#13540=CARTESIAN_POINT('Ctrl Pts',(2.55632770460325,0.64842258228734,-7.96967380038315));
#13541=CARTESIAN_POINT('Ctrl Pts',(2.54666273304519,0.633639989371951,-7.96849175906524));
#13542=CARTESIAN_POINT('Ctrl Pts',(2.53974425220579,0.622666596284655,-7.96763463804521));
#13543=CARTESIAN_POINT('Ctrl Pts',(2.52245579714508,0.594214060390553,-7.9654578137858));
#13544=CARTESIAN_POINT('Ctrl Pts',(2.51235406731231,0.576576279199561,-7.96415151182035));
#13545=CARTESIAN_POINT('Ctrl Pts',(2.45467807658373,0.469541350189625,-7.95642501541004));
#13546=CARTESIAN_POINT('Ctrl Pts',(2.41833834277047,0.374573445293031,-7.95035414576092));
#13547=CARTESIAN_POINT('Ctrl Pts',(2.38650237053188,0.242567533977751,-7.94173392020738));
#13548=CARTESIAN_POINT('Ctrl Pts',(2.37988961134717,0.208676039467854,-7.93950971701043));
#13549=CARTESIAN_POINT('Ctrl Pts',(2.37324383318611,0.16432865133715,-7.93655937948593));
#13550=CARTESIAN_POINT('Ctrl Pts',(2.37184731709931,0.154092504908083,-7.93587571436136));
#13551=CARTESIAN_POINT('Ctrl Pts',(2.36983897146936,0.137771389640783,-7.93478078549251));
#13552=CARTESIAN_POINT('Ctrl Pts',(2.36913954485042,0.131697583349774,-7.93437224945119));
#13553=CARTESIAN_POINT('Ctrl Pts',(2.36791902205137,0.120319733217702,-7.93360483805153));
#13554=CARTESIAN_POINT('Ctrl Pts',(2.3673865737766,0.115017043402438,-7.93324632528428));
#13555=CARTESIAN_POINT('Ctrl Pts',(2.36640123908301,0.104485446871551,-7.9325325108268));
#13556=CARTESIAN_POINT('Ctrl Pts',(2.36594727951419,0.0992567623689709,
-7.93217725115629));
#13557=CARTESIAN_POINT('Ctrl Pts',(2.364995855742,0.0873773763892674,-7.93136807229652));
#13558=CARTESIAN_POINT('Ctrl Pts',(2.36451990884689,0.0807251811422267,
-7.93091349850281));
#13559=CARTESIAN_POINT('Ctrl Pts',(2.36253235015777,0.0491843186856213,
-7.92875104626062));
#13560=CARTESIAN_POINT('Ctrl Pts',(2.36175499908727,0.0242577447497806,
-7.92702086516518));
#13561=CARTESIAN_POINT('Ctrl Pts',(2.36176924264068,-0.000672880918024107,
-7.92526805329864));
#13562=CARTESIAN_POINT('Ctrl Pts',(2.36176924189409,-0.000671572882392571,
-7.92526814526343));
#13563=CARTESIAN_POINT('Ctrl Pts',(2.36182874002516,-0.105014547877794,
-7.91793204682712));
#13564=CARTESIAN_POINT('Ctrl Pts',(2.37575537529407,-0.208883089305192,
-7.91018050052472));
#13565=CARTESIAN_POINT('Ctrl Pts',(2.41340834476088,-0.347111401056375,
-7.89976355597196));
#13566=CARTESIAN_POINT('Ctrl Pts',(2.42550200525097,-0.384159261872818,
-7.8969683755995));
#13567=CARTESIAN_POINT('Ctrl Pts',(2.44176920881263,-0.426712988878862,
-7.8938030358703));
#13568=CARTESIAN_POINT('Ctrl Pts',(2.4441796374853,-0.432862871050662,-7.8933467320813));
#13569=CARTESIAN_POINT('Ctrl Pts',(2.44797872648623,-0.442320754302456,
-7.89264711749572));
#13570=CARTESIAN_POINT('Ctrl Pts',(2.4493309278344,-0.445643115841913,-7.89240176631258));
#13571=CARTESIAN_POINT('Ctrl Pts',(2.45186011309046,-0.451776922058735,
-7.89194962064927));
#13572=CARTESIAN_POINT('Ctrl Pts',(2.45303282899958,-0.454589971599706,
-7.89174259118068));
#13573=CARTESIAN_POINT('Ctrl Pts',(2.45573897904796,-0.461011049293892,
-7.89127075322823));
#13574=CARTESIAN_POINT('Ctrl Pts',(2.45727951827934,-0.464615999352169,
-7.89100637163265));
#13575=CARTESIAN_POINT('Ctrl Pts',(2.46137393663102,-0.47406630868873,-7.89031449689183));
#13576=CARTESIAN_POINT('Ctrl Pts',(2.46395739465777,-0.479898823181687,
-7.88988869613323));
#13577=CARTESIAN_POINT('Ctrl Pts',(2.48611061912444,-0.528835159126472,
-7.88632395785479));
#13578=CARTESIAN_POINT('Ctrl Pts',(2.50821792777159,-0.57074957711135,-7.88332144604226));
#13579=CARTESIAN_POINT('Ctrl Pts',(2.57323889122626,-0.677843567369104,
-7.87549415025452));
#13580=CARTESIAN_POINT('Ctrl Pts',(2.62019810293726,-0.740282602905352,
-7.87075387472766));
#13581=CARTESIAN_POINT('Ctrl Pts',(2.69082968639269,-0.817016525230019,
-7.86416012938778));
#13582=CARTESIAN_POINT('Ctrl Pts',(2.70932318569956,-0.835801604992794,
-7.86247595689157));
#13583=CARTESIAN_POINT('Ctrl Pts',(2.73759518937276,-0.862654597433883,
-7.85994709854885));
#13584=CARTESIAN_POINT('Ctrl Pts',(2.74689935110735,-0.871211126312293,
-7.85912180446637));
#13585=CARTESIAN_POINT('Ctrl Pts',(2.76202758228735,-0.884680784060638,
-7.85778950911532));
#13586=CARTESIAN_POINT('Ctrl Pts',(2.76776489478522,-0.889690166035058,
-7.85728638991197));
#13587=CARTESIAN_POINT('Ctrl Pts',(2.77873227542358,-0.899080131374576,
-7.85632837347067));
#13588=CARTESIAN_POINT('Ctrl Pts',(2.78395262365634,-0.903471621642111,
-7.85587393868121));
#13589=CARTESIAN_POINT('Ctrl Pts',(2.78925201976461,-0.907851556189349,
-7.85541409511517));
#13590=CARTESIAN_POINT('Ctrl Pts',(2.78929330427405,-0.907885672969693,
-7.85541051283117));
#13591=CARTESIAN_POINT('Ctrl Pts',(2.79338483398073,-0.911266370301086,
-7.85505549697381));
#13592=CARTESIAN_POINT('Ctrl Pts',(2.79745736820196,-0.914585766804777,
-7.85470298948713));
#13593=CARTESIAN_POINT('Ctrl Pts',(2.80561374538718,-0.921143435526385,
-7.85399862218538));
#13594=CARTESIAN_POINT('Ctrl Pts',(2.80969714516943,-0.924382069644818,
-7.85364678771651));
#13595=CARTESIAN_POINT('Ctrl Pts',(2.82076433139421,-0.933040655363849,
-7.85269526920025));
#13596=CARTESIAN_POINT('Ctrl Pts',(2.82778775143206,-0.938409165203609,
-7.85209359799435));
#13597=CARTESIAN_POINT('Ctrl Pts',(2.85468645697024,-0.958494114878888,
-7.84979698753703));
#13598=CARTESIAN_POINT('Ctrl Pts',(2.8749618558444,-0.97266141392418,-7.84808144234096));
#13599=CARTESIAN_POINT('Ctrl Pts',(2.97861622030849,-1.0403348019763,-7.83938123253326));
#13600=CARTESIAN_POINT('Ctrl Pts',(3.06805822498817,-1.08380212983403,-7.83204773736348));
#13601=CARTESIAN_POINT('Ctrl Pts',(3.19039147666707,-1.12521655850216,-7.82262609199434));
#13602=CARTESIAN_POINT('Ctrl Pts',(3.21928441327302,-1.133777926907,-7.820446164179));
#13603=CARTESIAN_POINT('Ctrl Pts',(3.25958702226249,-1.14405621165389,-7.81749248755068));
#13604=CARTESIAN_POINT('Ctrl Pts',(3.27073969054687,-1.14672761948898,-7.81668422016562));
#13605=CARTESIAN_POINT('Ctrl Pts',(3.29017712253898,-1.15108431347198,-7.81529322201355));
#13606=CARTESIAN_POINT('Ctrl Pts',(3.29844415787695,-1.15284404849337,-7.81470712391008));
#13607=CARTESIAN_POINT('Ctrl Pts',(3.31061024995569,-1.15529714548863,-7.81385337024948));
#13608=CARTESIAN_POINT('Ctrl Pts',(3.31449478024017,-1.15606003835501,-7.81358208149238));
#13609=CARTESIAN_POINT('Ctrl Pts',(3.32135285214677,-1.15737103549866,-7.81310551690047));
#13610=CARTESIAN_POINT('Ctrl Pts',(3.32432474192281,-1.15792729228806,-7.81289979581226));
#13611=CARTESIAN_POINT('Ctrl Pts',(3.33078937516846,-1.15911154675628,-7.81245403910711));
#13612=CARTESIAN_POINT('Ctrl Pts',(3.33428283308934,-1.15973520731395,-7.81221424560107));
#13613=CARTESIAN_POINT('Ctrl Pts',(3.3439409058313,-1.16141438221933,-7.81155418695836));
#13614=CARTESIAN_POINT('Ctrl Pts',(3.35011130037759,-1.16243661604988,-7.8111357195743));
#13615=CARTESIAN_POINT('Ctrl Pts',(3.38362026596937,-1.16771405678282,-7.80887926711422));
#13616=CARTESIAN_POINT('Ctrl Pts',(3.41109654103612,-1.17105443329986,-7.80708692359229));
#13617=CARTESIAN_POINT('Ctrl Pts',(3.54509038932417,-1.18257073763232,-7.79851598864044));
#13618=CARTESIAN_POINT('Ctrl Pts',(3.65226583812479,-1.17719832191472,-7.79213408930033));
#13619=CARTESIAN_POINT('Ctrl Pts',(3.77881925169055,-1.15339151023154,-7.78393636740898));
#13620=CARTESIAN_POINT('Ctrl Pts',(3.80026544549824,-1.14873312464606,-7.78252558185132));
#13621=CARTESIAN_POINT('Ctrl Pts',(3.8372201260119,-1.13961792888321,-7.78004778766584));
#13622=CARTESIAN_POINT('Ctrl Pts',(3.85279060425364,-1.13543641260057,-7.77898915379222));
#13623=CARTESIAN_POINT('Ctrl Pts',(3.87525051983323,-1.12890756559048,-7.77743842223813));
#13624=CARTESIAN_POINT('Ctrl Pts',(3.88221220231322,-1.12681378713968,-7.77695442311493));
#13625=CARTESIAN_POINT('Ctrl Pts',(3.89439745562673,-1.12302561497784,-7.77610118739983));
#13626=CARTESIAN_POINT('Ctrl Pts',(3.89962944288688,-1.12135887113613,-7.77573285269488));
#13627=CARTESIAN_POINT('Ctrl Pts',(3.90979105090446,-1.1180432579845,-7.77501351975038));
#13628=CARTESIAN_POINT('Ctrl Pts',(3.91472179510634,-1.11639821746324,-7.77466265328197));
#13629=CARTESIAN_POINT('Ctrl Pts',(3.92793970869251,-1.11189087761117,-7.77371708494631));
#13630=CARTESIAN_POINT('Ctrl Pts',(3.93620593906893,-1.10896863646193,-7.77312044018602));
#13631=CARTESIAN_POINT('Ctrl Pts',(3.96716186367784,-1.09763484365831,-7.77086558654179));
#13632=CARTESIAN_POINT('Ctrl Pts',(3.98962178057065,-1.08861747623762,-7.76918772356668));
#13633=CARTESIAN_POINT('Ctrl Pts',(4.03425479370724,-1.06908051436565,-7.76576585230553));
#13634=CARTESIAN_POINT('Ctrl Pts',(4.05639274468124,-1.05855387822235,-7.76402332099047));
#13635=CARTESIAN_POINT('Ctrl Pts',(4.07816960641408,-1.04735411443813,-7.76226461992608));
#13636=CARTESIAN_POINT('Ctrl Pts',(4.07816926754758,-1.04735428871592,-7.66392024962001));
#13637=CARTESIAN_POINT('Ctrl Pts',(4.07599933067676,-1.04847027876743,-7.66408638768524));
#13638=CARTESIAN_POINT('Ctrl Pts',(4.07382593516263,-1.0495795204847,-7.6642520981632));
#13639=CARTESIAN_POINT('Ctrl Pts',(4.06823659364625,-1.05241030673236,-7.66467650685746));
#13640=CARTESIAN_POINT('Ctrl Pts',(4.0648156862231,-1.0541219757116,-7.66493459423372));
#13641=CARTESIAN_POINT('Ctrl Pts',(4.0559518984867,-1.05850315338341,-7.66559917020746));
#13642=CARTESIAN_POINT('Ctrl Pts',(4.0504965571681,-1.06114739960968,-7.666004175306));
#13643=CARTESIAN_POINT('Ctrl Pts',(4.01373074194367,-1.07861879499067,-7.66870842048069));
#13644=CARTESIAN_POINT('Ctrl Pts',(3.9817963483123,-1.09210188638138,-7.67093511289324));
#13645=CARTESIAN_POINT('Ctrl Pts',(3.92285150753164,-1.11397837109124,-7.67490795160055));
#13646=CARTESIAN_POINT('Ctrl Pts',(3.89604682207342,-1.12284444738343,-7.6766652819446));
#13647=CARTESIAN_POINT('Ctrl Pts',(3.8228898202535,-1.14415800566199,-7.68138972842663));
#13648=CARTESIAN_POINT('Ctrl Pts',(3.77605503881949,-1.15474982941892,-7.68433988936288));
#13649=CARTESIAN_POINT('Ctrl Pts',(3.67607140816564,-1.17102187003846,-7.690674660315));
#13650=CARTESIAN_POINT('Ctrl Pts',(3.62292282389914,-1.17600233552378,-7.69406459648467));
#13651=CARTESIAN_POINT('Ctrl Pts',(3.55879719845989,-1.17764201358477,-7.69828058026507));
#13652=CARTESIAN_POINT('Ctrl Pts',(3.54796738261376,-1.17776949020798,-7.69899673981775));
#13653=CARTESIAN_POINT('Ctrl Pts',(3.53091596820103,-1.17773501212722,-7.70013154338773));
#13654=CARTESIAN_POINT('Ctrl Pts',(3.52469460032593,-1.17767313164058,-7.70054709872797));
#13655=CARTESIAN_POINT('Ctrl Pts',(3.51304772995083,-1.17746498323356,-7.70132801185411));
#13656=CARTESIAN_POINT('Ctrl Pts',(3.50762216039025,-1.17733049916599,-7.7016929957926));
#13657=CARTESIAN_POINT('Ctrl Pts',(3.4954772805074,-1.17694545143863,-7.70251278203914));
#13658=CARTESIAN_POINT('Ctrl Pts',(3.48875884144225,-1.17667483660613,-7.70296819202734));
#13659=CARTESIAN_POINT('Ctrl Pts',(3.4716687161671,-1.17583981971684,-7.70413168007832));
#13660=CARTESIAN_POINT('Ctrl Pts',(3.46130168433332,-1.17519572036113,-7.70484218789373));
#13661=CARTESIAN_POINT('Ctrl Pts',(3.37566400039517,-1.16873693410163,-7.71075196532745));
#13662=CARTESIAN_POINT('Ctrl Pts',(3.30111759441655,-1.15583535098057,-7.71617307756693));
#13663=CARTESIAN_POINT('Ctrl Pts',(3.17252192617881,-1.12060544461102,-7.72592684272138));
#13664=CARTESIAN_POINT('Ctrl Pts',(3.11791510789142,-1.10122378340417,-7.73020067207606));
#13665=CARTESIAN_POINT('Ctrl Pts',(3.04624034787487,-1.06966781603221,-7.73585547351368));
#13666=CARTESIAN_POINT('Ctrl Pts',(3.02774391662478,-1.06094270653197,-7.73731849390011));
#13667=CARTESIAN_POINT('Ctrl Pts',(2.99784897382991,-1.04587681761694,-7.73967933610442));
#13668=CARTESIAN_POINT('Ctrl Pts',(2.98631239963288,-1.03982076639324,-7.74058943201842));
#13669=CARTESIAN_POINT('Ctrl Pts',(2.97075501624351,-1.03132177780032,-7.74181308691415));
#13670=CARTESIAN_POINT('Ctrl Pts',(2.96664534557664,-1.02904463271438,-7.74213597893885));
#13671=CARTESIAN_POINT('Ctrl Pts',(2.95978504394658,-1.02518954268339,-7.74267425708184));
#13672=CARTESIAN_POINT('Ctrl Pts',(2.95702699479534,-1.02362499119719,-7.74289046247985));
#13673=CARTESIAN_POINT('Ctrl Pts',(2.95179596606035,-1.0206296100506,-7.74330010015454));
#13674=CARTESIAN_POINT('Ctrl Pts',(2.94932182895659,-1.01920089531999,-7.74349366760424));
#13675=CARTESIAN_POINT('Ctrl Pts',(2.94344852930459,-1.01578074208898,-7.74395280360183));
#13676=CARTESIAN_POINT('Ctrl Pts',(2.94005408435178,-1.01378120800476,-7.7442178630693));
#13677=CARTESIAN_POINT('Ctrl Pts',(2.9280566471667,-1.00663266061807,-7.74515388091924));
#13678=CARTESIAN_POINT('Ctrl Pts',(2.91950914964193,-1.0013906946412,-7.74581924411855));
#13679=CARTESIAN_POINT('Ctrl Pts',(2.86043178839065,-0.964113560823456,
-7.75041510479541));
#13680=CARTESIAN_POINT('Ctrl Pts',(2.81233372185633,-0.928373744823914,
-7.75414444405375));
#13681=CARTESIAN_POINT('Ctrl Pts',(2.71660604837684,-0.845217537616965,
-7.76200080480283));
#13682=CARTESIAN_POINT('Ctrl Pts',(2.66989610621342,-0.797078309952863,
-7.76611179794526));
#13683=CARTESIAN_POINT('Ctrl Pts',(2.60579444269048,-0.718633012873777,
-7.77255201164657));
#13684=CARTESIAN_POINT('Ctrl Pts',(2.58523450023074,-0.691097460731915,
-7.77476919362937));
#13685=CARTESIAN_POINT('Ctrl Pts',(2.56051406242008,-0.654779508937179,
-7.77766441192508));
#13686=CARTESIAN_POINT('Ctrl Pts',(2.55521672100893,-0.646788904696646,
-7.7782996400518));
#13687=CARTESIAN_POINT('Ctrl Pts',(2.54679012290392,-0.633734767313471,
-7.7793350350392));
#13688=CARTESIAN_POINT('Ctrl Pts',(2.54360059546308,-0.628710511846509,
-7.7797329764866));
#13689=CARTESIAN_POINT('Ctrl Pts',(2.53754760353215,-0.619013981839423,
-7.78050002719979));
#13690=CARTESIAN_POINT('Ctrl Pts',(2.53467839516187,-0.614345461357498,
-7.78086891458866));
#13691=CARTESIAN_POINT('Ctrl Pts',(2.52817943998174,-0.603603606680172,
-7.78171682991672));
#13692=CARTESIAN_POINT('Ctrl Pts',(2.52457166297125,-0.597517295623453,
-7.78219663276089));
#13693=CARTESIAN_POINT('Ctrl Pts',(2.51324888297684,-0.57801734272091,-7.78373213218779));
#13694=CARTESIAN_POINT('Ctrl Pts',(2.50574357027402,-0.564484474773569,
-7.78479518406623));
#13695=CARTESIAN_POINT('Ctrl Pts',(2.46146197049144,-0.480793522645426,
-7.79135685972649));
#13696=CARTESIAN_POINT('Ctrl Pts',(2.43158085101455,-0.407232425315046,
-7.79709156562835));
#13697=CARTESIAN_POINT('Ctrl Pts',(2.39398850534059,-0.278966808632871,
-7.80689404753544));
#13698=CARTESIAN_POINT('Ctrl Pts',(2.38231188412581,-0.225687427177136,
-7.81090641336049));
#13699=CARTESIAN_POINT('Ctrl Pts',(2.37197344526455,-0.155567315329824,
-7.81599157449511));
#13700=CARTESIAN_POINT('Ctrl Pts',(2.3699206223463,-0.139296458171391,-7.81715778788155));
#13701=CARTESIAN_POINT('Ctrl Pts',(2.36705077574876,-0.111964492097584,
-7.8190884161107));
#13702=CARTESIAN_POINT('Ctrl Pts',(2.36604899329987,-0.100925466978323,
-7.81986044562139));
#13703=CARTESIAN_POINT('Ctrl Pts',(2.36486648113425,-0.0854743775618568,
-7.82092877814227));
#13704=CARTESIAN_POINT('Ctrl Pts',(2.36455452284292,-0.0810733510683677,
-7.82123168941661));
#13705=CARTESIAN_POINT('Ctrl Pts',(2.36406449451421,-0.0735619093196238,
-7.8217461985763));
#13706=CARTESIAN_POINT('Ctrl Pts',(2.36387402275671,-0.0704523764723134,
-7.82195846468412));
#13707=CARTESIAN_POINT('Ctrl Pts',(2.36352888200818,-0.0644260593539233,
-7.82236839152458));
#13708=CARTESIAN_POINT('Ctrl Pts',(2.36337272274075,-0.0615094275918239,
-7.82256613781282));
#13709=CARTESIAN_POINT('Ctrl Pts',(2.36297689330821,-0.0535627928466335,
-7.82310321623733));
#13710=CARTESIAN_POINT('Ctrl Pts',(2.36275862647741,-0.0485317129067095,
-7.82344139072724));
#13711=CARTESIAN_POINT('Ctrl Pts',(2.36204278491587,-0.0291634094983746,
-7.82473666981689));
#13712=CARTESIAN_POINT('Ctrl Pts',(2.36177488286253,-0.0148182653979148,
-7.8256821052238));
#13713=CARTESIAN_POINT('Ctrl Pts',(2.36175953056197,0.0235664998942394,
-7.82818322953387));
#13714=CARTESIAN_POINT('Ctrl Pts',(2.36248581951748,0.0476002929455243,
-7.82971921949145));
#13715=CARTESIAN_POINT('Ctrl Pts',(2.36721770908896,0.125295133830403,-7.83463471318658));
#13716=CARTESIAN_POINT('Ctrl Pts',(2.37416376763856,0.178708983497501,-7.83793899574084));
#13717=CARTESIAN_POINT('Ctrl Pts',(2.39924636467484,0.303847515676125,-7.8458443064072));
#13718=CARTESIAN_POINT('Ctrl Pts',(2.42052633574254,0.374697597684427,-7.85046048557332));
#13719=CARTESIAN_POINT('Ctrl Pts',(2.45221963643209,0.452751468272571,-7.85598885609869));
#13720=CARTESIAN_POINT('Ctrl Pts',(2.45627278956272,0.462365044837467,-7.8566775111369));
#13721=CARTESIAN_POINT('Ctrl Pts',(2.46315287194618,0.4780965498791,-7.85781790304939));
#13722=CARTESIAN_POINT('Ctrl Pts',(2.46590560098539,0.484246444690515,-7.85826715151437));
#13723=CARTESIAN_POINT('Ctrl Pts',(2.47097103731202,0.495307654249576,-7.85908156578698));
#13724=CARTESIAN_POINT('Ctrl Pts',(2.47326523502905,0.500227276499942,-7.85944609530074));
#13725=CARTESIAN_POINT('Ctrl Pts',(2.47825746934426,0.510742110613748,-7.86023026781283));
#13726=CARTESIAN_POINT('Ctrl Pts',(2.48096591681059,0.516332168081663,-7.86065025855924));
#13727=CARTESIAN_POINT('Ctrl Pts',(2.48849712075084,0.531567736380428,-7.86180358602152));
#13728=CARTESIAN_POINT('Ctrl Pts',(2.49340823500583,0.541168646053145,-7.86253994584183));
#13729=CARTESIAN_POINT('Ctrl Pts',(2.52292407524643,0.596966702556771,-7.86687715304661));
#13730=CARTESIAN_POINT('Ctrl Pts',(2.55045113486666,0.641543335113617,-7.87057981786423));
#13731=CARTESIAN_POINT('Ctrl Pts',(2.62580475670246,0.747135358210077,-7.87994864816813));
#13732=CARTESIAN_POINT('Ctrl Pts',(2.67685913574037,0.805544453025278,-7.88569208628232));
#13733=CARTESIAN_POINT('Ctrl Pts',(2.75847135023436,0.882187427319258,-7.89380896596216));
#13734=CARTESIAN_POINT('Ctrl Pts',(2.7847038771568,0.90473460964183,-7.89628223371594));
#13735=CARTESIAN_POINT('Ctrl Pts',(2.81665755169725,0.929840325062126,-7.89910667328438));
#13736=CARTESIAN_POINT('Ctrl Pts',(2.82145101250359,0.933547038574874,-7.89952561743558));
#13737=CARTESIAN_POINT('Ctrl Pts',(2.82931621212083,0.939532658226551,-7.90020502900419));
#13738=CARTESIAN_POINT('Ctrl Pts',(2.83237074928425,0.941833832818596,-7.90046694398928));
#13739=CARTESIAN_POINT('Ctrl Pts',(2.83787460027423,0.945938358664749,-7.90093532457074));
#13740=CARTESIAN_POINT('Ctrl Pts',(2.84031973216837,0.947747132313531,-7.90114215336278));
#13741=CARTESIAN_POINT('Ctrl Pts',(2.84572405890346,0.951712655999637,-7.90159653939135));
#13742=CARTESIAN_POINT('Ctrl Pts',(2.84868631857519,0.953865088661074,-7.90184380475498));
#13743=CARTESIAN_POINT('Ctrl Pts',(2.85730859327204,0.960068957483658,-7.90255848385646));
#13744=CARTESIAN_POINT('Ctrl Pts',(2.86299466400094,0.96408416195213,-7.90302353375881));
#13745=CARTESIAN_POINT('Ctrl Pts',(2.91174891292745,0.997868088427713,-7.90696117643822));
#13746=CARTESIAN_POINT('Ctrl Pts',(2.95672821372755,1.02478894607964,-7.91026625506025));
#13747=CARTESIAN_POINT('Ctrl Pts',(3.07778011709415,1.08668269577411,-7.91873437274206));
#13748=CARTESIAN_POINT('Ctrl Pts',(3.15604029988409,1.11670307393626,-7.92382090397586));
#13749=CARTESIAN_POINT('Ctrl Pts',(3.26615393099711,1.14598778583277,-7.93109212874473));
#13750=CARTESIAN_POINT('Ctrl Pts',(3.29577775326035,1.15265191106773,-7.9330566735109));
#13751=CARTESIAN_POINT('Ctrl Pts',(3.33498931899542,1.15989368099631,-7.93568483420892));
#13752=CARTESIAN_POINT('Ctrl Pts',(3.34437498356216,1.16150959817997,-7.93631593813377));
#13753=CARTESIAN_POINT('Ctrl Pts',(3.35964207183885,1.16394784572987,-7.93734627241968));
#13754=CARTESIAN_POINT('Ctrl Pts',(3.36551205663904,1.16483985119583,-7.93774331825712));
#13755=CARTESIAN_POINT('Ctrl Pts',(3.37681647861515,1.16647032199944,-7.93850978710612));
#13756=CARTESIAN_POINT('Ctrl Pts',(3.3822498335401,1.16721528890515,-7.93887899660334));
#13757=CARTESIAN_POINT('Ctrl Pts',(3.39485552970633,1.1688540406299,-7.93973756413188));
#13758=CARTESIAN_POINT('Ctrl Pts',(3.4020312274163,1.16971979423164,-7.94022778046154));
#13759=CARTESIAN_POINT('Ctrl Pts',(3.42500715009868,1.17227752349685,-7.94180239726834));
#13760=CARTESIAN_POINT('Ctrl Pts',(3.44083325407097,1.17371573999058,-7.94289457308637));
#13761=CARTESIAN_POINT('Ctrl Pts',(3.4781640898054,1.17634789247088,-7.94548982727891));
#13762=CARTESIAN_POINT('Ctrl Pts',(3.49968146617711,1.17727297668321,-7.94700058425828));
#13763=CARTESIAN_POINT('Ctrl Pts',(3.58163396158158,1.17854707806411,-7.9528113677481));
#13764=CARTESIAN_POINT('Ctrl Pts',(3.64203331349611,1.17483455253705,-7.95721757077947));
#13765=CARTESIAN_POINT('Ctrl Pts',(3.77007661815412,1.15701335510924,-7.96670291533719));
#13766=CARTESIAN_POINT('Ctrl Pts',(3.83732106760747,1.14155700509463,-7.9717730964071));
#13767=CARTESIAN_POINT('Ctrl Pts',(3.91221756712543,1.11726817856383,-7.97729251785475));
#13768=CARTESIAN_POINT('Ctrl Pts',(3.92156258616551,1.11410731971923,-7.97797866728605));
#13769=CARTESIAN_POINT('Ctrl Pts',(3.93455737876684,1.10952921977917,-7.9789282201923));
#13770=CARTESIAN_POINT('Ctrl Pts',(3.93824116220082,1.10821074217709,-7.97919688277755));
#13771=CARTESIAN_POINT('Ctrl Pts',(3.94459701224662,1.10590009981054,-7.97965944301357));
#13772=CARTESIAN_POINT('Ctrl Pts',(3.94727214522463,1.1049165579523,-7.97985383021229));
#13773=CARTESIAN_POINT('Ctrl Pts',(3.95292321249396,1.10281556289205,-7.98026378504648));
#13774=CARTESIAN_POINT('Ctrl Pts',(3.95589824469661,1.10169575383819,-7.98047920691228));
#13775=CARTESIAN_POINT('Ctrl Pts',(3.96329475408134,1.09887744957494,-7.98101387400011));
#13776=CARTESIAN_POINT('Ctrl Pts',(3.96771064635915,1.09716427907276,-7.98133226735685));
#13777=CARTESIAN_POINT('Ctrl Pts',(3.98449314698845,1.09053665509096,-7.98253963907799));
#13778=CARTESIAN_POINT('Ctrl Pts',(3.99678703457802,1.08543916003456,-7.98341853533375));
#13779=CARTESIAN_POINT('Ctrl Pts',(4.02830534967419,1.07173992397506,-7.98566393577523));
#13780=CARTESIAN_POINT('Ctrl Pts',(4.04739077121115,1.0628287411521,-7.98701595004106));
#13781=CARTESIAN_POINT('Ctrl Pts',(4.10750138849634,1.03277320498155,-7.99128104343455));
#13782=CARTESIAN_POINT('Ctrl Pts',(4.14752851994361,1.00972738002557,-7.99413271592813));
#13783=CARTESIAN_POINT('Ctrl Pts',(4.25290974355454,0.94050926715765,-8.00193140006753));
#13784=CARTESIAN_POINT('Ctrl Pts',(4.31506883090708,0.889946346859065,-8.00687724209208));
#13785=CARTESIAN_POINT('Ctrl Pts',(4.38256396026648,0.822562594487059,-8.01309271023972));
#13786=CARTESIAN_POINT('Ctrl Pts',(4.39328537825723,0.811428963784638,-8.01410843621434));
#13787=CARTESIAN_POINT('Ctrl Pts',(4.40858845543719,0.794898386246554,-8.01560251117703));
#13788=CARTESIAN_POINT('Ctrl Pts',(4.41334576605828,0.789665715719755,-8.0160734712462));
#13789=CARTESIAN_POINT('Ctrl Pts',(4.4217048081552,0.780303385651714,-8.01691282204701));
#13790=CARTESIAN_POINT('Ctrl Pts',(4.42532541798199,0.776190802746072,-8.01728041734379));
#13791=CARTESIAN_POINT('Ctrl Pts',(4.43281933305807,0.76755788195842,-8.01804985402368));
#13792=CARTESIAN_POINT('Ctrl Pts',(4.43668731889776,0.76303315321934,-8.01845189782744));
#13793=CARTESIAN_POINT('Ctrl Pts',(4.44669937561324,0.751139777104453,-8.01950559893049));
#13794=CARTESIAN_POINT('Ctrl Pts',(4.45278789644545,0.743725159317698,-8.02015945827958));
#13795=CARTESIAN_POINT('Ctrl Pts',(4.48030824730135,0.709363241103852,-8.02317657984523));
#13796=CARTESIAN_POINT('Ctrl Pts',(4.50064059136776,0.6815610655869,-8.02558205634847));
#13797=CARTESIAN_POINT('Ctrl Pts',(4.55700565228999,0.59694100733188,-8.03280607622727));
#13798=CARTESIAN_POINT('Ctrl Pts',(4.58942083239077,0.53788655892917,-8.03773320938785));
#13799=CARTESIAN_POINT('Ctrl Pts',(4.64067044636245,0.422014935357697,-8.04703071292563));
#13800=CARTESIAN_POINT('Ctrl Pts',(4.66057277854912,0.365883808944387,-8.05138389697688));
#13801=CARTESIAN_POINT('Ctrl Pts',(4.67877465897564,0.298817754867696,-8.05625697026201));
#13802=CARTESIAN_POINT('Ctrl Pts',(4.68127492668306,0.289117498343914,-8.05695388311472));
#13803=CARTESIAN_POINT('Ctrl Pts',(4.684585386014,0.275560622657904,-8.05791579648316));
#13804=CARTESIAN_POINT('Ctrl Pts',(4.68550036337036,0.271730383196766,-8.05818623119838));
#13805=CARTESIAN_POINT('Ctrl Pts',(4.68704589542861,0.26511386703647,-8.05865100584461));
#13806=CARTESIAN_POINT('Ctrl Pts',(4.68768554875982,0.262329782991995,-8.05884584610375));
#13807=CARTESIAN_POINT('Ctrl Pts',(4.68901394454091,0.256450010983176,-8.05925576227636));
#13808=CARTESIAN_POINT('Ctrl Pts',(4.68970032442039,0.253353818048499,-8.05947069770028));
#13809=CARTESIAN_POINT('Ctrl Pts',(4.69137297357451,0.245661751955655,-8.06000247890595));
#13810=CARTESIAN_POINT('Ctrl Pts',(4.69234426483084,0.241062613330397,-8.06031849275867));
#13811=CARTESIAN_POINT('Ctrl Pts',(4.69590685177904,0.223679366779489,-8.06150602657403));
#13812=CARTESIAN_POINT('Ctrl Pts',(4.69831335624334,0.21085776671871,-8.06236788525131));
#13813=CARTESIAN_POINT('Ctrl Pts',(4.70394966352988,0.17780856618879,-8.0645596114501));
#13814=CARTESIAN_POINT('Ctrl Pts',(4.70686583482621,0.157531341017235,-8.06587584425933));
#13815=CARTESIAN_POINT('Ctrl Pts',(4.71598751525121,0.0797549411841474,
-8.07085079217485));
#13816=CARTESIAN_POINT('Ctrl Pts',(4.71848471588639,0.0219011894639412,
-8.07440147699045));
#13817=CARTESIAN_POINT('Ctrl Pts',(4.71442086586518,-0.111339375009466,
-8.08265544155528));
#13818=CARTESIAN_POINT('Ctrl Pts',(4.70487551711657,-0.186367459087978,
-8.08736880221026));
#13819=CARTESIAN_POINT('Ctrl Pts',(4.68592773817508,-0.270092730762107,
-8.09300270423713));
#13820=CARTESIAN_POINT('Ctrl Pts',(4.68350106420552,-0.280192975495403,
-8.09368841499957));
#13821=CARTESIAN_POINT('Ctrl Pts',(4.67928400458495,-0.296776220448255,
-8.09482493340234));
#13822=CARTESIAN_POINT('Ctrl Pts',(4.67757108937437,-0.303278468161848,
-8.09527328216385));
#13823=CARTESIAN_POINT('Ctrl Pts',(4.6743751683658,-0.315001760738158,-8.09608673391792));
#13824=CARTESIAN_POINT('Ctrl Pts',(4.67291156205078,-0.32022793538717,-8.09645120746891));
#13825=CARTESIAN_POINT('Ctrl Pts',(4.66969272935793,-0.331423031053153,
-8.09723600381042));
#13826=CARTESIAN_POINT('Ctrl Pts',(4.66792622881616,-0.337388510854894,
-8.09765667960181));
#13827=CARTESIAN_POINT('Ctrl Pts',(4.66295547830574,-0.353698936619533,
-8.09881383808323));
#13828=CARTESIAN_POINT('Ctrl Pts',(4.65965574201968,-0.364013906078497,
-8.09955337760108));
#13829=CARTESIAN_POINT('Ctrl Pts',(4.63927153071905,-0.424831620805284,
-8.10396102536625));
#13830=CARTESIAN_POINT('Ctrl Pts',(4.61891845833394,-0.474165448162224,
-8.10773496713708));
#13831=CARTESIAN_POINT('Ctrl Pts',(4.57403179429686,-0.56496106664072,-8.11505531157072));
#13832=CARTESIAN_POINT('Ctrl Pts',(4.55015814282189,-0.606634827725838,
-8.11857938297091));
#13833=CARTESIAN_POINT('Ctrl Pts',(4.50830751646034,-0.670329060104568,
-8.12417104878833));
#13834=CARTESIAN_POINT('Ctrl Pts',(4.49196037929793,-0.693359755237035,
-8.12623879928793));
#13835=CARTESIAN_POINT('Ctrl Pts',(4.45374840689439,-0.743289761903298,
-8.13079737101257));
#13836=CARTESIAN_POINT('Ctrl Pts',(4.43149023323762,-0.769859007028095,
-8.13327577408438));
#13837=CARTESIAN_POINT('Ctrl Pts',(4.40399676309858,-0.799881300427521,
-8.13610527621456));
#13838=CARTESIAN_POINT('Ctrl Pts',(4.39986813103883,-0.804320380095369,
-8.13652441753216));
#13839=CARTESIAN_POINT('Ctrl Pts',(4.39307871316497,-0.811508223019384,
-8.13720408363009));
#13840=CARTESIAN_POINT('Ctrl Pts',(4.39043854757939,-0.814276184280567,
-8.13746605772801));
#13841=CARTESIAN_POINT('Ctrl Pts',(4.38567496250284,-0.81922187805559,-8.13793450010119));
#13842=CARTESIAN_POINT('Ctrl Pts',(4.38355655686312,-0.82140428620393,-8.13814133201844));
#13843=CARTESIAN_POINT('Ctrl Pts',(4.37886965662658,-0.826195512214695,
-8.13859567281474));
#13844=CARTESIAN_POINT('Ctrl Pts',(4.37629744082877,-0.828800573599379,
-8.13884289021091));
#13845=CARTESIAN_POINT('Ctrl Pts',(4.36880199642375,-0.836321264907127,
-8.13955729033005));
#13846=CARTESIAN_POINT('Ctrl Pts',(4.36384720477366,-0.841205422225085,
-8.14002211204946));
#13847=CARTESIAN_POINT('Ctrl Pts',(4.3213771798022,-0.882334385032535,-8.14394688501801));
#13848=CARTESIAN_POINT('Ctrl Pts',(4.28153026818175,-0.916098748325419,
-8.14724055042111));
#13849=CARTESIAN_POINT('Ctrl Pts',(4.18853051777139,-0.98483881953171,-8.15444442903269));
#13850=CARTESIAN_POINT('Ctrl Pts',(4.13455216629061,-1.01835679177162,-8.15832338762119));
#13851=CARTESIAN_POINT('Ctrl Pts',(4.07816915725551,-1.04735434543869,-8.16230176652656));
#13852=CARTESIAN_POINT('Origin',(3.53951905042299,8.32667268468867E-16,
0.924367114736157));
#13853=CARTESIAN_POINT('',(4.07816926754758,-1.04735428871592,-8.76047541727166));
#13854=CARTESIAN_POINT('',(4.0781691574206,-1.04735434535379,-8.66209739867239));
#13855=CARTESIAN_POINT('',(4.07816926754759,-1.04735428871592,0.924367114736157));
#13856=CARTESIAN_POINT('Ctrl Pts',(4.07816926754756,-1.04735428871593,-8.76047541727166));
#13857=CARTESIAN_POINT('Ctrl Pts',(4.07894167719801,-1.04695704145165,-8.76041663737559));
#13858=CARTESIAN_POINT('Ctrl Pts',(4.07971365089275,-1.04655893792941,-8.76035790996024));
#13859=CARTESIAN_POINT('Ctrl Pts',(4.08398913035627,-1.04434810052881,-8.76003275863783));
#13860=CARTESIAN_POINT('Ctrl Pts',(4.08748401095802,-1.0425185975108,-8.759767356016));
#13861=CARTESIAN_POINT('Ctrl Pts',(4.09985431291982,-1.03596358879242,-8.75882908017515));
#13862=CARTESIAN_POINT('Ctrl Pts',(4.10867863906273,-1.0311418635942,-8.75816183669268));
#13863=CARTESIAN_POINT('Ctrl Pts',(4.1694784759547,-0.996901684785136,-8.75357135667992));
#13864=CARTESIAN_POINT('Ctrl Pts',(4.21921901049277,-0.963676110532028,
-8.74984838855954));
#13865=CARTESIAN_POINT('Ctrl Pts',(4.31895738292415,-0.885471935464067,
-8.74199558192822));
#13866=CARTESIAN_POINT('Ctrl Pts',(4.36805845418722,-0.839706212042074,
-8.73788191574333));
#13867=CARTESIAN_POINT('Ctrl Pts',(4.43605213722485,-0.76452887931233,-8.73143801305769));
#13868=CARTESIAN_POINT('Ctrl Pts',(4.457974851502,-0.738047814722179,-8.72921998365108));
#13869=CARTESIAN_POINT('Ctrl Pts',(4.48449317042756,-0.703001369460029,
-8.72632374268465));
#13870=CARTESIAN_POINT('Ctrl Pts',(4.49018542063203,-0.695284442914425,
-8.72568837469458));
#13871=CARTESIAN_POINT('Ctrl Pts',(4.49925722358364,-0.682666192611757,
-8.72465276782382));
#13872=CARTESIAN_POINT('Ctrl Pts',(4.50269503310349,-0.677807137572368,
-8.72425475547095));
#13873=CARTESIAN_POINT('Ctrl Pts',(4.5092272003606,-0.6684244183521,-8.72348757848482));
#13874=CARTESIAN_POINT('Ctrl Pts',(4.51232711057117,-0.663904793983033,
-8.72311863587933));
#13875=CARTESIAN_POINT('Ctrl Pts',(4.51935687410455,-0.653500553125249,
-8.72227060757938));
#13876=CARTESIAN_POINT('Ctrl Pts',(4.52326543196141,-0.647601873592266,
-8.72179074686709));
#13877=CARTESIAN_POINT('Ctrl Pts',(4.53555170613786,-0.628691885618473,
-8.72025511476989));
#13878=CARTESIAN_POINT('Ctrl Pts',(4.54372594391739,-0.615550983984805,
-8.71919198728));
#13879=CARTESIAN_POINT('Ctrl Pts',(4.59213721494029,-0.534193211276483,
-8.71263113727757));
#13880=CARTESIAN_POINT('Ctrl Pts',(4.62566054368773,-0.462233565168181,
-8.70689742218396));
#13881=CARTESIAN_POINT('Ctrl Pts',(4.66163295506535,-0.358978655410027,
-8.69887849644065));
#13882=CARTESIAN_POINT('Ctrl Pts',(4.67046026857206,-0.330117072024171,
-8.69666078823665));
#13883=CARTESIAN_POINT('Ctrl Pts',(4.68916829934652,-0.259334424213223,
-8.69131246159671));
#13884=CARTESIAN_POINT('Ctrl Pts',(4.69787857338737,-0.217144464822941,
-8.68819929075556));
#13885=CARTESIAN_POINT('Ctrl Pts',(4.7056571047478,-0.165245198072979,-8.6845260584898));
#13886=CARTESIAN_POINT('Ctrl Pts',(4.70694250689332,-0.155905177983892,
-8.68387115598234));
#13887=CARTESIAN_POINT('Ctrl Pts',(4.70863041020275,-0.142445791302384,
-8.68293718217323));
#13888=CARTESIAN_POINT('Ctrl Pts',(4.70912353458231,-0.13833845077449,-8.68265347108429));
#13889=CARTESIAN_POINT('Ctrl Pts',(4.70994507827246,-0.131177017952631,
-8.68216117263583));
#13890=CARTESIAN_POINT('Ctrl Pts',(4.71028320604943,-0.1281241175152,-8.68195205983454));
#13891=CARTESIAN_POINT('Ctrl Pts',(4.71097610655518,-0.12163614907077,-8.68150928370947));
#13892=CARTESIAN_POINT('Ctrl Pts',(4.71132771837084,-0.11820081901649,-8.68127579450919));
#13893=CARTESIAN_POINT('Ctrl Pts',(4.71224767154721,-0.108804847567738,
-8.68063967238852));
#13894=CARTESIAN_POINT('Ctrl Pts',(4.71278568541892,-0.102841239845358,
-8.68023866821042));
#13895=CARTESIAN_POINT('Ctrl Pts',(4.71517480988392,-0.0738936653030591,
-8.67830433912641));
#13896=CARTESIAN_POINT('Ctrl Pts',(4.71639629805474,-0.0508610995218777,
-8.6768023856533));
#13897=CARTESIAN_POINT('Ctrl Pts',(4.71745525039126,-0.0060202718215907,
-8.67392477403572));
#13898=CARTESIAN_POINT('Ctrl Pts',(4.71736502113479,0.0157763560118024,
-8.67254728714376));
#13899=CARTESIAN_POINT('Ctrl Pts',(4.7148086565318,0.095896599358694,-8.66752294070916));
#13900=CARTESIAN_POINT('Ctrl Pts',(4.70861320325548,0.154016299215415,-8.66395071123672));
#13901=CARTESIAN_POINT('Ctrl Pts',(4.6880366002948,0.266769587040108,-8.65681838791266));
#13902=CARTESIAN_POINT('Ctrl Pts',(4.67398969918011,0.321300173780052,-8.65327149184867));
#13903=CARTESIAN_POINT('Ctrl Pts',(4.65150784642783,0.388309994217652,-8.64865740279191));
#13904=CARTESIAN_POINT('Ctrl Pts',(4.64666167768181,0.401919030822529,-8.6477069097239));
#13905=CARTESIAN_POINT('Ctrl Pts',(4.63911134223433,0.421948224718169,-8.64628634151834));
#13906=CARTESIAN_POINT('Ctrl Pts',(4.63659843747045,0.428439409467722,-8.64582253941805));
#13907=CARTESIAN_POINT('Ctrl Pts',(4.63201559574652,0.439972800833869,-8.64499217235558));
#13908=CARTESIAN_POINT('Ctrl Pts',(4.62996790100747,0.445023673047537,-8.64462635417326));
#13909=CARTESIAN_POINT('Ctrl Pts',(4.62556499293986,0.455671087806128,-8.643850502281));
#13910=CARTESIAN_POINT('Ctrl Pts',(4.62320141649993,0.461263977124023,-8.64344019750508));
#13911=CARTESIAN_POINT('Ctrl Pts',(4.61677645067952,0.476145275539295,-8.64234093869668));
#13912=CARTESIAN_POINT('Ctrl Pts',(4.61263828065911,0.485399769653717,-8.64164942092564));
#13913=CARTESIAN_POINT('Ctrl Pts',(4.5931399703854,0.527536911875695,-8.6384636009424));
#13914=CARTESIAN_POINT('Ctrl Pts',(4.57638593150609,0.559748891316038,-8.63592248768897));
#13915=CARTESIAN_POINT('Ctrl Pts',(4.51438768266219,0.666585653805986,-8.62712293548962));
#13916=CARTESIAN_POINT('Ctrl Pts',(4.46235688783584,0.736934511634343,-8.62065725483451));
#13917=CARTESIAN_POINT('Ctrl Pts',(4.38366152179544,0.821785405833363,-8.61222595943785));
#13918=CARTESIAN_POINT('Ctrl Pts',(4.36352192276271,0.84197817567143,-8.610166217067));
#13919=CARTESIAN_POINT('Ctrl Pts',(4.33064279840472,0.872633135757097,-8.60697707828644));
#13920=CARTESIAN_POINT('Ctrl Pts',(4.31838329929547,0.88359262320473,-8.60582335619578));
#13921=CARTESIAN_POINT('Ctrl Pts',(4.30200769432815,0.89762596551128,-8.6043322671962));
#13922=CARTESIAN_POINT('Ctrl Pts',(4.29809600262463,0.900934135244649,-8.60397972049204));
#13923=CARTESIAN_POINT('Ctrl Pts',(4.29165809790856,0.906307099519065,-8.60340558557649));
#13924=CARTESIAN_POINT('Ctrl Pts',(4.28914472176671,0.908387064479045,-8.60318294228608));
#13925=CARTESIAN_POINT('Ctrl Pts',(4.28420992744763,0.912436464380075,-8.6027487822397));
#13926=CARTESIAN_POINT('Ctrl Pts',(4.28178927734339,0.914406755466843,-8.60253720798839));
#13927=CARTESIAN_POINT('Ctrl Pts',(4.27635221284621,0.91879644372195,-8.60206502421522));
#13928=CARTESIAN_POINT('Ctrl Pts',(4.273331630036,0.921210678016675,-8.601804775349));
#13929=CARTESIAN_POINT('Ctrl Pts',(4.26277643591755,0.929562174448172,-8.6009023308121));
#13930=CARTESIAN_POINT('Ctrl Pts',(4.25518097830398,0.935422418612936,-8.60026522035512));
#13931=CARTESIAN_POINT('Ctrl Pts',(4.18779171641593,0.986114964937178,-8.59471113198653));
#13932=CARTESIAN_POINT('Ctrl Pts',(4.12391952051061,1.02526068021109,-8.59011404178723));
#13933=CARTESIAN_POINT('Ctrl Pts',(3.98419860014707,1.09356227255585,-8.58049395013948));
#13934=CARTESIAN_POINT('Ctrl Pts',(3.90819144645325,1.12147079937742,-8.57548379790194));
#13935=CARTESIAN_POINT('Ctrl Pts',(3.81718319798797,1.1446268999476,-8.56933940746492));
#13936=CARTESIAN_POINT('Ctrl Pts',(3.80438129615286,1.14765678108192,-8.56847239334271));
#13937=CARTESIAN_POINT('Ctrl Pts',(3.78497916224747,1.1519068505908,-8.56715306498016));
#13938=CARTESIAN_POINT('Ctrl Pts',(3.77841456375193,1.15328616982992,-8.56670576975186));
#13939=CARTESIAN_POINT('Ctrl Pts',(3.76651837175313,1.15567980945034,-8.56589338864939));
#13940=CARTESIAN_POINT('Ctrl Pts',(3.76119083263706,1.15671350521278,-8.56552892385501));
#13941=CARTESIAN_POINT('Ctrl Pts',(3.7497274030358,1.15885563704338,-8.56474320543117));
#13942=CARTESIAN_POINT('Ctrl Pts',(3.74358949686853,1.15995223579348,-8.56432159203344));
#13943=CARTESIAN_POINT('Ctrl Pts',(3.72698567308032,1.1627828118813,-8.56317846307211));
#13944=CARTESIAN_POINT('Ctrl Pts',(3.71650477115154,1.16442416846699,-8.56245408256723));
#13945=CARTESIAN_POINT('Ctrl Pts',(3.66188692833145,1.17222314980592,-8.55866363262338));
#13946=CARTESIAN_POINT('Ctrl Pts',(3.61745397904909,1.17601287359168,-8.55552523033936));
#13947=CARTESIAN_POINT('Ctrl Pts',(3.49311547712419,1.17954029340672,-8.54659387911479));
#13948=CARTESIAN_POINT('Ctrl Pts',(3.41329264872653,1.1736838088619,-8.54067565904613));
#13949=CARTESIAN_POINT('Ctrl Pts',(3.30793374917549,1.15507632667367,-8.53289016369807));
#13950=CARTESIAN_POINT('Ctrl Pts',(3.28135107368906,1.1494270584444,-8.53093017990873));
#13951=CARTESIAN_POINT('Ctrl Pts',(3.24458715709001,1.14027412442777,-8.52824472074925));
#13952=CARTESIAN_POINT('Ctrl Pts',(3.23422374128349,1.13754327076715,-8.52749057441487));
#13953=CARTESIAN_POINT('Ctrl Pts',(3.21617134511942,1.13252181223845,-8.52618354332796));
#13954=CARTESIAN_POINT('Ctrl Pts',(3.2084659351522,1.13029342977862,-8.52562779253115));
#13955=CARTESIAN_POINT('Ctrl Pts',(3.19707144198659,1.12687165243393,-8.52480974476516));
#13956=CARTESIAN_POINT('Ctrl Pts',(3.1933647098405,1.12573853943016,-8.52454422298092));
#13957=CARTESIAN_POINT('Ctrl Pts',(3.187034327676,1.12376917767997,-8.52409186432015));
#13958=CARTESIAN_POINT('Ctrl Pts',(3.18440794368603,1.12294200514727,-8.52390451583051));
#13959=CARTESIAN_POINT('Ctrl Pts',(3.17844858026903,1.12104212087132,-8.52348017499062));
#13960=CARTESIAN_POINT('Ctrl Pts',(3.17511746500235,1.11996375232857,-8.52324351250845));
#13961=CARTESIAN_POINT('Ctrl Pts',(3.16604682836266,1.1169825976276,-8.52260040581994));
#13962=CARTESIAN_POINT('Ctrl Pts',(3.1603169758199,1.11505040895927,-8.52219561238292));
#13963=CARTESIAN_POINT('Ctrl Pts',(3.13130028363809,1.10501602206794,-8.52015186246492));
#13964=CARTESIAN_POINT('Ctrl Pts',(3.10825526564424,1.09622749524947,-8.51854895746084));
#13965=CARTESIAN_POINT('Ctrl Pts',(2.98417627878229,1.04438893918088,-8.50994256029602));
#13966=CARTESIAN_POINT('Ctrl Pts',(2.88926500168818,0.98809287574705,-8.50339777767256));
#13967=CARTESIAN_POINT('Ctrl Pts',(2.77743761387999,0.898578455106839,-8.49428234908546));
#13968=CARTESIAN_POINT('Ctrl Pts',(2.75225641022963,0.87660057569829,-8.49212413958846));
#13969=CARTESIAN_POINT('Ctrl Pts',(2.72115792865735,0.847036266523619,-8.48929586229167));
#13970=CARTESIAN_POINT('Ctrl Pts',(2.71435048905148,0.840405972757504,-8.48866612744616));
#13971=CARTESIAN_POINT('Ctrl Pts',(2.70342410021016,0.829503165820822,-8.48763743252494));
#13972=CARTESIAN_POINT('Ctrl Pts',(2.69925581182815,0.825280531434257,-8.48724064318669));
#13973=CARTESIAN_POINT('Ctrl Pts',(2.69129480770916,0.817092895909135,-8.48647425703022));
#13974=CARTESIAN_POINT('Ctrl Pts',(2.68749753550389,0.813132524770494,-8.48610487079755));
#13975=CARTESIAN_POINT('Ctrl Pts',(2.67883843410771,0.803974249263913,-8.48525358057556));
#13976=CARTESIAN_POINT('Ctrl Pts',(2.67399581296909,0.798758560742342,-8.48477088140782));
#13977=CARTESIAN_POINT('Ctrl Pts',(2.65901443198015,0.782326829947111,-8.4832564831037));
#13978=CARTESIAN_POINT('Ctrl Pts',(2.6490445273262,0.770959622067727,-8.48221787510914));
#13979=CARTESIAN_POINT('Ctrl Pts',(2.58514172435429,0.695207147980153,-8.47535155363096));
#13980=CARTESIAN_POINT('Ctrl Pts',(2.53801879968694,0.625412982214548,-8.46925464976282));
#13981=CARTESIAN_POINT('Ctrl Pts',(2.46585157925222,0.48914858571782,-8.45793991106179));
#13982=CARTESIAN_POINT('Ctrl Pts',(2.43859409938251,0.424257483959232,-8.45277110510551));
#13983=CARTESIAN_POINT('Ctrl Pts',(2.41473183721581,0.349312718931294,-8.44727950744019));
#13984=CARTESIAN_POINT('Ctrl Pts',(2.41226849366853,0.341279713674368,-8.44669693316973));
#13985=CARTESIAN_POINT('Ctrl Pts',(2.40877390108438,0.329432945656863,-8.44584731520043));
#13986=CARTESIAN_POINT('Ctrl Pts',(2.407675601022,0.325639471846193,-8.44557668684376));
#13987=CARTESIAN_POINT('Ctrl Pts',(2.40577041564792,0.318932957741597,-8.44510084680316));
#13988=CARTESIAN_POINT('Ctrl Pts',(2.40495563961301,0.316022255524059,-8.444895194759));
#13989=CARTESIAN_POINT('Ctrl Pts',(2.4032069318705,0.309681239384391,-8.4444490787412));
#13990=CARTESIAN_POINT('Ctrl Pts',(2.40227732066876,0.306249815900599,-8.44420886049168));
#13991=CARTESIAN_POINT('Ctrl Pts',(2.39974793001022,0.296742861274635,-8.44354649343665));
#13992=CARTESIAN_POINT('Ctrl Pts',(2.39818117580525,0.2906585503752,-8.44312616282846));
#13993=CARTESIAN_POINT('Ctrl Pts',(2.38987335001104,0.257292698606628,-8.44083915609968));
#13994=CARTESIAN_POINT('Ctrl Pts',(2.38406108336921,0.22978673756206,-8.43901959458475));
#13995=CARTESIAN_POINT('Ctrl Pts',(2.36767240847776,0.135695832573901,-8.43293643656744));
#13996=CARTESIAN_POINT('Ctrl Pts',(2.36182733505878,0.0684204361754785,
-8.42881828362204));
#13997=CARTESIAN_POINT('Ctrl Pts',(2.36171109837723,-0.0670221457747454,
-8.42041453648346));
#13998=CARTESIAN_POINT('Ctrl Pts',(2.36754740706567,-0.134922850805612,
-8.41614138650875));
#13999=CARTESIAN_POINT('Ctrl Pts',(2.3809958634023,-0.212197045817843,-8.41099392244342));
#14000=CARTESIAN_POINT('Ctrl Pts',(2.3829178310719,-0.222434640364436,-8.41030634553304));
#14001=CARTESIAN_POINT('Ctrl Pts',(2.38630535142021,-0.239245825696107,
-8.40916733531976));
#14002=CARTESIAN_POINT('Ctrl Pts',(2.38769197391493,-0.24583487007222,-8.40871837931082));
#14003=CARTESIAN_POINT('Ctrl Pts',(2.39029846120642,-0.257714126105459,
-8.40790422563686));
#14004=CARTESIAN_POINT('Ctrl Pts',(2.39149855791437,-0.263008518053009,
-8.4075396617061));
#14005=CARTESIAN_POINT('Ctrl Pts',(2.39415135534913,-0.274347501794364,
-8.40675511489876));
#14006=CARTESIAN_POINT('Ctrl Pts',(2.39561539294219,-0.280389244629929,
-8.40633478205096));
#14007=CARTESIAN_POINT('Ctrl Pts',(2.39975462755282,-0.296898721168346,
-8.40517972785861));
#14008=CARTESIAN_POINT('Ctrl Pts',(2.40252608536289,-0.307341461882251,
-8.40444196888563));
#14009=CARTESIAN_POINT('Ctrl Pts',(2.41966980699661,-0.368530042638528,
-8.4000756464045));
#14010=CARTESIAN_POINT('Ctrl Pts',(2.43729204199588,-0.418295250520235,
-8.39634362246878));
#14011=CARTESIAN_POINT('Ctrl Pts',(2.49035572886478,-0.541240797259785,
-8.3866695571447));
#14012=CARTESIAN_POINT('Ctrl Pts',(2.53014233362705,-0.612244117505038,
-8.38063578176255));
#14013=CARTESIAN_POINT('Ctrl Pts',(2.59461113326625,-0.703695712638651,
-8.37255123801458));
#14014=CARTESIAN_POINT('Ctrl Pts',(2.61328700866883,-0.728102463512583,
-8.37036139090804));
#14015=CARTESIAN_POINT('Ctrl Pts',(2.63700500402221,-0.756706591717967,
-8.36778032532398));
#14016=CARTESIAN_POINT('Ctrl Pts',(2.64115299219315,-0.761626483244267,
-8.36733584751317));
#14017=CARTESIAN_POINT('Ctrl Pts',(2.64767734312063,-0.769237489966658,
-8.36664773123736));
#14018=CARTESIAN_POINT('Ctrl Pts',(2.6500259606934,-0.771952065249593,-8.36640220114627));
#14019=CARTESIAN_POINT('Ctrl Pts',(2.65439144341123,-0.776951394168435,
-8.36594989383805));
#14020=CARTESIAN_POINT('Ctrl Pts',(2.65640476233692,-0.779239054548447,
-8.36574288020811));
#14021=CARTESIAN_POINT('Ctrl Pts',(2.66102602661373,-0.784449112625628,
-8.36527129217798));
#14022=CARTESIAN_POINT('Ctrl Pts',(2.66363968859208,-0.787366336468796,
-8.36500714286347));
#14023=CARTESIAN_POINT('Ctrl Pts',(2.67179126022163,-0.796373846062074,
-8.36419102470067));
#14024=CARTESIAN_POINT('Ctrl Pts',(2.677378643775,-0.80241931006212,-8.36364255849445));
#14025=CARTESIAN_POINT('Ctrl Pts',(2.69063554465881,-0.816464731761108,
-8.36236517798217));
#14026=CARTESIAN_POINT('Ctrl Pts',(2.69835561024227,-0.824416127297166,
-8.36163958540622));
#14027=CARTESIAN_POINT('Ctrl Pts',(2.72638653046604,-0.852483230938626,
-8.35906425502588));
#14028=CARTESIAN_POINT('Ctrl Pts',(2.74731709514597,-0.871968143662895,
-8.35724969201277));
#14029=CARTESIAN_POINT('Ctrl Pts',(2.83533745573989,-0.948120508046633,
-8.34994587666708));
#14030=CARTESIAN_POINT('Ctrl Pts',(2.907951967483,-0.997961797715426,-8.34463263717578));
#14031=CARTESIAN_POINT('Ctrl Pts',(3.01689772192598,-1.05604615518521,-8.33680003673317));
#14032=CARTESIAN_POINT('Ctrl Pts',(3.04910569725687,-1.07138270307079,-8.33450297401191));
#14033=CARTESIAN_POINT('Ctrl Pts',(3.09127361683347,-1.08916174804517,-8.33149066566375));
#14034=CARTESIAN_POINT('Ctrl Pts',(3.10063973184961,-1.09296944853439,-8.33082134756185));
#14035=CARTESIAN_POINT('Ctrl Pts',(3.11570172974273,-1.09886793412042,-8.32974404639008));
#14036=CARTESIAN_POINT('Ctrl Pts',(3.12136689846352,-1.10103616354446,-8.32933863782942));
#14037=CARTESIAN_POINT('Ctrl Pts',(3.13215460473117,-1.10506967581051,-8.32856613133437));
#14038=CARTESIAN_POINT('Ctrl Pts',(3.13727385261059,-1.1069433495594,-8.32819932169251));
#14039=CARTESIAN_POINT('Ctrl Pts',(3.14896871985422,-1.1111318994336,-8.32736075399843));
#14040=CARTESIAN_POINT('Ctrl Pts',(3.15555220320492,-1.11342405006773,-8.32688826609158));
#14041=CARTESIAN_POINT('Ctrl Pts',(3.17589154265965,-1.12030369213053,-8.32542700848202));
#14042=CARTESIAN_POINT('Ctrl Pts',(3.1897116327207,-1.12469554325453,-8.32443195761117));
#14043=CARTESIAN_POINT('Ctrl Pts',(3.25794026328678,-1.14499858195926,-8.31950681014561));
#14044=CARTESIAN_POINT('Ctrl Pts',(3.31336010578011,-1.1572202988964,-8.31546182403757));
#14045=CARTESIAN_POINT('Ctrl Pts',(3.43094931057503,-1.17438153781219,-8.30682270724011));
#14046=CARTESIAN_POINT('Ctrl Pts',(3.4930733968492,-1.17847438861881,-8.30222594957249));
#14047=CARTESIAN_POINT('Ctrl Pts',(3.57404026514595,-1.17739427150161,-8.29633632062212));
#14048=CARTESIAN_POINT('Ctrl Pts',(3.59284352033292,-1.17669262992757,-8.29497626222724));
#14049=CARTESIAN_POINT('Ctrl Pts',(3.63349208578982,-1.17419938823439,-8.29206246582409));
#14050=CARTESIAN_POINT('Ctrl Pts',(3.65532159167139,-1.17224786397305,-8.29051419852507));
#14051=CARTESIAN_POINT('Ctrl Pts',(3.68293202746475,-1.16900061372482,-8.28858690779628));
#14052=CARTESIAN_POINT('Ctrl Pts',(3.6887734443652,-1.16826916691848,-8.28818093185543));
#14053=CARTESIAN_POINT('Ctrl Pts',(3.69801046151917,-1.1670421188928,-8.28754202573396));
#14054=CARTESIAN_POINT('Ctrl Pts',(3.70140970609501,-1.16657543734981,-8.28730756464445));
#14055=CARTESIAN_POINT('Ctrl Pts',(3.70785420220928,-1.16566196287278,-8.28686436896848));
#14056=CARTESIAN_POINT('Ctrl Pts',(3.71089971888508,-1.16521809190991,-8.28665548889017));
#14057=CARTESIAN_POINT('Ctrl Pts',(3.71807784491507,-1.16414315916352,-8.2861644455726));
#14058=CARTESIAN_POINT('Ctrl Pts',(3.72220888347381,-1.16350202593281,-8.28588284246284));
#14059=CARTESIAN_POINT('Ctrl Pts',(3.73589114198609,-1.16130388427055,-8.28495319087635));
#14060=CARTESIAN_POINT('Ctrl Pts',(3.7454268831382,-1.15965110669471,-8.28431018833489));
#14061=CARTESIAN_POINT('Ctrl Pts',(3.79963017956614,-1.14956664198542,-8.28067765834852));
#14062=CARTESIAN_POINT('Ctrl Pts',(3.84380533166667,-1.1386711839365,-8.27780356820473));
#14063=CARTESIAN_POINT('Ctrl Pts',(3.8911227553943,-1.12404909828158,-8.27471382251194));
#14064=CARTESIAN_POINT('Ctrl Pts',(3.89499492655824,-1.12283054932074,-8.27446089984202));
#14065=CARTESIAN_POINT('Ctrl Pts',(3.96060868788209,-1.10180885897501,-8.27017273092163));
#14066=CARTESIAN_POINT('Ctrl Pts',(4.02057866627441,-1.07697292027265,-8.2662102054588));
#14067=CARTESIAN_POINT('Ctrl Pts',(4.07816941731679,-1.04735421169019,-8.2621380879065));
#14068=CARTESIAN_POINT('',(2.36176920301685,-0.00059952881750885,-8.32476442050443));
#14069=CARTESIAN_POINT('Ctrl Pts',(4.07816915725551,-1.04735434543869,-8.16230176652656));
#14070=CARTESIAN_POINT('Ctrl Pts',(4.06073549734461,-1.05632040627034,-8.16353188364908));
#14071=CARTESIAN_POINT('Ctrl Pts',(4.04307190617316,-1.06485430475583,-8.16477093535508));
#14072=CARTESIAN_POINT('Ctrl Pts',(3.99701977505773,-1.08570004337058,-8.16799473780531));
#14073=CARTESIAN_POINT('Ctrl Pts',(3.96835626301873,-1.09733763424601,-8.16999526366853));
#14074=CARTESIAN_POINT('Ctrl Pts',(3.93025510188608,-1.11108606666217,-8.17266465525085));
#14075=CARTESIAN_POINT('Ctrl Pts',(3.92120121171684,-1.1142287145254,-8.17329967124867));
#14076=CARTESIAN_POINT('Ctrl Pts',(3.90646535603871,-1.11914292169965,-8.17433480590633));
#14077=CARTESIAN_POINT('Ctrl Pts',(3.90080642365143,-1.12098256103426,-8.17473270126296));
#14078=CARTESIAN_POINT('Ctrl Pts',(3.88990968634928,-1.12443385523869,-8.17549972165527));
#14079=CARTESIAN_POINT('Ctrl Pts',(3.88467408494917,-1.12605199389359,-8.1758686252423));
#14080=CARTESIAN_POINT('Ctrl Pts',(3.87253551839709,-1.12971098483687,-8.17672486506758));
#14081=CARTESIAN_POINT('Ctrl Pts',(3.86562481522897,-1.13172518898455,-8.17721304479307));
#14082=CARTESIAN_POINT('Ctrl Pts',(3.84355771358168,-1.13793800079285,-8.17877438232976));
#14083=CARTESIAN_POINT('Ctrl Pts',(3.82833603164517,-1.1418962791287,-8.17985513208896));
#14084=CARTESIAN_POINT('Ctrl Pts',(3.79237505212377,-1.15048263902049,-8.18241838030266));
#14085=CARTESIAN_POINT('Ctrl Pts',(3.77158128612784,-1.15485647691928,-8.18390830313411));
#14086=CARTESIAN_POINT('Ctrl Pts',(3.69263205179868,-1.16924469347928,-8.18959480980407));
#14087=CARTESIAN_POINT('Ctrl Pts',(3.6338755575999,-1.17544552741947,-8.19389261342827));
#14088=CARTESIAN_POINT('Ctrl Pts',(3.50399101501144,-1.1793500889145,-8.20342455683792));
#14089=CARTESIAN_POINT('Ctrl Pts',(3.43301989923687,-1.17506961604388,-8.20865490359785));
#14090=CARTESIAN_POINT('Ctrl Pts',(3.35319778904565,-1.16295957410807,-8.21431328507573));
#14091=CARTESIAN_POINT('Ctrl Pts',(3.3435531050952,-1.16137330225034,-8.21499301095464));
#14092=CARTESIAN_POINT('Ctrl Pts',(3.33009151782234,-1.15898678139177,-8.21593517475724));
#14093=CARTESIAN_POINT('Ctrl Pts',(3.32625746309614,-1.1582874199884,-8.21620276858639));
#14094=CARTESIAN_POINT('Ctrl Pts',(3.31962932290604,-1.1570443690027,-8.21666399584115));
#14095=CARTESIAN_POINT('Ctrl Pts',(3.31683363599089,-1.15650956362117,-8.21685811233292));
#14096=CARTESIAN_POINT('Ctrl Pts',(3.31091535024887,-1.15535515962905,-8.21726810454076));
#14097=CARTESIAN_POINT('Ctrl Pts',(3.30779326886099,-1.15473302510711,-8.21748383126231));
#14098=CARTESIAN_POINT('Ctrl Pts',(3.3000105146125,-1.15314932666193,-8.21802029289698));
#14099=CARTESIAN_POINT('Ctrl Pts',(3.29535301415351,-1.15217214728251,-8.21834016350221));
#14100=CARTESIAN_POINT('Ctrl Pts',(3.27753271886894,-1.1483204004705,-8.21956000107659));
#14101=CARTESIAN_POINT('Ctrl Pts',(3.26441308816788,-1.14524815112546,-8.22044961659397));
#14102=CARTESIAN_POINT('Ctrl Pts',(3.23057450747311,-1.13670900744828,-8.22272901672618));
#14103=CARTESIAN_POINT('Ctrl Pts',(3.20994624849184,-1.13090051643412,-8.22410375475496));
#14104=CARTESIAN_POINT('Ctrl Pts',(3.0949110140873,-1.09509358266368,-8.23174479328571));
#14105=CARTESIAN_POINT('Ctrl Pts',(3.0044250515071,-1.05384189374142,-8.23769211062487));
#14106=CARTESIAN_POINT('Ctrl Pts',(2.88999386488484,-0.983092326946821,
-8.24622934224479));
#14107=CARTESIAN_POINT('Ctrl Pts',(2.86068165635078,-0.963085097966447,
-8.2485150974589));
#14108=CARTESIAN_POINT('Ctrl Pts',(2.82427440828986,-0.935746422877154,
-8.25151234904213));
#14109=CARTESIAN_POINT('Ctrl Pts',(2.81630787696671,-0.929603062779868,
-8.25217838736915));
#14110=CARTESIAN_POINT('Ctrl Pts',(2.80367460499541,-0.91960027709676,-8.25325161890292));
#14111=CARTESIAN_POINT('Ctrl Pts',(2.79895711802928,-0.915805514003791,
-8.25365627182413));
#14112=CARTESIAN_POINT('Ctrl Pts',(2.79022993678891,-0.908673812405774,
-8.2544122689703));
#14113=CARTESIAN_POINT('Ctrl Pts',(2.78621273183558,-0.905346266374552,
-8.2547632326959));
#14114=CARTESIAN_POINT('Ctrl Pts',(2.7821519465749,-0.901936882440655,-8.25512107657468));
#14115=CARTESIAN_POINT('Ctrl Pts',(2.78208607966513,-0.901881569113669,
-8.25512688171452));
#14116=CARTESIAN_POINT('Ctrl Pts',(2.78196023573616,-0.901775865127666,
-8.25513797447173));
#14117=CARTESIAN_POINT('Ctrl Pts',(2.78190025768347,-0.901725475698881,
-8.25514326203924));
#14118=CARTESIAN_POINT('Ctrl Pts',(2.781785524688,-0.901629065410631,-8.25515337802556));
#14119=CARTESIAN_POINT('Ctrl Pts',(2.78173076890668,-0.9015830455441,-8.25515820640423));
#14120=CARTESIAN_POINT('Ctrl Pts',(2.78162590926246,-0.901494899246168,
-8.25516745404972));
#14121=CARTESIAN_POINT('Ctrl Pts',(2.78157580471779,-0.901452773624273,
-8.25517187328376));
#14122=CARTESIAN_POINT('Ctrl Pts',(2.78147975527106,-0.901372005949661,
-8.25518034578901));
#14123=CARTESIAN_POINT('Ctrl Pts',(2.78143380980148,-0.901333364552745,
-8.25518439903413));
#14124=CARTESIAN_POINT('Ctrl Pts',(2.78134565179312,-0.901259209746639,
-8.25519217698409));
#14125=CARTESIAN_POINT('Ctrl Pts',(2.78130343879901,-0.901223696888161,
-8.25519590166635));
#14126=CARTESIAN_POINT('Ctrl Pts',(2.77603242535316,-0.89678867736647,-8.25566103439582));
#14127=CARTESIAN_POINT('Ctrl Pts',(2.77084210881456,-0.89234383202169,-8.25612427268104));
#14128=CARTESIAN_POINT('Ctrl Pts',(2.75996749929069,-0.882865834528284,
-8.25710609299208));
#14129=CARTESIAN_POINT('Ctrl Pts',(2.7542926265547,-0.877822397316013,-8.25762508446563));
#14130=CARTESIAN_POINT('Ctrl Pts',(2.73934452115733,-0.864276611912959,
-8.25901011484282));
#14131=CARTESIAN_POINT('Ctrl Pts',(2.73015830159822,-0.855680136748306,
-8.25988000738303));
#14132=CARTESIAN_POINT('Ctrl Pts',(2.70228727702932,-0.828748017138927,
-8.26257842807472));
#14133=CARTESIAN_POINT('Ctrl Pts',(2.68407570317796,-0.809936308071678,
-8.2644262723009));
#14134=CARTESIAN_POINT('Ctrl Pts',(2.63525212525014,-0.756018914141172,
-8.2696217206456));
#14135=CARTESIAN_POINT('Ctrl Pts',(2.60607407402053,-0.719682643910868,
-8.27301345992998));
#14136=CARTESIAN_POINT('Ctrl Pts',(2.53580503111774,-0.620688669606909,
-8.28191310786105));
#14137=CARTESIAN_POINT('Ctrl Pts',(2.49839701114971,-0.555664500011472,
-8.28744250732238));
#14138=CARTESIAN_POINT('Ctrl Pts',(2.46344431126419,-0.478800661341516,
-8.29335778435933));
#14139=CARTESIAN_POINT('Ctrl Pts',(2.45958349030215,-0.470027784455235,
-8.29402412159409));
#14140=CARTESIAN_POINT('Ctrl Pts',(2.45431653133051,-0.457652152582669,
-8.29495085444575));
#14141=CARTESIAN_POINT('Ctrl Pts',(2.45282050633424,-0.454088400576892,
-8.29521619395022));
#14142=CARTESIAN_POINT('Ctrl Pts',(2.45014844907429,-0.447634327873626,
-8.29569389492909));
#14143=CARTESIAN_POINT('Ctrl Pts',(2.44896631070694,-0.444746580955021,
-8.29590661129576));
#14144=CARTESIAN_POINT('Ctrl Pts',(2.44657173926473,-0.438830126501377,
-8.29634029331725));
#14145=CARTESIAN_POINT('Ctrl Pts',(2.44536039133525,-0.435801026035407,
-8.29656119482868));
#14146=CARTESIAN_POINT('Ctrl Pts',(2.44227879460698,-0.428001330697253,
-8.29712718375281));
#14147=CARTESIAN_POINT('Ctrl Pts',(2.44042703988587,-0.423223431332281,
-8.29747119748459));
#14148=CARTESIAN_POINT('Ctrl Pts',(2.4327599354013,-0.403051021945426,-8.29891291664065));
#14149=CARTESIAN_POINT('Ctrl Pts',(2.42723606091783,-0.387546749506852,
-8.29999483466165));
#14150=CARTESIAN_POINT('Ctrl Pts',(2.41302343835898,-0.344844384244739,
-8.30291682181446));
#14151=CARTESIAN_POINT('Ctrl Pts',(2.40499540442107,-0.31743713828913,-8.3047291022613));
#14152=CARTESIAN_POINT('Ctrl Pts',(2.37397794645469,-0.195241175366891,
-8.31264077386489));
#14153=CARTESIAN_POINT('Ctrl Pts',(2.36181884170173,-0.0981126955574954,
-8.3185224645049));
#14154=CARTESIAN_POINT('Ctrl Pts',(2.36176920301685,-0.00059952881750885,
-8.32476442050443));
#14155=CARTESIAN_POINT('Ctrl Pts',(2.36176920232564,-0.000598169433328872,
-8.32476450752056));
#14156=CARTESIAN_POINT('Ctrl Pts',(2.36176078348145,0.0159778906434922,
-8.32582556508734));
#14157=CARTESIAN_POINT('Ctrl Pts',(2.36210231053494,0.0325518147491741,
-8.32689511243933));
#14158=CARTESIAN_POINT('Ctrl Pts',(2.3632880888756,0.0609627629056844,-8.32874710217912));
#14159=CARTESIAN_POINT('Ctrl Pts',(2.3639616363581,0.0728044195543848,-8.32952454898454));
#14160=CARTESIAN_POINT('Ctrl Pts',(2.36529272230237,0.0912797575822726,
-8.33074720652455));
#14161=CARTESIAN_POINT('Ctrl Pts',(2.36582794586177,0.097921661903201,-8.33118871079188));
#14162=CARTESIAN_POINT('Ctrl Pts',(2.36688523479258,0.109783963946712,-8.33198090684105));
#14163=CARTESIAN_POINT('Ctrl Pts',(2.36738587832962,0.115006128882268,-8.33233093345332));
#14164=CARTESIAN_POINT('Ctrl Pts',(2.36846555335454,0.125527633098669,-8.33303882149122));
#14165=CARTESIAN_POINT('Ctrl Pts',(2.3690457082434,0.130826730141698,-8.33339670969349));
#14166=CARTESIAN_POINT('Ctrl Pts',(2.37036882146246,0.142197836632974,-8.33416770460845));
#14167=CARTESIAN_POINT('Ctrl Pts',(2.37112315013313,0.14826833907374,-8.33458115498868));
#14168=CARTESIAN_POINT('Ctrl Pts',(2.37328079151084,0.164591850499612,-8.33569804832022));
#14169=CARTESIAN_POINT('Ctrl Pts',(2.37477197897301,0.174832495547505,-8.33640420175529));
#14170=CARTESIAN_POINT('Ctrl Pts',(2.38235476865716,0.222493200376698,-8.33971711464745));
#14171=CARTESIAN_POINT('Ctrl Pts',(2.39011539350623,0.259621034503504,-8.34237513906323));
#14172=CARTESIAN_POINT('Ctrl Pts',(2.41357854808535,0.349881821637091,-8.3490306541492));
#14173=CARTESIAN_POINT('Ctrl Pts',(2.43126392072715,0.402403845014105,-8.35307584541218));
#14174=CARTESIAN_POINT('Ctrl Pts',(2.47186594605988,0.499722039360119,-8.36081419854414));
#14175=CARTESIAN_POINT('Ctrl Pts',(2.49408918139198,0.544685400994504,-8.36449572639096));
#14176=CARTESIAN_POINT('Ctrl Pts',(2.52692639280436,0.601661214198898,-8.36920738648013));
#14177=CARTESIAN_POINT('Ctrl Pts',(2.53501305265763,0.615067360084952,-8.37031937416484));
#14178=CARTESIAN_POINT('Ctrl Pts',(2.54907675903647,0.637364700071641,-8.37216983659112));
#14179=CARTESIAN_POINT('Ctrl Pts',(2.55491200851504,0.646342545901904,-8.37291518236059));
#14180=CARTESIAN_POINT('Ctrl Pts',(2.56329036313399,0.65885624575479,-8.37395312550783));
#14181=CARTESIAN_POINT('Ctrl Pts',(2.56573167118435,0.662459164024132,-8.37425185477075));
#14182=CARTESIAN_POINT('Ctrl Pts',(2.56994873913427,0.668609088486464,-8.37476145765566));
#14183=CARTESIAN_POINT('Ctrl Pts',(2.57171468728923,0.671162735380082,-8.37497296830299));
#14184=CARTESIAN_POINT('Ctrl Pts',(2.57517103568886,0.676118774457328,-8.37538324279247));
#14185=CARTESIAN_POINT('Ctrl Pts',(2.57686033829371,0.678521845731866,-8.37558208073538));
#14186=CARTESIAN_POINT('Ctrl Pts',(2.58151871724492,0.685096079024294,-8.37612586870096));
#14187=CARTESIAN_POINT('Ctrl Pts',(2.58450607370395,0.689254301800044,-8.37646961026985));
#14188=CARTESIAN_POINT('Ctrl Pts',(2.59633102872468,0.705489452312067,-8.37781145673959));
#14189=CARTESIAN_POINT('Ctrl Pts',(2.60537179489746,0.717417568419994,-8.37879680066266));
#14190=CARTESIAN_POINT('Ctrl Pts',(2.6625211180006,0.789905837487637,-8.38480389256936));
#14191=CARTESIAN_POINT('Ctrl Pts',(2.71627609625787,0.845783958635265,-8.38952749019953));
#14192=CARTESIAN_POINT('Ctrl Pts',(2.81283353155703,0.928159282717652,-8.397389559084));
#14193=CARTESIAN_POINT('Ctrl Pts',(2.85252957276116,0.957912519213582,-8.40047769743529));
#14194=CARTESIAN_POINT('Ctrl Pts',(2.91000815473591,0.995579411105192,-8.40487403231615));
#14195=CARTESIAN_POINT('Ctrl Pts',(2.92629051023476,1.00569032416323,-8.40611129291946));
#14196=CARTESIAN_POINT('Ctrl Pts',(2.95154890788124,1.02053362371434,-8.40802356147196));
#14197=CARTESIAN_POINT('Ctrl Pts',(2.96035185823942,1.02555502974522,-8.40868873019762));
#14198=CARTESIAN_POINT('Ctrl Pts',(2.97498524871428,1.03365375908587,-8.40979301758771));
#14199=CARTESIAN_POINT('Ctrl Pts',(2.98077878926827,1.03679690615021,-8.41022985052777));
#14200=CARTESIAN_POINT('Ctrl Pts',(2.99204867994407,1.04278922172803,-8.41107907659921));
#14201=CARTESIAN_POINT('Ctrl Pts',(2.99752165794217,1.04564429497018,-8.41149124859477));
#14202=CARTESIAN_POINT('Ctrl Pts',(3.0031273065338,1.04851274432564,-8.41191324272441));
#14203=CARTESIAN_POINT('Ctrl Pts',(3.00323788122554,1.04856930409486,-8.41192156673778));
#14204=CARTESIAN_POINT('Ctrl Pts',(3.00342760145061,1.04866630952776,-8.41193584867706));
#14205=CARTESIAN_POINT('Ctrl Pts',(3.00350674264168,1.04870676373657,-8.41194180630864));
#14206=CARTESIAN_POINT('Ctrl Pts',(3.00369151720069,1.04880118764809,-8.4119557157843));
#14207=CARTESIAN_POINT('Ctrl Pts',(3.00379715412595,1.04885515034204,-8.41196366786963));
#14208=CARTESIAN_POINT('Ctrl Pts',(3.00404358363176,1.04898098741264,-8.41198221833064));
#14209=CARTESIAN_POINT('Ctrl Pts',(3.00418438250648,1.0490528493909,-8.41199281713353));
#14210=CARTESIAN_POINT('Ctrl Pts',(3.00451246163604,1.04922021361064,-8.41201751343464));
#14211=CARTESIAN_POINT('Ctrl Pts',(3.00469975295649,1.0493156940368,-8.41203161168472));
#14212=CARTESIAN_POINT('Ctrl Pts',(3.00974093748187,1.05188397105003,-8.41241107909415));
#14213=CARTESIAN_POINT('Ctrl Pts',(3.01461183209274,1.05432307569324,-8.41277760506912));
#14214=CARTESIAN_POINT('Ctrl Pts',(3.02572890960923,1.05979382811957,-8.413613958701));
#14215=CARTESIAN_POINT('Ctrl Pts',(3.03198528345281,1.06280418644835,-8.41408450255825));
#14216=CARTESIAN_POINT('Ctrl Pts',(3.05125910350334,1.07186911251431,-8.4155339070149));
#14217=CARTESIAN_POINT('Ctrl Pts',(3.06436052435261,1.07774093068685,-8.41651890293448));
#14218=CARTESIAN_POINT('Ctrl Pts',(3.16623233261341,1.12117943555923,-8.4241792865517));
#14219=CARTESIAN_POINT('Ctrl Pts',(3.25918932323782,1.14795222313181,-8.43122245127678));
#14220=CARTESIAN_POINT('Ctrl Pts',(3.39652600960279,1.16981726679668,-8.44142450440444));
#14221=CARTESIAN_POINT('Ctrl Pts',(3.43904440882171,1.17423368633329,-8.44454845461538));
#14222=CARTESIAN_POINT('Ctrl Pts',(3.4959612390448,1.17703072899519,-8.44862038899891));
#14223=CARTESIAN_POINT('Ctrl Pts',(3.51022364871473,1.17747205426027,-8.44963145722491));
#14224=CARTESIAN_POINT('Ctrl Pts',(3.53447613724297,1.17778153594492,-8.45133129499277));
#14225=CARTESIAN_POINT('Ctrl Pts',(3.54446269446469,1.1777819638142,-8.45202564480724));
#14226=CARTESIAN_POINT('Ctrl Pts',(3.5586809796072,1.17760171540678,-8.45300514502328));
#14227=CARTESIAN_POINT('Ctrl Pts',(3.56291326864206,1.17752524032596,-8.45329556270668));
#14228=CARTESIAN_POINT('Ctrl Pts',(3.57022945136861,1.17735357986424,-8.45379551098007));
#14229=CARTESIAN_POINT('Ctrl Pts',(3.57331352286744,1.177269092133,-8.4540056168586));
#14230=CARTESIAN_POINT('Ctrl Pts',(3.57980093206327,1.17706585560554,-8.45444619224068));
#14231=CARTESIAN_POINT('Ctrl Pts',(3.58320411657049,1.176944465197,-8.45467651666644));
#14232=CARTESIAN_POINT('Ctrl Pts',(3.59237350454669,1.1765775697008,-8.45529506806198));
#14233=CARTESIAN_POINT('Ctrl Pts',(3.59813860016192,1.17630443449146,-8.45568181359106));
#14234=CARTESIAN_POINT('Ctrl Pts',(3.62455042772362,1.17485845080363,-8.457444685568));
#14235=CARTESIAN_POINT('Ctrl Pts',(3.64516743184313,1.17318423927814,-8.45879574553957));
#14236=CARTESIAN_POINT('Ctrl Pts',(3.75004831213089,1.16187971710014,-8.46558934874178));
#14237=CARTESIAN_POINT('Ctrl Pts',(3.83314476718577,1.14371053453635,-8.47072471942511));
#14238=CARTESIAN_POINT('Ctrl Pts',(3.96546579235455,1.0993903585392,-8.47941622617269));
#14239=CARTESIAN_POINT('Ctrl Pts',(4.01607619473185,1.07841644012371,-8.4828718505141));
#14240=CARTESIAN_POINT('Ctrl Pts',(4.07779586716481,1.04764318308853,-8.48737551929737));
#14241=CARTESIAN_POINT('Ctrl Pts',(4.09043308348804,1.0410532504195,-8.4883134819999));
#14242=CARTESIAN_POINT('Ctrl Pts',(4.10902642607274,1.03092402098117,-8.48971885375018));
#14243=CARTESIAN_POINT('Ctrl Pts',(4.11507624026926,1.02755871157946,-8.49018018622034));
#14244=CARTESIAN_POINT('Ctrl Pts',(4.12583100290101,1.02145142224118,-8.49100776511676));
#14245=CARTESIAN_POINT('Ctrl Pts',(4.13054730392122,1.0187297558649,-8.49137328327114));
#14246=CARTESIAN_POINT('Ctrl Pts',(4.14049969022332,1.01289409384736,-8.49215022197749));
#14247=CARTESIAN_POINT('Ctrl Pts',(4.14573081111337,1.00977199087759,-8.49256192531093));
#14248=CARTESIAN_POINT('Ctrl Pts',(4.15968315294684,1.0012972866936,-8.49366912193411));
#14249=CARTESIAN_POINT('Ctrl Pts',(4.1683590635553,0.995871476056532,-8.49436724494464));
#14250=CARTESIAN_POINT('Ctrl Pts',(4.20852813092419,0.970016016376495,-8.49764576156005));
#14251=CARTESIAN_POINT('Ctrl Pts',(4.23910055237191,0.94820325248831,-8.50027644314178));
#14252=CARTESIAN_POINT('Ctrl Pts',(4.34468730792228,0.864980202184821,-8.509865916935));
#14253=CARTESIAN_POINT('Ctrl Pts',(4.41309969317005,0.795826513084492,-8.51708911224113));
#14254=CARTESIAN_POINT('Ctrl Pts',(4.48524465052383,0.70224679447951,-8.52563080566304));
#14255=CARTESIAN_POINT('Ctrl Pts',(4.49777338669352,0.685051974154603,-8.52715445888678));
#14256=CARTESIAN_POINT('Ctrl Pts',(4.51742671607161,0.656484041974723,-8.5296015499679));
#14257=CARTESIAN_POINT('Ctrl Pts',(4.52483458296233,0.645312357990113,-8.53053833038903));
#14258=CARTESIAN_POINT('Ctrl Pts',(4.53460721584136,0.630013620454196,-8.53179166238889));
#14259=CARTESIAN_POINT('Ctrl Pts',(4.5371397517018,0.6259956527282,-8.53211812333897));
#14260=CARTESIAN_POINT('Ctrl Pts',(4.54132805893828,0.619260764496889,-8.53266069052015));
#14261=CARTESIAN_POINT('Ctrl Pts',(4.54299722813137,0.616552294285877,-8.53287764345538));
#14262=CARTESIAN_POINT('Ctrl Pts',(4.54613975814134,0.611406512883597,-8.53328743014268));
#14263=CARTESIAN_POINT('Ctrl Pts',(4.54761528325948,0.608970573167416,-8.53348040714606));
#14264=CARTESIAN_POINT('Ctrl Pts',(4.55109230512926,0.603183099193891,-8.53393656499734));
#14265=CARTESIAN_POINT('Ctrl Pts',(4.55308601929775,0.599826892922202,-8.53419925227035));
#14266=CARTESIAN_POINT('Ctrl Pts',(4.56003193179556,0.588000667300395,-8.53511865226972));
#14267=CARTESIAN_POINT('Ctrl Pts',(4.56489510715683,0.579478458143812,-8.53577002527697));
#14268=CARTESIAN_POINT('Ctrl Pts',(4.60361959657166,0.509603489367829,-8.541028813743));
#14269=CARTESIAN_POINT('Ctrl Pts',(4.63205456827286,0.445392584374849,-8.54535691824139));
#14270=CARTESIAN_POINT('Ctrl Pts',(4.67379162317286,0.322602367426191,-8.55337926701765));
#14271=CARTESIAN_POINT('Ctrl Pts',(4.68865901741366,0.264807918989477,-8.55705994800979));
#14272=CARTESIAN_POINT('Ctrl Pts',(4.70282844640128,0.185102235443723,-8.56221864047418));
#14273=CARTESIAN_POINT('Ctrl Pts',(4.70599483514099,0.163968747254171,-8.56359350718065));
#14274=CARTESIAN_POINT('Ctrl Pts',(4.71049919872604,0.127082840863855,-8.56601384679704));
#14275=CARTESIAN_POINT('Ctrl Pts',(4.71209815794922,0.111367653997609,-8.56705147957901));
#14276=CARTESIAN_POINT('Ctrl Pts',(4.71396599474155,0.0884388505797337,
-8.56857697513455));
#14277=CARTESIAN_POINT('Ctrl Pts',(4.71448542527577,0.0812469655499764,
-8.56905711141265));
#14278=CARTESIAN_POINT('Ctrl Pts',(4.71528343765786,0.0685800088011585,
-8.56990586882487));
#14279=CARTESIAN_POINT('Ctrl Pts',(4.71558989610086,0.0631068626366261,
-8.5702736176451));
#14280=CARTESIAN_POINT('Ctrl Pts',(4.71614903908379,0.0516940467651455,
-8.57104267325166));
#14281=CARTESIAN_POINT('Ctrl Pts',(4.71639498017566,0.0457542175321624,
-8.57144417776944));
#14282=CARTESIAN_POINT('Ctrl Pts',(4.71691904845266,0.0302600167263839,
-8.5724948917667));
#14283=CARTESIAN_POINT('Ctrl Pts',(4.71712584639623,0.0207038332566813,
-8.57314628028743));
#14284=CARTESIAN_POINT('Ctrl Pts',(4.71750672063379,-0.0195381573761509,
-8.57590410907704));
#14285=CARTESIAN_POINT('Ctrl Pts',(4.71659779669541,-0.050219693612534,
-8.5780433410594));
#14286=CARTESIAN_POINT('Ctrl Pts',(4.70733399068953,-0.184884185073918,
-8.58759982283007));
#14287=CARTESIAN_POINT('Ctrl Pts',(4.68638390766865,-0.287522454895993,
-8.59537806441465));
#14288=CARTESIAN_POINT('Ctrl Pts',(4.64506917273959,-0.406605480060373,
-8.60449579594782));
#14289=CARTESIAN_POINT('Ctrl Pts',(4.63736336424964,-0.42697431729419,-8.60605646720677));
#14290=CARTESIAN_POINT('Ctrl Pts',(4.62392295508212,-0.459727057020625,
-8.60855596303928));
#14291=CARTESIAN_POINT('Ctrl Pts',(4.61853036117598,-0.472245091705853,
-8.60950880102283));
#14292=CARTESIAN_POINT('Ctrl Pts',(4.61095454229709,-0.489023407460298,
-8.61077994173423));
#14293=CARTESIAN_POINT('Ctrl Pts',(4.60896113534847,-0.493367545810233,
-8.6111085083254));
#14294=CARTESIAN_POINT('Ctrl Pts',(4.6055941985544,-0.500588656288921,-8.61165361075));
#14295=CARTESIAN_POINT('Ctrl Pts',(4.60423535414794,-0.503472360276474,
-8.61187100954129));
#14296=CARTESIAN_POINT('Ctrl Pts',(4.60164255535387,-0.508917286714236,
-8.61228090783311));
#14297=CARTESIAN_POINT('Ctrl Pts',(4.60041101058886,-0.511479612238486,
-8.61247355525552));
#14298=CARTESIAN_POINT('Ctrl Pts',(4.59747529028392,-0.517531387488772,
-8.61292803045502));
#14299=CARTESIAN_POINT('Ctrl Pts',(4.59576309756903,-0.521016944470832,
-8.61318937340532));
#14300=CARTESIAN_POINT('Ctrl Pts',(4.5896708982446,-0.533265536182916,-8.61410651738165));
#14301=CARTESIAN_POINT('Ctrl Pts',(4.58519868258256,-0.541982617598227,
-8.61475698364283));
#14302=CARTESIAN_POINT('Ctrl Pts',(4.54727226219442,-0.613689952245968,
-8.62009747764822));
#14303=CARTESIAN_POINT('Ctrl Pts',(4.50826355218086,-0.673586541315487,
-8.62449772361319));
#14304=CARTESIAN_POINT('Ctrl Pts',(4.42768005500991,-0.77570327773717,-8.63254402284896));
#14305=CARTESIAN_POINT('Ctrl Pts',(4.38789514166113,-0.819025576961739,
-8.63617457326418));
#14306=CARTESIAN_POINT('Ctrl Pts',(4.32958614886297,-0.873692251181874,
-8.64126928940964));
#14307=CARTESIAN_POINT('Ctrl Pts',(4.31373830148116,-0.887766095862214,
-8.64263328865554));
#14308=CARTESIAN_POINT('Ctrl Pts',(4.28550665895609,-0.91150640607757,-8.64503622250764));
#14309=CARTESIAN_POINT('Ctrl Pts',(4.27329295323843,-0.921367061625402,
-8.6460674750963));
#14310=CARTESIAN_POINT('Ctrl Pts',(4.25520064786482,-0.935385828702654,
-8.64758530924305));
#14311=CARTESIAN_POINT('Ctrl Pts',(4.2494748769335,-0.939739069115081,-8.64806427573587));
#14312=CARTESIAN_POINT('Ctrl Pts',(4.23931779162323,-0.947315578756129,
-8.6489116959137));
#14313=CARTESIAN_POINT('Ctrl Pts',(4.23490314428115,-0.950560910315168,
-8.64927928630794));
#14314=CARTESIAN_POINT('Ctrl Pts',(4.22564520798168,-0.957267672088207,
-8.65004873541952));
#14315=CARTESIAN_POINT('Ctrl Pts',(4.22079800950673,-0.960723413776496,
-8.65045079670912));
#14316=CARTESIAN_POINT('Ctrl Pts',(4.20807001540218,-0.969652894894793,
-8.65150459465732));
#14317=CARTESIAN_POINT('Ctrl Pts',(4.20014829255068,-0.975067240938383,
-8.65215853411324));
#14318=CARTESIAN_POINT('Ctrl Pts',(4.16632706798313,-0.997582057101962,
-8.65494305709908));
#14319=CARTESIAN_POINT('Ctrl Pts',(4.13982523641633,-1.01375067267504,-8.65710723485515));
#14320=CARTESIAN_POINT('Ctrl Pts',(4.10129953939983,-1.03521427371071,-8.66023075645344));
#14321=CARTESIAN_POINT('Ctrl Pts',(4.08978158170309,-1.0413821224762,-8.66116176426806));
#14322=CARTESIAN_POINT('Ctrl Pts',(4.07816915742063,-1.04735434535377,-8.66209739867239));
#14323=CARTESIAN_POINT('Origin',(3.53951905042299,8.32667268468867E-16,
0.924367114736157));
#14324=CARTESIAN_POINT('',(4.07816930022569,-1.0473542719097,-9.26219992867132));
#14325=CARTESIAN_POINT('',(4.07816926754755,-1.04735428871594,-9.16390755708093));
#14326=CARTESIAN_POINT('',(4.07816926754759,-1.04735428871592,0.924367114736157));
#14327=CARTESIAN_POINT('',(2.36176880457028,-0.000312140290006209,-8.92337267760163));
#14328=CARTESIAN_POINT('Ctrl Pts',(4.07816930022569,-1.0473542719097,-9.26219992867132));
#14329=CARTESIAN_POINT('Ctrl Pts',(4.08963334306672,-1.04145835903123,-9.26127063730459));
#14330=CARTESIAN_POINT('Ctrl Pts',(4.1010020975504,-1.03537344480409,-9.26033685088515));
#14331=CARTESIAN_POINT('Ctrl Pts',(4.16522820456332,-0.999628076415812,
-9.25499407938348));
#14332=CARTESIAN_POINT('Ctrl Pts',(4.21582958212587,-0.966111787617561,
-9.25051465419603));
#14333=CARTESIAN_POINT('Ctrl Pts',(4.29570019777826,-0.903846834707519,
-9.24314029442522));
#14334=CARTESIAN_POINT('Ctrl Pts',(4.3264615069074,-0.87719515088128,-9.24021534012738));
#14335=CARTESIAN_POINT('Ctrl Pts',(4.36031091982148,-0.844650927099082,
-9.23694933981284));
#14336=CARTESIAN_POINT('Ctrl Pts',(4.36480211480201,-0.840263261988187,
-9.23651499506486));
#14337=CARTESIAN_POINT('Ctrl Pts',(4.37201908160375,-0.833098970981894,
-9.23581571117833));
#14338=CARTESIAN_POINT('Ctrl Pts',(4.37476648882677,-0.830344455691755,
-9.23554918530032));
#14339=CARTESIAN_POINT('Ctrl Pts',(4.37964025009225,-0.825409418096969,
-9.23507589663737));
#14340=CARTESIAN_POINT('Ctrl Pts',(4.38177184379941,-0.823234213558013,
-9.23486873617146));
#14341=CARTESIAN_POINT('Ctrl Pts',(4.3864111418626,-0.818463117163704,-9.23441751402385));
#14342=CARTESIAN_POINT('Ctrl Pts',(4.38891536393468,-0.815863954448002,
-9.23417371553508));
#14343=CARTESIAN_POINT('Ctrl Pts',(4.39604087317134,-0.808399932866357,
-9.23347918874594));
#14344=CARTESIAN_POINT('Ctrl Pts',(4.40063268022099,-0.803506942148487,
-9.23303062349273));
#14345=CARTESIAN_POINT('Ctrl Pts',(4.43368499966977,-0.767677881049802,
-9.2297920926314));
#14346=CARTESIAN_POINT('Ctrl Pts',(4.46051640196867,-0.735273280729588,
-9.22710973787847));
#14347=CARTESIAN_POINT('Ctrl Pts',(4.53757918975904,-0.631346531393782,
-9.21899012150749));
#14348=CARTESIAN_POINT('Ctrl Pts',(4.58163335796371,-0.555626474272578,
-9.21370441083827));
#14349=CARTESIAN_POINT('Ctrl Pts',(4.63152725662795,-0.442631127956828,
-9.20587193656605));
#14350=CARTESIAN_POINT('Ctrl Pts',(4.64460819991752,-0.408878725878092,
-9.20354193730801));
#14351=CARTESIAN_POINT('Ctrl Pts',(4.65933517862198,-0.364978717601283,
-9.20049408875856));
#14352=CARTESIAN_POINT('Ctrl Pts',(4.66243208574637,-0.355336361622174,
-9.19982366696854));
#14353=CARTESIAN_POINT('Ctrl Pts',(4.66718554213982,-0.339853183258862,
-9.19874501033467));
#14354=CARTESIAN_POINT('Ctrl Pts',(4.66892199164482,-0.334037268492338,
-9.19833936166919));
#14355=CARTESIAN_POINT('Ctrl Pts',(4.67213232569506,-0.322973590811261,
-9.19756666953539));
#14356=CARTESIAN_POINT('Ctrl Pts',(4.67361489002397,-0.317728495057857,
-9.19719991644738));
#14357=CARTESIAN_POINT('Ctrl Pts',(4.67690874478701,-0.305758482561444,
-9.19636185880566));
#14358=CARTESIAN_POINT('Ctrl Pts',(4.67869688507542,-0.299027463514963,
-9.19588982767392));
#14359=CARTESIAN_POINT('Ctrl Pts',(4.6840151654805,-0.278267795252604,-9.19443141043853));
#14360=CARTESIAN_POINT('Ctrl Pts',(4.68734651148602,-0.264190103164261,
-9.19343877846734));
#14361=CARTESIAN_POINT('Ctrl Pts',(4.70239420986669,-0.194931884615751,
-9.18853546129311));
#14362=CARTESIAN_POINT('Ctrl Pts',(4.71039341590205,-0.139027482799525,
-9.18451105362411));
#14363=CARTESIAN_POINT('Ctrl Pts',(4.71858583218342,-0.022747468196687,
-9.17603826664869));
#14364=CARTESIAN_POINT('Ctrl Pts',(4.71820837928671,0.0375109533950848,
-9.17159145904167));
#14365=CARTESIAN_POINT('Ctrl Pts',(4.70982465616552,0.138459987042075,-9.16421327406482));
#14366=CARTESIAN_POINT('Ctrl Pts',(4.70427615462658,0.179242910641523,-9.16125432621756));
#14367=CARTESIAN_POINT('Ctrl Pts',(4.69543002744637,0.225841801929512,-9.15795512584361));
#14368=CARTESIAN_POINT('Ctrl Pts',(4.6942061132978,0.232018312735089,-9.15751952514883));
#14369=CARTESIAN_POINT('Ctrl Pts',(4.69214483700591,0.24200007238953,-9.15681862455754));
#14370=CARTESIAN_POINT('Ctrl Pts',(4.69133804372864,0.245811404715399,-9.15655172633476));
#14371=CARTESIAN_POINT('Ctrl Pts',(4.6898667778766,0.252595419317296,-9.15607803813025));
#14372=CARTESIAN_POINT('Ctrl Pts',(4.68920967077125,0.255569595437543,-9.15587084768446));
#14373=CARTESIAN_POINT('Ctrl Pts',(4.68774960209091,0.262058504494397,-9.15541986490099));
#14374=CARTESIAN_POINT('Ctrl Pts',(4.68694203740685,0.265572117087249,-9.15517633353269));
#14375=CARTESIAN_POINT('Ctrl Pts',(4.68458969482365,0.275595805334758,-9.15448334423797));
#14376=CARTESIAN_POINT('Ctrl Pts',(4.6830055284955,0.282096629209457,-9.15403603439235));
#14377=CARTESIAN_POINT('Ctrl Pts',(4.67121284352306,0.32875705178178,-9.15083840015818));
#14378=CARTESIAN_POINT('Ctrl Pts',(4.65894538874058,0.36837145359408,-9.14819261039131));
#14379=CARTESIAN_POINT('Ctrl Pts',(4.61536088769029,0.486637140151741,-9.1402783699292));
#14380=CARTESIAN_POINT('Ctrl Pts',(4.57764197956753,0.562630195292374,-9.13515435698543));
#14381=CARTESIAN_POINT('Ctrl Pts',(4.51106281395198,0.666878027597784,-9.12733329502117));
#14382=CARTESIAN_POINT('Ctrl Pts',(4.48839341349544,0.698756425904325,-9.12482164501113));
#14383=CARTESIAN_POINT('Ctrl Pts',(4.45776177492426,0.737585817886362,-9.12156794623588));
#14384=CARTESIAN_POINT('Ctrl Pts',(4.45123381713147,0.745639800961582,-9.12088191730762));
#14385=CARTESIAN_POINT('Ctrl Pts',(4.44068336071585,0.758310902967337,-9.11978408369215));
#14386=CARTESIAN_POINT('Ctrl Pts',(4.43672960966522,0.762984763740334,-9.11937503229437));
#14387=CARTESIAN_POINT('Ctrl Pts',(4.42954794135272,0.771341439396519,-9.11863610890818));
#14388=CARTESIAN_POINT('Ctrl Pts',(4.42633313032989,0.775035372907749,-9.11830677570351));
#14389=CARTESIAN_POINT('Ctrl Pts',(4.41872399066602,0.783669220839258,-9.11753056446599));
#14390=CARTESIAN_POINT('Ctrl Pts',(4.41431095395292,0.78859235164709,-9.11708292067995));
#14391=CARTESIAN_POINT('Ctrl Pts',(4.40131462950385,0.802847556905981,-9.11577174995042));
#14392=CARTESIAN_POINT('Ctrl Pts',(4.39262204055105,0.812078251290364,-9.11490367186589));
#14393=CARTESIAN_POINT('Ctrl Pts',(4.3725553530735,0.832709352064227,-9.11291885955465));
#14394=CARTESIAN_POINT('Ctrl Pts',(4.36109324951042,0.844020224018436,-9.11179848748276));
#14395=CARTESIAN_POINT('Ctrl Pts',(4.32202449301362,0.881023456425117,-9.10802254504472));
#14396=CARTESIAN_POINT('Ctrl Pts',(4.29341853456765,0.905622545049296,-9.10532590165063));
#14397=CARTESIAN_POINT('Ctrl Pts',(4.19873448746549,0.979445226994026,-9.09662732168164));
#14398=CARTESIAN_POINT('Ctrl Pts',(4.12865545500534,1.02313031586584,-9.09049984960047));
#14399=CARTESIAN_POINT('Ctrl Pts',(4.03142391945597,1.07041510186476,-9.08272768367678));
#14400=CARTESIAN_POINT('Ctrl Pts',(4.00788805977255,1.08092071459722,-9.08089969833643));
#14401=CARTESIAN_POINT('Ctrl Pts',(3.97835066881136,1.09295901750643,-9.07868626043227));
#14402=CARTESIAN_POINT('Ctrl Pts',(3.97265864685262,1.09522723546081,-9.0782633591093));
#14403=CARTESIAN_POINT('Ctrl Pts',(3.9636693543853,1.09872834224854,-9.07760147925565));
#14404=CARTESIAN_POINT('Ctrl Pts',(3.96038391356208,1.09999100823811,-9.07736082638668));
#14405=CARTESIAN_POINT('Ctrl Pts',(3.95452091590766,1.10221417149019,-9.07693366324458));
#14406=CARTESIAN_POINT('Ctrl Pts',(3.95194565856286,1.10318036663616,-9.07674682639839));
#14407=CARTESIAN_POINT('Ctrl Pts',(3.94575839536678,1.10547703413972,-9.07629980351597));
#14408=CARTESIAN_POINT('Ctrl Pts',(3.94214322633311,1.10679883105043,-9.0760401272873));
#14409=CARTESIAN_POINT('Ctrl Pts',(3.93110419472364,1.11077373401279,-9.07525162115299));
#14410=CARTESIAN_POINT('Ctrl Pts',(3.92365993440262,1.11337011048949,-9.07472596184706));
#14411=CARTESIAN_POINT('Ctrl Pts',(3.90625970466304,1.11924358376448,-9.07351015179051));
#14412=CARTESIAN_POINT('Ctrl Pts',(3.89628480994533,1.12246296901949,-9.07282290104905));
#14413=CARTESIAN_POINT('Ctrl Pts',(3.86116177180829,1.13328335453121,-9.07043260088062));
#14414=CARTESIAN_POINT('Ctrl Pts',(3.83580215638392,1.14017617431293,-9.0687595007412));
#14415=CARTESIAN_POINT('Ctrl Pts',(3.73437495640479,1.16413119829472,-9.06219971522339));
#14416=CARTESIAN_POINT('Ctrl Pts',(3.6569262098942,1.17447290519373,-9.05746845855324));
#14417=CARTESIAN_POINT('Ctrl Pts',(3.53156931604559,1.17867981538654,-9.04959495586625));
#14418=CARTESIAN_POINT('Ctrl Pts',(3.48406947340453,1.1774013087679,-9.04656497099992));
#14419=CARTESIAN_POINT('Ctrl Pts',(3.42604321405689,1.17232011891981,-9.0427372482447));
#14420=CARTESIAN_POINT('Ctrl Pts',(3.41532006689647,1.17123260993621,-9.04202468907453));
#14421=CARTESIAN_POINT('Ctrl Pts',(3.39838136732172,1.16927951085471,-9.04089017243358));
#14422=CARTESIAN_POINT('Ctrl Pts',(3.39215504153234,1.16851113234425,-9.04047123282275));
#14423=CARTESIAN_POINT('Ctrl Pts',(3.38055783923645,1.16698578082427,-9.03968720548648));
#14424=CARTESIAN_POINT('Ctrl Pts',(3.37518545506005,1.16624137598451,-9.03932251860125));
#14425=CARTESIAN_POINT('Ctrl Pts',(3.36323066364055,1.16450065979171,-9.03850759904843));
#14426=CARTESIAN_POINT('Ctrl Pts',(3.35665121845978,1.1634855971851,-9.03805679208694));
#14427=CARTESIAN_POINT('Ctrl Pts',(3.3373448740235,1.16033925122396,-9.03672699418806));
#14428=CARTESIAN_POINT('Ctrl Pts',(3.32464433158858,1.15805457893625,-9.03584325233268));
#14429=CARTESIAN_POINT('Ctrl Pts',(3.23423826910566,1.14025326364087,-9.02948614802173));
#14430=CARTESIAN_POINT('Ctrl Pts',(3.1582500251045,1.11714074226845,-9.02377049920137));
#14431=CARTESIAN_POINT('Ctrl Pts',(3.01422070215346,1.05691564585518,-9.01233051479835));
#14432=CARTESIAN_POINT('Ctrl Pts',(2.94634207959322,1.02036857650566,-9.00664242673716));
#14433=CARTESIAN_POINT('Ctrl Pts',(2.87467016283542,0.972193495537268,-9.00059461486867));
#14434=CARTESIAN_POINT('Ctrl Pts',(2.86689622447771,0.966831311097906,-8.99993823704848));
#14435=CARTESIAN_POINT('Ctrl Pts',(2.85605205373321,0.959157275726047,-8.99902298535755));
#14436=CARTESIAN_POINT('Ctrl Pts',(2.85292759994875,0.956923192484188,-8.99875932279186));
#14437=CARTESIAN_POINT('Ctrl Pts',(2.84728970449266,0.952850089783382,-8.99828371742789));
#14438=CARTESIAN_POINT('Ctrl Pts',(2.84477252497009,0.951016312772162,-8.99807142961469));
#14439=CARTESIAN_POINT('Ctrl Pts',(2.83968959327961,0.947282421592249,-8.99764292220031));
#14440=CARTESIAN_POINT('Ctrl Pts',(2.83712425097242,0.94538182850305,-8.99742673704875));
#14441=CARTESIAN_POINT('Ctrl Pts',(2.83071938564329,0.940596173958933,-8.99688710575142));
#14442=CARTESIAN_POINT('Ctrl Pts',(2.82688967760883,0.937697982421469,-8.99656454525431));
#14443=CARTESIAN_POINT('Ctrl Pts',(2.81846895712306,0.931244083643993,-8.9958552705697));
#14444=CARTESIAN_POINT('Ctrl Pts',(2.81388626687212,0.92767766332118,-8.99546925057171));
#14445=CARTESIAN_POINT('Ctrl Pts',(2.80058346694731,0.917166034860543,-8.99434801501589));
#14446=CARTESIAN_POINT('Ctrl Pts',(2.79193511747921,0.910130548343248,-8.99361821525855));
#14447=CARTESIAN_POINT('Ctrl Pts',(2.76127234382075,0.884454160107922,-8.99102220184978));
#14448=CARTESIAN_POINT('Ctrl Pts',(2.73984326759052,0.865127720320402,-8.98919177269108));
#14449=CARTESIAN_POINT('Ctrl Pts',(2.65448340844706,0.782258625648962,-8.98172854256945));
#14450=CARTESIAN_POINT('Ctrl Pts',(2.5972423842953,0.712272274297962,-8.97627865820013));
#14451=CARTESIAN_POINT('Ctrl Pts',(2.53047149259053,0.608306034599382,-8.96842090093681));
#14452=CARTESIAN_POINT('Ctrl Pts',(2.51360955787103,0.57941573864605,-8.96626259963272));
#14453=CARTESIAN_POINT('Ctrl Pts',(2.49339641322563,0.541128213777162,-8.96341113527916));
#14454=CARTESIAN_POINT('Ctrl Pts',(2.48890217169691,0.53234996030533,-8.9627580081856));
#14455=CARTESIAN_POINT('Ctrl Pts',(2.48184658109268,0.518131402611675,-8.96170059706348));
#14456=CARTESIAN_POINT('Ctrl Pts',(2.47921567050628,0.512725992147499,-8.96129871906388));
#14457=CARTESIAN_POINT('Ctrl Pts',(2.47427286168787,0.502369856149128,-8.96052886436018));
#14458=CARTESIAN_POINT('Ctrl Pts',(2.47195380031458,0.497422707581607,-8.9601611448831));
#14459=CARTESIAN_POINT('Ctrl Pts',(2.46671179418306,0.486034650087646,-8.95931467700909));
#14460=CARTESIAN_POINT('Ctrl Pts',(2.46381230526263,0.47958324070721,-8.9588351480557));
#14461=CARTESIAN_POINT('Ctrl Pts',(2.45492885865795,0.459331504189362,-8.95732961954061));
#14462=CARTESIAN_POINT('Ctrl Pts',(2.44915125745764,0.445442874693758,-8.95629677508804));
#14463=CARTESIAN_POINT('Ctrl Pts',(2.43629641795002,0.412791587659935,-8.95386670986936));
#14464=CARTESIAN_POINT('Ctrl Pts',(2.4294294010271,0.393951722943571,-8.95246307168722));
#14465=CARTESIAN_POINT('Ctrl Pts',(2.40604235155459,0.324312519831071,-8.9472686394524));
#14466=CARTESIAN_POINT('Ctrl Pts',(2.39250378116479,0.272585558554468,-8.9433949359844));
#14467=CARTESIAN_POINT('Ctrl Pts',(2.36869852434421,0.147462386188431,-8.93406709201026));
#14468=CARTESIAN_POINT('Ctrl Pts',(2.36174956856233,0.0736584921003024,
-8.92859389040902));
#14469=CARTESIAN_POINT('Ctrl Pts',(2.36176909144411,-0.000310846004542871,
-8.92337227123527));
#14470=CARTESIAN_POINT('Ctrl Pts',(2.36176909177713,-0.000312105247537074,
-8.92337218234323));
#14471=CARTESIAN_POINT('Ctrl Pts',(2.36177231614068,-0.0124794560323217,
-8.92251326923424));
#14472=CARTESIAN_POINT('Ctrl Pts',(2.36196409229702,-0.0246466945384356,
-8.92166180223257));
#14473=CARTESIAN_POINT('Ctrl Pts',(2.36247050361707,-0.0408418590511107,
-8.92054020408476));
#14474=CARTESIAN_POINT('Ctrl Pts',(2.362617316509,-0.0448736989792606,-8.92026194889334));
#14475=CARTESIAN_POINT('Ctrl Pts',(2.36291075130765,-0.0519342519770015,
-8.91977645943059));
#14476=CARTESIAN_POINT('Ctrl Pts',(2.36304835584035,-0.0549632730162014,
-8.91956875898379));
#14477=CARTESIAN_POINT('Ctrl Pts',(2.36334290853361,-0.0609380626644507,
-8.91916025015191));
#14478=CARTESIAN_POINT('Ctrl Pts',(2.36349922911758,-0.0638838392538005,
-8.91895941147573));
#14479=CARTESIAN_POINT('Ctrl Pts',(2.36386097653497,-0.0702487557989056,
-8.91852672076499));
#14480=CARTESIAN_POINT('Ctrl Pts',(2.36407025187672,-0.0736676125520782,
-8.91829508170281));
#14481=CARTESIAN_POINT('Ctrl Pts',(2.36467799633847,-0.0829331121346435,
-8.91766930113932));
#14482=CARTESIAN_POINT('Ctrl Pts',(2.36510519782933,-0.0887778677943178,
-8.91727670077202));
#14483=CARTESIAN_POINT('Ctrl Pts',(2.36731058186096,-0.11614008789068,-8.91544778385838));
#14484=CARTESIAN_POINT('Ctrl Pts',(2.36963672974143,-0.137610721060054,
-8.91403886236286));
#14485=CARTESIAN_POINT('Ctrl Pts',(2.38133402428916,-0.22345833706628,-8.90846743496257));
#14486=CARTESIAN_POINT('Ctrl Pts',(2.39544112017721,-0.287077292534596,
-8.90447455344316));
#14487=CARTESIAN_POINT('Ctrl Pts',(2.43703807823093,-0.421058881289123,
-8.89579171533054));
#14488=CARTESIAN_POINT('Ctrl Pts',(2.4661742525164,-0.4905953086895,-8.89110400683701));
#14489=CARTESIAN_POINT('Ctrl Pts',(2.50793363757105,-0.568417288364759,
-8.8853247761715));
#14490=CARTESIAN_POINT('Ctrl Pts',(2.51431974038685,-0.579856042604948,
-8.88446131719707));
#14491=CARTESIAN_POINT('Ctrl Pts',(2.52425670568453,-0.596977623060411,
-8.88314631488429));
#14492=CARTESIAN_POINT('Ctrl Pts',(2.52766757932933,-0.602740830219868,
-8.88269974011925));
#14493=CARTESIAN_POINT('Ctrl Pts',(2.53393074493679,-0.613120433271041,
-8.88188812492872));
#14494=CARTESIAN_POINT('Ctrl Pts',(2.5367661625282,-0.617746833225735,-8.88152370008984));
#14495=CARTESIAN_POINT('Ctrl Pts',(2.54293252729267,-0.627653840240728,
-8.88073745886427));
#14496=CARTESIAN_POINT('Ctrl Pts',(2.54627368435401,-0.632927864330125,
-8.88031527838795));
#14497=CARTESIAN_POINT('Ctrl Pts',(2.55542440021407,-0.647121385776659,
-8.87916910557777));
#14498=CARTESIAN_POINT('Ctrl Pts',(2.56131308989063,-0.655988913307658,
-8.87844222248564));
#14499=CARTESIAN_POINT('Ctrl Pts',(2.59280065046521,-0.702037783473917,
-8.8746093584544));
#14500=CARTESIAN_POINT('Ctrl Pts',(2.62039827712374,-0.737800020886741,
-8.87142906096169));
#14501=CARTESIAN_POINT('Ctrl Pts',(2.72094054186407,-0.853667504362611,
-8.86040848353568));
#14502=CARTESIAN_POINT('Ctrl Pts',(2.80283439872371,-0.925263300356887,
-8.85227333757289));
#14503=CARTESIAN_POINT('Ctrl Pts',(2.90152362503403,-0.990026502614511,
-8.84392696276257));
#14504=CARTESIAN_POINT('Ctrl Pts',(2.90976392173099,-0.995288466050037,
-8.84324040757507));
#14505=CARTESIAN_POINT('Ctrl Pts',(2.92257112261698,-1.00324394137235,-8.84219027383643));
#14506=CARTESIAN_POINT('Ctrl Pts',(2.92709209135357,-1.00601012611928,-8.84182277416599));
#14507=CARTESIAN_POINT('Ctrl Pts',(2.93552925982405,-1.01109450750296,-8.84114307391586));
#14508=CARTESIAN_POINT('Ctrl Pts',(2.93944050101716,-1.01342069571614,-8.8408304082343));
#14509=CARTESIAN_POINT('Ctrl Pts',(2.94604676579269,-1.01729807712049,-8.84030649511363));
#14510=CARTESIAN_POINT('Ctrl Pts',(2.94873459662084,-1.01886135475544,-8.84009449452714));
#14511=CARTESIAN_POINT('Ctrl Pts',(2.9539029945154,-1.02184003325973,-8.83968910540955));
#14512=CARTESIAN_POINT('Ctrl Pts',(2.95638256253205,-1.02325708179407,-8.83949560891932));
#14513=CARTESIAN_POINT('Ctrl Pts',(2.96228996236755,-1.02660465558767,-8.83903690863292));
#14514=CARTESIAN_POINT('Ctrl Pts',(2.96572238797495,-1.02852706830489,-8.83877221143111));
#14515=CARTESIAN_POINT('Ctrl Pts',(2.9779055997819,-1.03527059830275,-8.83783889164384));
#14516=CARTESIAN_POINT('Ctrl Pts',(2.98670832404251,-1.03999769069367,-8.8371758217598));
#14517=CARTESIAN_POINT('Ctrl Pts',(3.04657770056838,-1.07117275790117,-8.83273452174878));
#14518=CARTESIAN_POINT('Ctrl Pts',(3.09946859370275,-1.09396504642525,-8.8291419138987));
#14519=CARTESIAN_POINT('Ctrl Pts',(3.19913497165124,-1.12850961528438,-8.82260172546278));
#14520=CARTESIAN_POINT('Ctrl Pts',(3.24536697292716,-1.14143319377165,-8.81965237923606));
#14521=CARTESIAN_POINT('Ctrl Pts',(3.34442092574751,-1.16270299392756,-8.81331692873009));
#14522=CARTESIAN_POINT('Ctrl Pts',(3.39727873306971,-1.17034530686602,-8.80992542131133));
#14523=CARTESIAN_POINT('Ctrl Pts',(3.46126980497719,-1.17519762780947,-8.80570760389383));
#14524=CARTESIAN_POINT('Ctrl Pts',(3.47208192614711,-1.17586760747678,-8.80499129516506));
#14525=CARTESIAN_POINT('Ctrl Pts',(3.48911704761752,-1.1766874791496,-8.80385626827961));
#14526=CARTESIAN_POINT('Ctrl Pts',(3.49533480206862,-1.17693735396795,-8.80344064021155));
#14527=CARTESIAN_POINT('Ctrl Pts',(3.5069794176266,-1.17731291464548,-8.802659597622));
#14528=CARTESIAN_POINT('Ctrl Pts',(3.51240575520512,-1.17745037866853,-8.80229455713028));
#14529=CARTESIAN_POINT('Ctrl Pts',(3.5245564279757,-1.17767415073417,-8.80147465256933));
#14530=CARTESIAN_POINT('Ctrl Pts',(3.5312808972948,-1.17774038521574,-8.8010191807041));
#14531=CARTESIAN_POINT('Ctrl Pts',(3.54839348320659,-1.17776237774439,-8.79985554920618));
#14532=CARTESIAN_POINT('Ctrl Pts',(3.55878094268081,-1.17763828976162,-8.79914495935162));
#14533=CARTESIAN_POINT('Ctrl Pts',(3.64445378739264,-1.17548106781179,-8.79324761506457));
#14534=CARTESIAN_POINT('Ctrl Pts',(3.7193729583074,-1.1663686175127,-8.78784016432703));
#14535=CARTESIAN_POINT('Ctrl Pts',(3.8497285256343,-1.13765184422876,-8.77807623586314));
#14536=CARTESIAN_POINT('Ctrl Pts',(3.90555469519211,-1.12093701855502,-8.77377774225982));
#14537=CARTESIAN_POINT('Ctrl Pts',(3.97892912238956,-1.09289893176094,-8.76810670357589));
#14538=CARTESIAN_POINT('Ctrl Pts',(3.9977505134751,-1.08514206931875,-8.76665058505482));
#14539=CARTESIAN_POINT('Ctrl Pts',(4.02823573009161,-1.07164345030026,-8.76429956479538));
#14540=CARTESIAN_POINT('Ctrl Pts',(4.04002187807957,-1.06618977294646,-8.76339250896237));
#14541=CARTESIAN_POINT('Ctrl Pts',(4.05594175985787,-1.05850114302582,-8.7621722110569));
#14542=CARTESIAN_POINT('Ctrl Pts',(4.06015536865852,-1.05643500065844,-8.76184970093639));
#14543=CARTESIAN_POINT('Ctrl Pts',(4.06719449747374,-1.05293102069315,-8.76131185770972));
#14544=CARTESIAN_POINT('Ctrl Pts',(4.07002673003855,-1.05150687796724,-8.76109570838924));
#14545=CARTESIAN_POINT('Ctrl Pts',(4.07462752246215,-1.04917012245422,-8.76074504322008));
#14546=CARTESIAN_POINT('Ctrl Pts',(4.07639953927922,-1.04826445304739,-8.76061009249694));
#14547=CARTESIAN_POINT('Ctrl Pts',(4.07816926754756,-1.04735428871593,-8.76047541727166));
#14548=CARTESIAN_POINT('Ctrl Pts',(4.07816915742063,-1.04735434535377,-8.66209739867239));
#14549=CARTESIAN_POINT('Ctrl Pts',(3.9974608073836,-1.08886232360001,-8.66860021902885));
#14550=CARTESIAN_POINT('Ctrl Pts',(3.9121910246898,-1.12091888908839,-8.67535949568211));
#14551=CARTESIAN_POINT('Ctrl Pts',(3.80295645902651,-1.14811531261076,-8.68350208996762));
#14552=CARTESIAN_POINT('Ctrl Pts',(3.78170985860687,-1.15278435411068,-8.68506098222062));
#14553=CARTESIAN_POINT('Ctrl Pts',(3.74696882773482,-1.15941584067738,-8.68755796389704));
#14554=CARTESIAN_POINT('Ctrl Pts',(3.73354871872066,-1.16173707413847,-8.68851003417399));
#14555=CARTESIAN_POINT('Ctrl Pts',(3.71536907575789,-1.16455771054805,-8.68978032429001));
#14556=CARTESIAN_POINT('Ctrl Pts',(3.71064296518156,-1.1652615587842,-8.69010879091327));
#14557=CARTESIAN_POINT('Ctrl Pts',(3.70275712088072,-1.16638696610513,-8.69065377289713));
#14558=CARTESIAN_POINT('Ctrl Pts',(3.69959977072883,-1.16682448810688,-8.69087115044265));
#14559=CARTESIAN_POINT('Ctrl Pts',(3.69362286572639,-1.16762800578355,-8.6912810430475));
#14560=CARTESIAN_POINT('Ctrl Pts',(3.69080370318118,-1.16799661817063,-8.69147370580855));
#14561=CARTESIAN_POINT('Ctrl Pts',(3.68412993167606,-1.16884466158273,-8.69192825967762));
#14562=CARTESIAN_POINT('Ctrl Pts',(3.68027420150043,-1.1693152433769,-8.69218966554994));
#14563=CARTESIAN_POINT('Ctrl Pts',(3.66667920828045,-1.17090625721777,-8.6931073248795));
#14564=CARTESIAN_POINT('Ctrl Pts',(3.65692803206303,-1.17192419350708,-8.69375823543138));
#14565=CARTESIAN_POINT('Ctrl Pts',(3.57638729633102,-1.1793165244109,-8.69908283427172));
#14566=CARTESIAN_POINT('Ctrl Pts',(3.50515659306746,-1.17939339271543,-8.70346881539347));
#14567=CARTESIAN_POINT('Ctrl Pts',(3.37566820087746,-1.16778366451642,-8.71151053143475));
#14568=CARTESIAN_POINT('Ctrl Pts',(3.31747213223363,-1.15812792746867,-8.7151511905174));
#14569=CARTESIAN_POINT('Ctrl Pts',(3.23962288714567,-1.1391259629978,-8.72025881467248));
#14570=CARTESIAN_POINT('Ctrl Pts',(3.21914168993476,-1.13353603150022,-8.72162501662779));
#14571=CARTESIAN_POINT('Ctrl Pts',(3.18377904313101,-1.12284955277767,-8.72403147961915));
#14572=CARTESIAN_POINT('Ctrl Pts',(3.16882761329751,-1.11800263486215,-8.72506402673299));
#14573=CARTESIAN_POINT('Ctrl Pts',(3.14717836349303,-1.11050242466259,-8.72658341566333));
#14574=CARTESIAN_POINT('Ctrl Pts',(3.14040039252556,-1.10808444753885,-8.72706261987008));
#14575=CARTESIAN_POINT('Ctrl Pts',(3.1285011019195,-1.10371614810957,-8.7279103115993));
#14576=CARTESIAN_POINT('Ctrl Pts',(3.12337039133706,-1.10179189568675,-8.72827793399818));
#14577=CARTESIAN_POINT('Ctrl Pts',(3.11269578886876,-1.0977032312863,-8.72904730221079));
#14578=CARTESIAN_POINT('Ctrl Pts',(3.10715451345502,-1.09553246666253,-8.72944924960882));
#14579=CARTESIAN_POINT('Ctrl Pts',(3.0927297134724,-1.08975514371388,-8.73050241678896));
#14580=CARTESIAN_POINT('Ctrl Pts',(3.08387350838729,-1.08608200218113,-8.73115583450176));
#14581=CARTESIAN_POINT('Ctrl Pts',(3.04660893451506,-1.07009038831552,-8.73393489708089));
#14582=CARTESIAN_POINT('Ctrl Pts',(3.01864962864896,-1.05676324728888,-8.73609397126681));
#14583=CARTESIAN_POINT('Ctrl Pts',(2.91773099252175,-1.00368077754352,-8.74416946267091));
#14584=CARTESIAN_POINT('Ctrl Pts',(2.84851704391596,-0.957344434425838,
-8.7502922529012));
#14585=CARTESIAN_POINT('Ctrl Pts',(2.74472765957978,-0.870701745962381,
-8.76018915930182));
#14586=CARTESIAN_POINT('Ctrl Pts',(2.70695127873819,-0.834653874771428,
-8.76397278175873));
#14587=CARTESIAN_POINT('Ctrl Pts',(2.66698249561753,-0.791090020150359,
-8.76808479599442));
#14588=CARTESIAN_POINT('Ctrl Pts',(2.66232473464918,-0.78592213206882,-8.7685657755721));
#14589=CARTESIAN_POINT('Ctrl Pts',(2.65528618998126,-0.777972179902232,
-8.76929495459797));
#14590=CARTESIAN_POINT('Ctrl Pts',(2.65287222992097,-0.775219891899317,
-8.76954546645073));
#14591=CARTESIAN_POINT('Ctrl Pts',(2.64847626374007,-0.770160415417471,
-8.77000238434609));
#14592=CARTESIAN_POINT('Ctrl Pts',(2.64649035360601,-0.76785679672948,-8.77020906624987));
#14593=CARTESIAN_POINT('Ctrl Pts',(2.64202693822144,-0.762638579443017,
-8.77067421435091));
#14594=CARTESIAN_POINT('Ctrl Pts',(2.63955469344502,-0.759719587427232,
-8.77093230250886));
#14595=CARTESIAN_POINT('Ctrl Pts',(2.63320127463518,-0.752143538191937,
-8.77159688184241));
#14596=CARTESIAN_POINT('Ctrl Pts',(2.62934169925146,-0.747468397983037,
-8.77200188949428));
#14597=CARTESIAN_POINT('Ctrl Pts',(2.60366932200679,-0.715877493478427,
-8.77470620070683));
#14598=CARTESIAN_POINT('Ctrl Pts',(2.58301493252321,-0.688037555303019,
-8.77693295254152));
#14599=CARTESIAN_POINT('Ctrl Pts',(2.54783916841607,-0.635971961828979,
-8.78090331680849));
#14600=CARTESIAN_POINT('Ctrl Pts',(2.53290471655096,-0.612059660536366,
-8.78265818904448));
#14601=CARTESIAN_POINT('Ctrl Pts',(2.49494161028182,-0.546120513736313,
-8.78737575616374));
#14602=CARTESIAN_POINT('Ctrl Pts',(2.47359651584187,-0.5031885361905,-8.79032150375918));
#14603=CARTESIAN_POINT('Ctrl Pts',(2.4340991329798,-0.409873764049416,-8.79665774635196));
#14604=CARTESIAN_POINT('Ctrl Pts',(2.41664772513331,-0.35931684385472,-8.80005391721409));
#14605=CARTESIAN_POINT('Ctrl Pts',(2.39985779673868,-0.297295624501065,
-8.8042768975133));
#14606=CARTESIAN_POINT('Ctrl Pts',(2.39717105565113,-0.286798723063731,
-8.80499336421082));
#14607=CARTESIAN_POINT('Ctrl Pts',(2.39316992523516,-0.270217445195534,
-8.80612854492578));
#14608=CARTESIAN_POINT('Ctrl Pts',(2.3917582452502,-0.264156991407749,-8.80654416676548));
#14609=CARTESIAN_POINT('Ctrl Pts',(2.3892054044546,-0.252790491024977,-8.80732513892054));
#14610=CARTESIAN_POINT('Ctrl Pts',(2.38805276118713,-0.247487170412317,
-8.8076901148465));
#14611=CARTESIAN_POINT('Ctrl Pts',(2.38555451204194,-0.23559732256814,-8.80850979656875));
#14612=CARTESIAN_POINT('Ctrl Pts',(2.38422857218946,-0.229006903620162,
-8.80896510934774));
#14613=CARTESIAN_POINT('Ctrl Pts',(2.38099857394131,-0.212210176042844,
-8.81012818078284));
#14614=CARTESIAN_POINT('Ctrl Pts',(2.37917295526403,-0.201989555996275,
-8.8108383661953));
#14615=CARTESIAN_POINT('Ctrl Pts',(2.36696642770435,-0.128014622434676,
-8.81599763491008));
#14616=CARTESIAN_POINT('Ctrl Pts',(2.36171261891292,-0.0635365509780738,
-8.82060582498249));
#14617=CARTESIAN_POINT('Ctrl Pts',(2.36181433349692,0.0519195771972148,
-8.82901285139798));
#14618=CARTESIAN_POINT('Ctrl Pts',(2.36515651413367,0.102744742857314,-8.83276508705235));
#14619=CARTESIAN_POINT('Ctrl Pts',(2.3778751890873,0.199695647522794,-8.8399088433191));
#14620=CARTESIAN_POINT('Ctrl Pts',(2.38674892915628,0.245798462044947,-8.84329878187754));
#14621=CARTESIAN_POINT('Ctrl Pts',(2.3999257152051,0.29742676582827,-8.84700591707656));
#14622=CARTESIAN_POINT('Ctrl Pts',(2.40155132085988,0.303587057758833,-8.84744675703674));
#14623=CARTESIAN_POINT('Ctrl Pts',(2.4042571527352,0.313513689506547,-8.84815437436656));
#14624=CARTESIAN_POINT('Ctrl Pts',(2.40530629706599,0.317288261814352,-8.84842279897806));
#14625=CARTESIAN_POINT('Ctrl Pts',(2.40720491253418,0.323989259454611,-8.84889810020102));
#14626=CARTESIAN_POINT('Ctrl Pts',(2.40804692610096,0.326917695634533,-8.84910538888988));
#14627=CARTESIAN_POINT('Ctrl Pts',(2.40990513071156,0.333287154191222,-8.84955531254499));
#14628=CARTESIAN_POINT('Ctrl Pts',(2.4109256845474,0.336726818231201,-8.84979769587075));
#14629=CARTESIAN_POINT('Ctrl Pts',(2.41387130656833,0.346490868119096,-8.85048421364171));
#14630=CARTESIAN_POINT('Ctrl Pts',(2.41583396400575,0.352803906558349,-8.8509262619992));
#14631=CARTESIAN_POINT('Ctrl Pts',(2.42977748094404,0.396357244641593,-8.85396543418084));
#14632=CARTESIAN_POINT('Ctrl Pts',(2.44355552443413,0.433001232753845,-8.85646949173506));
#14633=CARTESIAN_POINT('Ctrl Pts',(2.4902530283988,0.540597345477947,-8.86385036691219));
#14634=CARTESIAN_POINT('Ctrl Pts',(2.52843315541402,0.609024420041593,-8.86859470968871));
#14635=CARTESIAN_POINT('Ctrl Pts',(2.59999073242161,0.711753501755807,-8.87645640607158));
#14636=CARTESIAN_POINT('Ctrl Pts',(2.62915337702536,0.748692232846074,-8.87945856176948));
#14637=CARTESIAN_POINT('Ctrl Pts',(2.667598761611,0.791811643273932,-8.88325503414764));
#14638=CARTESIAN_POINT('Ctrl Pts',(2.67486353588126,0.799738392945461,-8.8839659080122));
#14639=CARTESIAN_POINT('Ctrl Pts',(2.6865328737979,0.812126173364211,-8.88509829773899));
#14640=CARTESIAN_POINT('Ctrl Pts',(2.69086639221976,0.816653538620872,-8.88551681436602));
#14641=CARTESIAN_POINT('Ctrl Pts',(2.69901696684668,0.825033770216634,-8.88630039219691));
#14642=CARTESIAN_POINT('Ctrl Pts',(2.7028249186663,0.828895290548517,-8.88666505556511));
#14643=CARTESIAN_POINT('Ctrl Pts',(2.71137063056066,0.837442330187668,-8.88748036288836));
#14644=CARTESIAN_POINT('Ctrl Pts',(2.71612172788788,0.842114189286999,-8.88793158445108));
#14645=CARTESIAN_POINT('Ctrl Pts',(2.73021293812381,0.855737129817766,-8.8892640394302));
#14646=CARTESIAN_POINT('Ctrl Pts',(2.73966092889519,0.864574682176917,-8.89015005339014));
#14647=CARTESIAN_POINT('Ctrl Pts',(2.76150175211802,0.884339913236428,-8.89218245226908));
#14648=CARTESIAN_POINT('Ctrl Pts',(2.77398258521334,0.895165835069931,-8.89333273114648));
#14649=CARTESIAN_POINT('Ctrl Pts',(2.81684584474778,0.93079348183847,-8.89724718513228));
#14650=CARTESIAN_POINT('Ctrl Pts',(2.84823566606857,0.954337376119247,-8.90005584414333));
#14651=CARTESIAN_POINT('Ctrl Pts',(2.94065745780453,1.01670297898974,-8.90814548186253));
#14652=CARTESIAN_POINT('Ctrl Pts',(3.00416872283774,1.05153207825113,-8.91350572617452));
#14653=CARTESIAN_POINT('Ctrl Pts',(3.10049717885613,1.09335557254088,-8.92110739508938));
#14654=CARTESIAN_POINT('Ctrl Pts',(3.1310573092291,1.10513621200808,-8.92344538144226));
#14655=CARTESIAN_POINT('Ctrl Pts',(3.1682661599061,1.11772497543486,-8.92617474308405));
#14656=CARTESIAN_POINT('Ctrl Pts',(3.17447839397634,1.11976924116198,-8.92662656994381));
#14657=CARTESIAN_POINT('Ctrl Pts',(3.18414845399379,1.12286234828569,-8.92732357957514));
#14658=CARTESIAN_POINT('Ctrl Pts',(3.18759450376476,1.1239471643922,-8.92757073064642));
#14659=CARTESIAN_POINT('Ctrl Pts',(3.19395393603935,1.12591699716735,-8.92802448380522));
#14660=CARTESIAN_POINT('Ctrl Pts',(3.19686575915843,1.12680657397948,-8.92823133539416));
#14661=CARTESIAN_POINT('Ctrl Pts',(3.2035004005722,1.12880539427537,-8.92870060630465));
#14662=CARTESIAN_POINT('Ctrl Pts',(3.20722528125847,1.12990751977592,-8.92896261696778));
#14663=CARTESIAN_POINT('Ctrl Pts',(3.21870138820684,1.13324143527843,-8.92976559017846));
#14664=CARTESIAN_POINT('Ctrl Pts',(3.22647033874073,1.1354120996197,-8.93030320975343));
#14665=CARTESIAN_POINT('Ctrl Pts',(3.24468724806487,1.1403007501308,-8.93155125643204));
#14666=CARTESIAN_POINT('Ctrl Pts',(3.25515164026599,1.14295528635163,-8.93225856637352));
#14667=CARTESIAN_POINT('Ctrl Pts',(3.29236858716396,1.15185342809371,-8.9347450010297));
#14668=CARTESIAN_POINT('Ctrl Pts',(3.31930291656333,1.15730494356889,-8.93649151118519));
#14669=CARTESIAN_POINT('Ctrl Pts',(3.42661289111125,1.17514182710077,-8.94332756233797));
#14670=CARTESIAN_POINT('Ctrl Pts',(3.50798584085962,1.18013237872005,-8.94825762361707));
#14671=CARTESIAN_POINT('Ctrl Pts',(3.63203742391708,1.17489212978994,-8.95608164288481));
#14672=CARTESIAN_POINT('Ctrl Pts',(3.67471410817305,1.17074883756273,-8.95882626358399));
#14673=CARTESIAN_POINT('Ctrl Pts',(3.72743839243694,1.16270866958556,-8.96233314904268));
#14674=CARTESIAN_POINT('Ctrl Pts',(3.73778789280795,1.16098862352448,-8.9630270704972));
#14675=CARTESIAN_POINT('Ctrl Pts',(3.75422247413022,1.1580311048233,-8.96413845742952));
#14676=CARTESIAN_POINT('Ctrl Pts',(3.76032329199444,1.15688334948042,-8.96455311102073));
#14677=CARTESIAN_POINT('Ctrl Pts',(3.77169085769813,1.1546515603288,-8.96532975844936));
#14678=CARTESIAN_POINT('Ctrl Pts',(3.7769598294118,1.15357958056401,-8.96569136402008));
#14679=CARTESIAN_POINT('Ctrl Pts',(3.78879516213081,1.15108714536521,-8.96650735723418));
#14680=CARTESIAN_POINT('Ctrl Pts',(3.7953570356006,1.14964651880492,-8.96696237107496));
#14681=CARTESIAN_POINT('Ctrl Pts',(3.81478330215444,1.14520702781804,-8.96831735422135));
#14682=CARTESIAN_POINT('Ctrl Pts',(3.82760959976974,1.14204787798827,-8.96922235200541));
#14683=CARTESIAN_POINT('Ctrl Pts',(3.92377167321873,1.11663992015718,-8.97608829831713));
#14684=CARTESIAN_POINT('Ctrl Pts',(4.00447517380053,1.08551606524862,-8.98233993169424));
#14685=CARTESIAN_POINT('Ctrl Pts',(4.14211592463982,1.01424946341971,-8.99371241749511));
#14686=CARTESIAN_POINT('Ctrl Pts',(4.20030761664452,0.977335754283417,-8.99877607047694));
#14687=CARTESIAN_POINT('Ctrl Pts',(4.26278676169745,0.929557012329672,-9.00428974473512));
#14688=CARTESIAN_POINT('Ctrl Pts',(4.2705493939516,0.923464711869176,-9.00497608830097));
#14689=CARTESIAN_POINT('Ctrl Pts',(4.28128243508099,0.914820996256648,-9.00592586438695));
#14690=CARTESIAN_POINT('Ctrl Pts',(4.28431782290389,0.912351447423313,-9.00619455915131));
#14691=CARTESIAN_POINT('Ctrl Pts',(4.28954287146836,0.90805696651733,-9.00665715955587));
#14692=CARTESIAN_POINT('Ctrl Pts',(4.29173829579751,0.906239148296796,-9.00685155493939));
#14693=CARTESIAN_POINT('Ctrl Pts',(4.29636804003268,0.902377289734746,-9.00726150888845));
#14694=CARTESIAN_POINT('Ctrl Pts',(4.29880072645957,0.900331329573268,-9.00747692178079));
#14695=CARTESIAN_POINT('Ctrl Pts',(4.30483711502588,0.895212684173822,-9.00801153566787));
#14696=CARTESIAN_POINT('Ctrl Pts',(4.30843067125841,0.892128023976856,-9.00832988516646));
#14697=CARTESIAN_POINT('Ctrl Pts',(4.32204676994453,0.880296757079998,-9.00953688811507));
#14698=CARTESIAN_POINT('Ctrl Pts',(4.33193992625116,0.871401861724606,-9.010415467372));
#14699=CARTESIAN_POINT('Ctrl Pts',(4.35709153127294,0.848005480232825,-9.01265986497983));
#14700=CARTESIAN_POINT('Ctrl Pts',(4.37211620715281,0.83325874566758,-9.01401120966142));
#14701=CARTESIAN_POINT('Ctrl Pts',(4.41876033807699,0.784955335773308,-9.0182727352167));
#14702=CARTESIAN_POINT('Ctrl Pts',(4.44880950201938,0.749940972771195,-9.02112162475523));
#14703=CARTESIAN_POINT('Ctrl Pts',(4.52517695256765,0.649594585799723,-9.02892155309964));
#14704=CARTESIAN_POINT('Ctrl Pts',(4.56700625576475,0.58117352557196,-9.03387127172343));
#14705=CARTESIAN_POINT('Ctrl Pts',(4.60825665614847,0.495109903431162,-9.04009098670924));
#14706=CARTESIAN_POINT('Ctrl Pts',(4.61466093118684,0.481044474614414,-9.04110659686171));
#14707=CARTESIAN_POINT('Ctrl Pts',(4.62358955710461,0.460365297518273,-9.04260053289578));
#14708=CARTESIAN_POINT('Ctrl Pts',(4.62633415826455,0.453847979323356,-9.04307147184577));
#14709=CARTESIAN_POINT('Ctrl Pts',(4.63110084378756,0.442237801066509,-9.04391079849984));
#14710=CARTESIAN_POINT('Ctrl Pts',(4.63314640866122,0.437154759645407,-9.04427839092883));
#14711=CARTESIAN_POINT('Ctrl Pts',(4.63734020559166,0.426519882548052,-9.04504783533151));
#14712=CARTESIAN_POINT('Ctrl Pts',(4.63948195741612,0.420965675490522,-9.04544988981759));
#14713=CARTESIAN_POINT('Ctrl Pts',(4.64496555133035,0.406417463038636,-9.04650364977647));
#14714=CARTESIAN_POINT('Ctrl Pts',(4.64823969711617,0.397398589305234,-9.04715755775172));
#14715=CARTESIAN_POINT('Ctrl Pts',(4.66275860734872,0.355828555554678,-9.05017527196661));
#14716=CARTESIAN_POINT('Ctrl Pts',(4.67268141784162,0.322836946117174,-9.05258131289991));
#14717=CARTESIAN_POINT('Ctrl Pts',(4.6976792322256,0.224246296643933,-9.05980799065887));
#14718=CARTESIAN_POINT('Ctrl Pts',(4.70859442915503,0.157741295767165,-9.06473732090874));
#14719=CARTESIAN_POINT('Ctrl Pts',(4.71834851226276,0.0314267403889369,
-9.07403414748872));
#14720=CARTESIAN_POINT('Ctrl Pts',(4.71843333017632,-0.028090571689763,
-9.078384477558));
#14721=CARTESIAN_POINT('Ctrl Pts',(4.71328123415862,-0.0973535970792769,
-9.08325489659547));
#14722=CARTESIAN_POINT('Ctrl Pts',(4.71241081294352,-0.107332738819506,
-9.08395179033353));
#14723=CARTESIAN_POINT('Ctrl Pts',(4.71102095152054,-0.121218253733473,
-9.08491368179602));
#14724=CARTESIAN_POINT('Ctrl Pts',(4.71060909679236,-0.125134622392454,
-9.08518411340566));
#14725=CARTESIAN_POINT('Ctrl Pts',(4.70986459912649,-0.131888282537682,
-9.08564888418753));
#14726=CARTESIAN_POINT('Ctrl Pts',(4.70954126553003,-0.134726534286877,
-9.08584372366878));
#14727=CARTESIAN_POINT('Ctrl Pts',(4.70883718672259,-0.140713240091258,
-9.08625363989225));
#14728=CARTESIAN_POINT('Ctrl Pts',(4.70845404537703,-0.143861384066815,
-9.08646857613572));
#14729=CARTESIAN_POINT('Ctrl Pts',(4.70747146660269,-0.151671720433927,
-9.08700036231522));
#14730=CARTESIAN_POINT('Ctrl Pts',(4.70685681754308,-0.15633200747528,-9.0873163802876));
#14731=CARTESIAN_POINT('Ctrl Pts',(4.70443121416943,-0.173910519729584,
-9.08850394839288));
#14732=CARTESIAN_POINT('Ctrl Pts',(4.70243351044067,-0.186802600467899,
-9.08936583651887));
#14733=CARTESIAN_POINT('Ctrl Pts',(4.69674966681931,-0.219845127477472,
-9.09155765517416));
#14734=CARTESIAN_POINT('Ctrl Pts',(4.69275122180787,-0.239937987831161,
-9.09287394953953));
#14735=CARTESIAN_POINT('Ctrl Pts',(4.67546913130656,-0.31631659852697,-9.09784888405803));
#14736=CARTESIAN_POINT('Ctrl Pts',(4.65857075737889,-0.371702645805051,
-9.10139950373775));
#14737=CARTESIAN_POINT('Ctrl Pts',(4.61039727293505,-0.49599443776295,-9.10965336955307));
#14738=CARTESIAN_POINT('Ctrl Pts',(4.57642730481095,-0.563568730204873,
-9.11436669797401));
#14739=CARTESIAN_POINT('Ctrl Pts',(4.53069656898575,-0.636215442441299,
-9.12000056385331));
#14740=CARTESIAN_POINT('Ctrl Pts',(4.52504691559712,-0.644932382720282,
-9.12068627442287));
#14741=CARTESIAN_POINT('Ctrl Pts',(4.51555142579745,-0.659166957573447,
-9.12182279251113));
#14742=CARTESIAN_POINT('Ctrl Pts',(4.51177223848081,-0.664728524211055,
-9.12227114115186));
#14743=CARTESIAN_POINT('Ctrl Pts',(4.50485704497861,-0.674719996704366,
-9.12308459268932));
#14744=CARTESIAN_POINT('Ctrl Pts',(4.50173762532359,-0.679161195974529,
-9.12344906614468));
#14745=CARTESIAN_POINT('Ctrl Pts',(4.49497660692086,-0.688646954383387,
-9.12423386228174));
#14746=CARTESIAN_POINT('Ctrl Pts',(4.49132552186291,-0.693684516485572,
-9.12465453796427));
#14747=CARTESIAN_POINT('Ctrl Pts',(4.48121009473172,-0.707410999539437,
-9.12581169614539));
#14748=CARTESIAN_POINT('Ctrl Pts',(4.47466568515546,-0.716039875404399,
-9.12655123547111));
#14749=CARTESIAN_POINT('Ctrl Pts',(4.4352036206312,-0.766607182388941,-9.13095888137041));
#14750=CARTESIAN_POINT('Ctrl Pts',(4.39959269150756,-0.806355556431621,
-9.13473282140429));
#14751=CARTESIAN_POINT('Ctrl Pts',(4.3270483382367,-0.877037768770133,-9.14205316633322));
#14752=CARTESIAN_POINT('Ctrl Pts',(4.29066669011835,-0.908391113799367,
-9.14557724009955));
#14753=CARTESIAN_POINT('Ctrl Pts',(4.23000442925745,-0.954527152966829,
-9.15116891279376));
#14754=CARTESIAN_POINT('Ctrl Pts',(4.2069245558265,-0.970804887645627,-9.15323666776888));
#14755=CARTESIAN_POINT('Ctrl Pts',(4.15427424381766,-1.00517214255317,-9.15779524132576));
#14756=CARTESIAN_POINT('Ctrl Pts',(4.12444273561059,-1.02281951573375,-9.16027364188836));
#14757=CARTESIAN_POINT('Ctrl Pts',(4.08865973468563,-1.04190906216893,-9.16309254270584));
#14758=CARTESIAN_POINT('Ctrl Pts',(4.08342477633549,-1.04465140108734,-9.16350119446097));
#14759=CARTESIAN_POINT('Ctrl Pts',(4.07816926754757,-1.04735428871593,-9.16390755708093));
#14760=CARTESIAN_POINT('Origin',(3.53951905042299,8.32667268468867E-16,
0.924367114736157));
#14761=CARTESIAN_POINT('',(4.07816928770683,-1.0473542783481,-9.76220700099567));
#14762=CARTESIAN_POINT('',(4.07816926754759,-1.04735428871592,-9.66287031899079));
#14763=CARTESIAN_POINT('',(4.07816926754759,-1.04735428871592,0.924367114736157));
#14764=CARTESIAN_POINT('Ctrl Pts',(4.07816928770683,-1.0473542783481,-9.76220700099567));
#14765=CARTESIAN_POINT('Ctrl Pts',(4.11407533352626,-1.02888793844727,-9.75965837420743));
#14766=CARTESIAN_POINT('Ctrl Pts',(4.14901218989046,-1.00858528532369,-9.75706832671646));
#14767=CARTESIAN_POINT('Ctrl Pts',(4.19188554154775,-0.980627144611524,
-9.75370406310379));
#14768=CARTESIAN_POINT('Ctrl Pts',(4.20084762038751,-0.974605635827041,
-9.75299007620032));
#14769=CARTESIAN_POINT('Ctrl Pts',(4.21483607662237,-0.964925180569075,
-9.75185789672956));
#14770=CARTESIAN_POINT('Ctrl Pts',(4.21991858333983,-0.961348096726768,
-9.75144276766345));
#14771=CARTESIAN_POINT('Ctrl Pts',(4.2293872027655,-0.954571353162807,-9.75066216056236));
#14772=CARTESIAN_POINT('Ctrl Pts',(4.23377998234182,-0.951381255132004,
-9.75029705243418));
#14773=CARTESIAN_POINT('Ctrl Pts',(4.24357308273726,-0.944165425550996,
-9.749476335414));
#14774=CARTESIAN_POINT('Ctrl Pts',(4.24896120298996,-0.940123534502952,
-9.74902011338139));
#14775=CARTESIAN_POINT('Ctrl Pts',(4.26259857468276,-0.929709478957409,
-9.74785327941638));
#14776=CARTESIAN_POINT('Ctrl Pts',(4.2707982984519,-0.923273720499176,-9.74714021421116));
#14777=CARTESIAN_POINT('Ctrl Pts',(4.3357735615412,-0.870867670851135,-9.7413954704903));
#14778=CARTESIAN_POINT('Ctrl Pts',(4.3882350750605,-0.819822731635173,-9.73615707407001));
#14779=CARTESIAN_POINT('Ctrl Pts',(4.46969380638,-0.724311054365501,-9.72698171705269));
#14780=CARTESIAN_POINT('Ctrl Pts',(4.50105406666881,-0.682130520119811,
-9.72310696375967));
#14781=CARTESIAN_POINT('Ctrl Pts',(4.5498944918105,-0.606345249765476,-9.71655719987377));
#14782=CARTESIAN_POINT('Ctrl Pts',(4.56876601542285,-0.57372850389306,-9.71385734250554));
#14783=CARTESIAN_POINT('Ctrl Pts',(4.58905130246254,-0.534434373753748,
-9.71078523715096));
#14784=CARTESIAN_POINT('Ctrl Pts',(4.59201022335995,-0.528583374445563,
-9.71033234969264));
#14785=CARTESIAN_POINT('Ctrl Pts',(4.5965074243875,-0.519503060084191,-9.70963685792346));
#14786=CARTESIAN_POINT('Ctrl Pts',(4.59808005785059,-0.516291048289142,
-9.70939224931919));
#14787=CARTESIAN_POINT('Ctrl Pts',(4.60096609390146,-0.510327864828727,
-9.70894080114829));
#14788=CARTESIAN_POINT('Ctrl Pts',(4.60228344333917,-0.507578763568637,
-9.70873373228062));
#14789=CARTESIAN_POINT('Ctrl Pts',(4.60527631027862,-0.501270386380638,
-9.70826094985865));
#14790=CARTESIAN_POINT('Ctrl Pts',(4.60694468210666,-0.497707804982908,
-9.70799567038162));
#14791=CARTESIAN_POINT('Ctrl Pts',(4.61129108955581,-0.488304255355011,
-9.70729979844479));
#14792=CARTESIAN_POINT('Ctrl Pts',(4.61393927316881,-0.482449519773926,
-9.70687093067232));
#14793=CARTESIAN_POINT('Ctrl Pts',(4.63723488707272,-0.429803148344929,
-9.7030511037493));
#14794=CARTESIAN_POINT('Ctrl Pts',(4.65486465001841,-0.381728150681832,
-9.69981968358328));
#14795=CARTESIAN_POINT('Ctrl Pts',(4.68360244627311,-0.284125579344376,
-9.693479090371));
#14796=CARTESIAN_POINT('Ctrl Pts',(4.69474944676736,-0.234727487176759,
-9.69037486898479));
#14797=CARTESIAN_POINT('Ctrl Pts',(4.71144646138595,-0.129613564760626,
-9.68375035829787));
#14798=CARTESIAN_POINT('Ctrl Pts',(4.71627264706459,-0.0739148273208844,
-9.6802275890705));
#14799=CARTESIAN_POINT('Ctrl Pts',(4.7173512094203,-0.00369563409559671,
-9.67564270659136));
#14800=CARTESIAN_POINT('Ctrl Pts',(4.71730840046682,0.0106990694075942,
-9.67469553898085));
#14801=CARTESIAN_POINT('Ctrl Pts',(4.71685373717589,0.0320375338763051,
-9.67327902833316));
#14802=CARTESIAN_POINT('Ctrl Pts',(4.7166441774608,0.0389846128011234,-9.67281590696469));
#14803=CARTESIAN_POINT('Ctrl Pts',(4.71616067243691,0.0513735405179801,
-9.67198634059529));
#14804=CARTESIAN_POINT('Ctrl Pts',(4.71591042672405,0.0568161542440685,
-9.67162063756692));
#14805=CARTESIAN_POINT('Ctrl Pts',(4.71530123054156,0.0683245864914515,
-9.67084459173008));
#14806=CARTESIAN_POINT('Ctrl Pts',(4.71493308333927,0.0743897374645629,
-9.67043397489875));
#14807=CARTESIAN_POINT('Ctrl Pts',(4.71382396669183,0.0905884179969579,
-9.66933282267605));
#14808=CARTESIAN_POINT('Ctrl Pts',(4.71299878187619,0.10071547297047,-9.66863970712123));
#14809=CARTESIAN_POINT('Ctrl Pts',(4.70860263419762,0.147224292371707,-9.66543407965036));
#14810=CARTESIAN_POINT('Ctrl Pts',(4.70347036786912,0.183434599833315,-9.66287402859214));
#14811=CARTESIAN_POINT('Ctrl Pts',(4.67842658984711,0.315552157758278,-9.65329194281599));
#14812=CARTESIAN_POINT('Ctrl Pts',(4.64826222422651,0.40910656083041,-9.64599264173347));
#14813=CARTESIAN_POINT('Ctrl Pts',(4.59785786745818,0.517174611986315,-9.63737170011505));
#14814=CARTESIAN_POINT('Ctrl Pts',(4.58831107208256,0.536270488108361,-9.63584257391797));
#14815=CARTESIAN_POINT('Ctrl Pts',(4.57191711711579,0.566947821012102,-9.63338771971974));
#14816=CARTESIAN_POINT('Ctrl Pts',(4.56538158671188,0.57868963608482,-9.63244854927329));
#14817=CARTESIAN_POINT('Ctrl Pts',(4.55626341190939,0.594431296096817,-9.63119256127574));
#14818=CARTESIAN_POINT('Ctrl Pts',(4.55385568480442,0.598530581083619,-9.63086578073964));
#14819=CARTESIAN_POINT('Ctrl Pts',(4.54979479815457,0.605349571757633,-9.63032282484557));
#14820=CARTESIAN_POINT('Ctrl Pts',(4.54815533992218,0.608077319695706,-9.63010580021551));
#14821=CARTESIAN_POINT('Ctrl Pts',(4.54502796199032,0.613233235062464,-9.62969595713501));
#14822=CARTESIAN_POINT('Ctrl Pts',(4.54354226345232,0.615662699831442,-9.62950299484803));
#14823=CARTESIAN_POINT('Ctrl Pts',(4.54000031108172,0.621407700344293,-9.62904700348911));
#14824=CARTESIAN_POINT('Ctrl Pts',(4.53793634995609,0.624718480632793,-9.62878446686456));
#14825=CARTESIAN_POINT('Ctrl Pts',(4.53062607625356,0.636316052254224,-9.62786544952819));
#14826=CARTESIAN_POINT('Ctrl Pts',(4.52529256674838,0.644547783244873,-9.62721430529991));
#14827=CARTESIAN_POINT('Ctrl Pts',(4.48092931213473,0.711178930215897,-9.6219448359307));
#14828=CARTESIAN_POINT('Ctrl Pts',(4.43684397683373,0.766054480594075,-9.61760718887869));
#14829=CARTESIAN_POINT('Ctrl Pts',(4.34687781464075,0.859537693119933,-9.60958163811238));
#14830=CARTESIAN_POINT('Ctrl Pts',(4.3024466027896,0.899207490532058,-9.60590752441663));
#14831=CARTESIAN_POINT('Ctrl Pts',(4.23825928288069,0.948321017632823,-9.60075714607797));
#14832=CARTESIAN_POINT('Ctrl Pts',(4.22095889550473,0.960827935050228,-9.59938362501157));
#14833=CARTESIAN_POINT('Ctrl Pts',(4.19029105872178,0.981753525611999,-9.59696539429325));
#14834=CARTESIAN_POINT('Ctrl Pts',(4.17707614783968,0.990386339291828,-9.59592850385312));
#14835=CARTESIAN_POINT('Ctrl Pts',(4.15757846189519,1.00257149539461,-9.59440383454691));
#14836=CARTESIAN_POINT('Ctrl Pts',(4.15142984815065,1.00633603296716,-9.59392376814036));
#14837=CARTESIAN_POINT('Ctrl Pts',(4.14054525839276,1.01286357367133,-9.5930750204444));
#14838=CARTESIAN_POINT('Ctrl Pts',(4.13582378176725,1.01565042567846,-9.59270721042155));
#14839=CARTESIAN_POINT('Ctrl Pts',(4.12594020454067,1.02139153417161,-9.5919379131431));
#14840=CARTESIAN_POINT('Ctrl Pts',(4.12077485078062,1.02433985004403,-9.59153622732433));
#14841=CARTESIAN_POINT('Ctrl Pts',(4.10724357982106,1.03192801886719,-9.59048478140566));
#14842=CARTESIAN_POINT('Ctrl Pts',(4.0988432123873,1.03650520977218,-9.5898328376858));
#14843=CARTESIAN_POINT('Ctrl Pts',(4.06320925506919,1.05536211310066,-9.58707002921739));
#14844=CARTESIAN_POINT('Ctrl Pts',(4.03547981472979,1.06867358930714,-9.58492623046284));
#14845=CARTESIAN_POINT('Ctrl Pts',(3.93086723853399,1.11394389213195,-9.57685557577604));
#14846=CARTESIAN_POINT('Ctrl Pts',(3.85118892367654,1.13880766580559,-9.57072038403955));
#14847=CARTESIAN_POINT('Ctrl Pts',(3.71835802817732,1.16526321220012,-9.56080585355076));
#14848=CARTESIAN_POINT('Ctrl Pts',(3.66651823782439,1.17204703099362,-9.55701730492824));
#14849=CARTESIAN_POINT('Ctrl Pts',(3.60744874437532,1.17580995483347,-9.55290054212497));
#14850=CARTESIAN_POINT('Ctrl Pts',(3.60049960803846,1.17619083088256,-9.55241939351805));
#14851=CARTESIAN_POINT('Ctrl Pts',(3.58988923336225,1.17667808546796,-9.55168997219977));
#14852=CARTESIAN_POINT('Ctrl Pts',(3.58623034328498,1.17682901399722,-9.55143938571454));
#14853=CARTESIAN_POINT('Ctrl Pts',(3.57953062010502,1.1770740807305,-9.55098234808661));
#14854=CARTESIAN_POINT('Ctrl Pts',(3.57649011436457,1.1771735038285,-9.55077562082111));
#14855=CARTESIAN_POINT('Ctrl Pts',(3.56962491982827,1.17737136705581,-9.55031038342588));
#14856=CARTESIAN_POINT('Ctrl Pts',(3.56580011425955,1.17746295315486,-9.55005225137544));
#14857=CARTESIAN_POINT('Ctrl Pts',(3.55591274832304,1.17765150692738,-9.54938756077394));
#14858=CARTESIAN_POINT('Ctrl Pts',(3.54984967373851,1.17772030089445,-9.54898248618808));
#14859=CARTESIAN_POINT('Ctrl Pts',(3.50913359648603,1.17786782115899,-9.54627756032263));
#14860=CARTESIAN_POINT('Ctrl Pts',(3.47448858993076,1.17646394957894,-9.54405029270586));
#14861=CARTESIAN_POINT('Ctrl Pts',(3.41185380817387,1.17114980760335,-9.54007835748678));
#14862=CARTESIAN_POINT('Ctrl Pts',(3.38384863764922,1.16775730751478,-9.53832244782797));
#14863=CARTESIAN_POINT('Ctrl Pts',(3.30862457386425,1.15589024004626,-9.53360070984589));
#14864=CARTESIAN_POINT('Ctrl Pts',(3.26175926165969,1.14553215308036,-9.53065183906796));
#14865=CARTESIAN_POINT('Ctrl Pts',(3.16436062180328,1.11767513338016,-9.52431686788137));
#14866=CARTESIAN_POINT('Ctrl Pts',(3.11412724720195,1.09953730220981,-9.52092534674652));
#14867=CARTESIAN_POINT('Ctrl Pts',(3.05538442554571,1.07369738419034,-9.51670751801753));
#14868=CARTESIAN_POINT('Ctrl Pts',(3.04552967872351,1.06919918429276,-9.51599121203832));
#14869=CARTESIAN_POINT('Ctrl Pts',(3.03011391402821,1.06190404091029,-9.51485618984739));
#14870=CARTESIAN_POINT('Ctrl Pts',(3.02451046229175,1.0591977797992,-9.51444056370144));
#14871=CARTESIAN_POINT('Ctrl Pts',(3.01405981154416,1.05404796600537,-9.51365952494999));
#14872=CARTESIAN_POINT('Ctrl Pts',(3.00920753041028,1.05161505144025,-9.51329448637314));
#14873=CARTESIAN_POINT('Ctrl Pts',(2.99838184827737,1.04609311882411,-9.51247458648246));
#14874=CARTESIAN_POINT('Ctrl Pts',(2.99241777754237,1.04298632721945,-9.51201911737847));
#14875=CARTESIAN_POINT('Ctrl Pts',(2.97730927385138,1.03495079079668,-9.51085549409399));
#14876=CARTESIAN_POINT('Ctrl Pts',(2.96820300397594,1.02995190923377,-9.51014490971284));
#14877=CARTESIAN_POINT('Ctrl Pts',(2.89349361720467,0.987644594310454,-9.50423676839299));
#14878=CARTESIAN_POINT('Ctrl Pts',(2.83156172473463,0.944236860007519,-9.49881752582396));
#14879=CARTESIAN_POINT('Ctrl Pts',(2.73027024794587,0.85764453125423,-9.48906923374195));
#14880=CARTESIAN_POINT('Ctrl Pts',(2.68914945890945,0.816890185641653,-9.4847990361949));
#14881=CARTESIAN_POINT('Ctrl Pts',(2.63773113880377,0.75782165468623,-9.47914388297175));
#14882=CARTESIAN_POINT('Ctrl Pts',(2.6246797791115,0.742013682611282,-9.47767729434716));
#14883=CARTESIAN_POINT('Ctrl Pts',(2.60400360579447,0.715595019343629,-9.47531133584986));
#14884=CARTESIAN_POINT('Ctrl Pts',(2.59613123928143,0.705184268122686,-9.47439963031944));
#14885=CARTESIAN_POINT('Ctrl Pts',(2.58566004828756,0.690847430897071,-9.47317415656299));
#14886=CARTESIAN_POINT('Ctrl Pts',(2.58290964239466,0.687033922808045,-9.47285102099374));
#14887=CARTESIAN_POINT('Ctrl Pts',(2.57834212820566,0.680620340039304,-9.47231243080403));
#14888=CARTESIAN_POINT('Ctrl Pts',(2.57651257639882,0.678029243354913,-9.47209615513099));
#14889=CARTESIAN_POINT('Ctrl Pts',(2.57305509534424,0.673090371080681,-9.4716864546784));
#14890=CARTESIAN_POINT('Ctrl Pts',(2.57142521051235,0.670744020978176,-9.47149289423685));
#14891=CARTESIAN_POINT('Ctrl Pts',(2.56756896131582,0.665149302706287,-9.47103386247538));
#14892=CARTESIAN_POINT('Ctrl Pts',(2.56535030202431,0.661895627235493,-9.47076889951872));
#14893=CARTESIAN_POINT('Ctrl Pts',(2.55754708991352,0.65032794718151,-9.4698336869106));
#14894=CARTESIAN_POINT('Ctrl Pts',(2.55205212347535,0.64195362340983,-9.46916901956574));
#14895=CARTESIAN_POINT('Ctrl Pts',(2.51285936305731,0.580529620308051,-9.46437514958382));
#14896=CARTESIAN_POINT('Ctrl Pts',(2.48334453251741,0.524921157958253,-9.46046852681187));
#14897=CARTESIAN_POINT('Ctrl Pts',(2.43273894704692,0.407822611628489,-9.45257057238299));
#14898=CARTESIAN_POINT('Ctrl Pts',(2.41201074334849,0.346418625917711,-9.44859100733336));
#14899=CARTESIAN_POINT('Ctrl Pts',(2.39104525662936,0.261921813321265,-9.44305269929184));
#14900=CARTESIAN_POINT('Ctrl Pts',(2.38627967850891,0.240070718409826,-9.44161589092358));
#14901=CARTESIAN_POINT('Ctrl Pts',(2.37911045572934,0.202025860736381,-9.43909659431812));
#14902=CARTESIAN_POINT('Ctrl Pts',(2.37641701152134,0.18589287148543,-9.43802288093174));
#14903=CARTESIAN_POINT('Ctrl Pts',(2.37300696279521,0.162474812259917,-9.43645409060667));
#14904=CARTESIAN_POINT('Ctrl Pts',(2.37202086466274,0.15523046550557,-9.43596738519616));
#14905=CARTESIAN_POINT('Ctrl Pts',(2.37041159936238,0.142523858004274,-9.43511103668022));
#14906=CARTESIAN_POINT('Ctrl Pts',(2.36975910366827,0.137065485985869,-9.43474231651561));
#14907=CARTESIAN_POINT('Ctrl Pts',(2.36848519262718,0.125736301951045,-9.4339751428557));
#14908=CARTESIAN_POINT('Ctrl Pts',(2.36786966003469,0.119864997177633,-9.43357651757802));
#14909=CARTESIAN_POINT('Ctrl Pts',(2.36639188091101,0.1046681166765,-9.43254193067574));
#14910=CARTESIAN_POINT('Ctrl Pts',(2.3655966951893,0.0953365910568731,-9.43190391317055));
#14911=CARTESIAN_POINT('Ctrl Pts',(2.36279975629333,0.0571339892772362,
-9.42928011703436));
#14912=CARTESIAN_POINT('Ctrl Pts',(2.36175133567514,0.0282054716253936,
-9.42726541018417));
#14913=CARTESIAN_POINT('Ctrl Pts',(2.36180118691856,-0.0521957103151589,
-9.42158484718462));
#14914=CARTESIAN_POINT('Ctrl Pts',(2.36520643867323,-0.103598346739239,
-9.41785828306704));
#14915=CARTESIAN_POINT('Ctrl Pts',(2.3828125307164,-0.236554346500744,-9.40804432698333));
#14916=CARTESIAN_POINT('Ctrl Pts',(2.40226129397133,-0.31713509315628,-9.40191130330289));
#14917=CARTESIAN_POINT('Ctrl Pts',(2.43308947359687,-0.403725223710294,
-9.39548061616314));
#14918=CARTESIAN_POINT('Ctrl Pts',(2.43629151458784,-0.412394813427911,
-9.39483884302727));
#14919=CARTESIAN_POINT('Ctrl Pts',(2.44104668514614,-0.424817615849938,
-9.39392312791095));
#14920=CARTESIAN_POINT('Ctrl Pts',(2.44251759767079,-0.428601630777045,
-9.39364472334985));
#14921=CARTESIAN_POINT('Ctrl Pts',(2.44513540893358,-0.435234347389366,
-9.39315774517539));
#14922=CARTESIAN_POINT('Ctrl Pts',(2.44627392441374,-0.438086278310212,
-9.3929486893714));
#14923=CARTESIAN_POINT('Ctrl Pts',(2.44871754797896,-0.444138592774605,
-9.39250577536879));
#14924=CARTESIAN_POINT('Ctrl Pts',(2.45002559763501,-0.447337707365659,
-9.39227209305574));
#14925=CARTESIAN_POINT('Ctrl Pts',(2.45364327063395,-0.456075502084081,
-9.39163489397865));
#14926=CARTESIAN_POINT('Ctrl Pts',(2.45598121074319,-0.461602455028222,
-9.39123301517199));
#14927=CARTESIAN_POINT('Ctrl Pts',(2.46894745232236,-0.491613605800345,
-9.38905595250223));
#14928=CARTESIAN_POINT('Ctrl Pts',(2.48036439077368,-0.515751049216119,
-9.38732360033491));
#14929=CARTESIAN_POINT('Ctrl Pts',(2.52201573903935,-0.596580285953777,
-9.38151747898576));
#14930=CARTESIAN_POINT('Ctrl Pts',(2.55606262982425,-0.651180232579175,
-9.3775821969801));
#14931=CARTESIAN_POINT('Ctrl Pts',(2.63810293832692,-0.761518235316816,
-9.36906438739634));
#14932=CARTESIAN_POINT('Ctrl Pts',(2.6871935351425,-0.816088320537324,-9.36448176950083));
#14933=CARTESIAN_POINT('Ctrl Pts',(2.74868686456395,-0.872804687904558,
-9.35899177817387));
#14934=CARTESIAN_POINT('Ctrl Pts',(2.75643711410827,-0.879764877200301,
-9.35830417518023));
#14935=CARTESIAN_POINT('Ctrl Pts',(2.76934752990161,-0.891053439386297,
-9.35716512789644));
#14936=CARTESIAN_POINT('Ctrl Pts',(2.77445441751921,-0.895442073605985,
-9.3567161611152));
#14937=CARTESIAN_POINT('Ctrl Pts',(2.78374609656861,-0.903289420095142,
-9.3559019919276));
#14938=CARTESIAN_POINT('Ctrl Pts',(2.78791773289922,-0.906763470837173,
-9.35553742330541));
#14939=CARTESIAN_POINT('Ctrl Pts',(2.79691761080636,-0.914153603462526,
-9.35475287079718));
#14940=CARTESIAN_POINT('Ctrl Pts',(2.8017531210579,-0.918060531639803,-9.35433253696674));
#14941=CARTESIAN_POINT('Ctrl Pts',(2.81507644145531,-0.928652084249496,
-9.35317749129558));
#14942=CARTESIAN_POINT('Ctrl Pts',(2.82362548307331,-0.935258346133828,
-9.35243974198683));
#14943=CARTESIAN_POINT('Ctrl Pts',(2.87443320916738,-0.973415160993876,
-9.34807373592682));
#14944=CARTESIAN_POINT('Ctrl Pts',(2.91867576523064,-1.00221177496292,-9.34434203850923));
#14945=CARTESIAN_POINT('Ctrl Pts',(3.03551550876267,-1.06754849481583,-9.3346709683711));
#14946=CARTESIAN_POINT('Ctrl Pts',(3.11023604222774,-1.09972469168996,-9.32864000464155));
#14947=CARTESIAN_POINT('Ctrl Pts',(3.21701658302399,-1.13315179121082,-9.32055525224378));
#14948=CARTESIAN_POINT('Ctrl Pts',(3.24671692507621,-1.14118714702618,-9.31836278747098));
#14949=CARTESIAN_POINT('Ctrl Pts',(3.28297499967284,-1.14948755786919,-9.31577908645669));
#14950=CARTESIAN_POINT('Ctrl Pts',(3.28926139259676,-1.15087254074165,-9.31533446839429));
#14951=CARTESIAN_POINT('Ctrl Pts',(3.29907110002684,-1.15294957976711,-9.31464617951545));
#14952=CARTESIAN_POINT('Ctrl Pts',(3.30258664184232,-1.15367715803208,-9.31440061567144));
#14953=CARTESIAN_POINT('Ctrl Pts',(3.30909251847901,-1.15499262458313,-9.3139482758526));
#14954=CARTESIAN_POINT('Ctrl Pts',(3.31208180398964,-1.15558498119413,-9.31374126321002));
#14955=CARTESIAN_POINT('Ctrl Pts',(3.31891784443122,-1.15691205657279,-9.31326971409797));
#14956=CARTESIAN_POINT('Ctrl Pts',(3.32276599172356,-1.15763919740886,-9.31300560240899));
#14957=CARTESIAN_POINT('Ctrl Pts',(3.33471074446141,-1.15983461287209,-9.31218972052416));
#14958=CARTESIAN_POINT('Ctrl Pts',(3.3428193717281,-1.16123727857612,-9.31164145004327));
#14959=CARTESIAN_POINT('Ctrl Pts',(3.36187580797443,-1.1643284019545,-9.31036460092272));
#14960=CARTESIAN_POINT('Ctrl Pts',(3.37283421590279,-1.16594765516191,-9.3096393402229));
#14961=CARTESIAN_POINT('Ctrl Pts',(3.41212785866392,-1.17118848494921,-9.30706563918827));
#14962=CARTESIAN_POINT('Ctrl Pts',(3.44057150054868,-1.1739338109378,-9.30525232571142));
#14963=CARTESIAN_POINT('Ctrl Pts',(3.55657605992569,-1.18088341275141,-9.2979594968495));
#14964=CARTESIAN_POINT('Ctrl Pts',(3.64437371420832,-1.17634288920514,-9.29265554749893));
#14965=CARTESIAN_POINT('Ctrl Pts',(3.76619889220178,-1.1562846776639,-9.28482404214195));
#14966=CARTESIAN_POINT('Ctrl Pts',(3.80125434139498,-1.14885693530191,-9.28251694545781));
#14967=CARTESIAN_POINT('Ctrl Pts',(3.84571300046889,-1.13729628041287,-9.27949324840693));
#14968=CARTESIAN_POINT('Ctrl Pts',(3.85547795469347,-1.13462219474938,-9.27882302194834));
#14969=CARTESIAN_POINT('Ctrl Pts',(3.87103927309664,-1.13014434332153,-9.27774460520045));
#14970=CARTESIAN_POINT('Ctrl Pts',(3.87685841569274,-1.12842104069961,-9.27733899901627));
#14971=CARTESIAN_POINT('Ctrl Pts',(3.88787815316852,-1.12506475754984,-9.27656633976162));
#14972=CARTESIAN_POINT('Ctrl Pts',(3.89308125336504,-1.12344049245383,-9.27619957670212));
#14973=CARTESIAN_POINT('Ctrl Pts',(3.90490743935773,-1.11965838896917,-9.27536142901954));
#14974=CARTESIAN_POINT('Ctrl Pts',(3.91152298094019,-1.11747780954752,-9.27488931724002));
#14975=CARTESIAN_POINT('Ctrl Pts',(3.93182250177834,-1.1105865576994,-9.27343039892889));
#14976=CARTESIAN_POINT('Ctrl Pts',(3.94543886662927,-1.10568240041257,-9.27243734030591));
#14977=CARTESIAN_POINT('Ctrl Pts',(3.99966304081146,-1.08501607301893,-9.26842265176871));
#14978=CARTESIAN_POINT('Ctrl Pts',(4.03945944623859,-1.06726260004585,-9.26533780364408));
#14979=CARTESIAN_POINT('Ctrl Pts',(4.07816930022569,-1.0473542719097,-9.26219992867132));
#14980=CARTESIAN_POINT('',(2.36176909431237,-0.000321529814770908,-9.3256328853208));
#14981=CARTESIAN_POINT('Ctrl Pts',(4.07816926754757,-1.04735428871593,-9.16390755708093));
#14982=CARTESIAN_POINT('Ctrl Pts',(4.07803365602181,-1.04742403319359,-9.16391804273648));
#14983=CARTESIAN_POINT('Ctrl Pts',(4.07789803081295,-1.04749375140339,-9.16392852686769));
#14984=CARTESIAN_POINT('Ctrl Pts',(4.07436011394742,-1.04931155080043,-9.16420194831119));
#14985=CARTESIAN_POINT('Ctrl Pts',(4.07094927920735,-1.05104310418198,-9.16446392229401));
#14986=CARTESIAN_POINT('Ctrl Pts',(4.06481132593214,-1.05412159560051,-9.1649323644239));
#14987=CARTESIAN_POINT('Ctrl Pts',(4.06208737942917,-1.05547461133838,-9.16513919621324));
#14988=CARTESIAN_POINT('Ctrl Pts',(4.05607314747128,-1.05843295930138,-9.16559353665096));
#14989=CARTESIAN_POINT('Ctrl Pts',(4.05278060306722,-1.06003351079141,-9.16584075381723));
#14990=CARTESIAN_POINT('Ctrl Pts',(4.04320957028047,-1.06463107354835,-9.16655515320663));
#14991=CARTESIAN_POINT('Ctrl Pts',(4.0369117919088,-1.06758790225852,-9.16701997442936));
#14992=CARTESIAN_POINT('Ctrl Pts',(3.98317531120304,-1.09223861877764,-9.17094473204776));
#14993=CARTESIAN_POINT('Ctrl Pts',(3.93436332591809,-1.11081750915699,-9.17423838386207));
#14994=CARTESIAN_POINT('Ctrl Pts',(3.80502510020497,-1.15043733756748,-9.18266467335368));
#14995=CARTESIAN_POINT('Ctrl Pts',(3.7232275499597,-1.16629770348424,-9.18772111356704));
#14996=CARTESIAN_POINT('Ctrl Pts',(3.60962901150093,-1.17606808574868,-9.19499248766605));
#14997=CARTESIAN_POINT('Ctrl Pts',(3.57872557685839,-1.17750334965447,-9.19699306615452));
#14998=CARTESIAN_POINT('Ctrl Pts',(3.53821988052455,-1.17778827607322,-9.19966251798157));
#14999=CARTESIAN_POINT('Ctrl Pts',(3.5286361255151,-1.17773870791541,-9.20029753959641));
#15000=CARTESIAN_POINT('Ctrl Pts',(3.51310469816021,-1.17746879049728,-9.20133268104424));
#15001=CARTESIAN_POINT('Ctrl Pts',(3.50715608936,-1.177320307798,-9.20173057751616));
#15002=CARTESIAN_POINT('Ctrl Pts',(3.49573189239385,-1.1769485023783,-9.20249759843314));
#15003=CARTESIAN_POINT('Ctrl Pts',(3.49025622436059,-1.17673202756017,-9.20286650141776));
#15004=CARTESIAN_POINT('Ctrl Pts',(3.47759192682601,-1.17614280931011,-9.20372273743164));
#15005=CARTESIAN_POINT('Ctrl Pts',(3.47040486869317,-1.175742362268,-9.20421091392577));
#15006=CARTESIAN_POINT('Ctrl Pts',(3.44752831094209,-1.1742572539103,-9.20577223109689));
#15007=CARTESIAN_POINT('Ctrl Pts',(3.4318572286,-1.17292424530377,-9.20685296344739));
#15008=CARTESIAN_POINT('Ctrl Pts',(3.3950892312141,-1.16905366391506,-9.20941616319836));
#15009=CARTESIAN_POINT('Ctrl Pts',(3.37402556140187,-1.16625822617734,-9.21090605459889));
#15010=CARTESIAN_POINT('Ctrl Pts',(3.29479064869994,-1.1535529919175,-9.21659237683874));
#15011=CARTESIAN_POINT('Ctrl Pts',(3.23732170245688,-1.13984729359774,-9.220890020222));
#15012=CARTESIAN_POINT('Ctrl Pts',(3.11353789073206,-1.10030435807032,-9.23042219550642));
#15013=CARTESIAN_POINT('Ctrl Pts',(3.0480317418016,-1.07264703085901,-9.2356529447894));
#15014=CARTESIAN_POINT('Ctrl Pts',(2.97678672734416,-1.03466075743234,-9.24131155898583));
#15015=CARTESIAN_POINT('Ctrl Pts',(2.96822120013041,-1.02995598552017,-9.24199116531814));
#15016=CARTESIAN_POINT('Ctrl Pts',(2.95632288533187,-1.02322650554734,-9.24293319159622));
#15017=CARTESIAN_POINT('Ctrl Pts',(2.95294036803041,-1.02129119210658,-9.24320076553422));
#15018=CARTESIAN_POINT('Ctrl Pts',(2.94710402790389,-1.01791335820003,-9.24366196804589));
#15019=CARTESIAN_POINT('Ctrl Pts',(2.94464573943877,-1.01647868055689,-9.24385607956485));
#15020=CARTESIAN_POINT('Ctrl Pts',(2.939504156155,-1.01345296891955,-9.24426171851963));
#15021=CARTESIAN_POINT('Ctrl Pts',(2.93682193387862,-1.01186015819009,-9.24447312584525));
#15022=CARTESIAN_POINT('Ctrl Pts',(2.93019821731662,-1.00789104887233,-9.2449947703348));
#15023=CARTESIAN_POINT('Ctrl Pts',(2.92626421424049,-1.0055022385388,-9.24530421591827));
#15024=CARTESIAN_POINT('Ctrl Pts',(2.91776737238589,-1.00027435786373,-9.2459719885778));
#15025=CARTESIAN_POINT('Ctrl Pts',(2.91320973467658,-0.997426981656927,
-9.24632980900532));
#15026=CARTESIAN_POINT('Ctrl Pts',(2.90024918673126,-0.989206036683672,
-9.24734676910381));
#15027=CARTESIAN_POINT('Ctrl Pts',(2.8918946227635,-0.98375665533815,-9.24800162297749));
#15028=CARTESIAN_POINT('Ctrl Pts',(2.86334969278014,-0.964616553637265,
-9.25024033264891));
#15029=CARTESIAN_POINT('Ctrl Pts',(2.84351498868768,-0.950404438314745,
-9.25179821053643));
#15030=CARTESIAN_POINT('Ctrl Pts',(2.78171705429099,-0.903151395934863,
-9.25670816601492));
#15031=CARTESIAN_POINT('Ctrl Pts',(2.7415523339534,-0.867868617023603,-9.25998794106046));
#15032=CARTESIAN_POINT('Ctrl Pts',(2.65191715125259,-0.7776265738463,-9.26786662277023));
#15033=CARTESIAN_POINT('Ctrl Pts',(2.60495759770233,-0.720508835282365,
-9.27248135593848));
#15034=CARTESIAN_POINT('Ctrl Pts',(2.557844514296,-0.650782446425274,-9.2780044110663));
#15035=CARTESIAN_POINT('Ctrl Pts',(2.55215034689112,-0.642110364029272,
-9.27868926237893));
#15036=CARTESIAN_POINT('Ctrl Pts',(2.54295774571561,-0.627698803335919,
-9.27982465034495));
#15037=CARTESIAN_POINT('Ctrl Pts',(2.53939248552123,-0.622002470079831,
-9.28027273671909));
#15038=CARTESIAN_POINT('Ctrl Pts',(2.53303647530488,-0.611651322778518,
-9.28108590888114));
#15039=CARTESIAN_POINT('Ctrl Pts',(2.53022876134786,-0.607007104874284,
-9.28145036723139));
#15040=CARTESIAN_POINT('Ctrl Pts',(2.5242698643067,-0.596994888325641,-9.28223534996601));
#15041=CARTESIAN_POINT('Ctrl Pts',(2.52112895080394,-0.591621001171614,
-9.28265622890078));
#15042=CARTESIAN_POINT('Ctrl Pts',(2.5126336141708,-0.576817943587628,-9.28381452192691));
#15043=CARTESIAN_POINT('Ctrl Pts',(2.507366693477,-0.567339525902516,-9.28455500285155));
#15044=CARTESIAN_POINT('Ctrl Pts',(2.47684224705872,-0.510575104527115,
-9.28898395138158));
#15045=CARTESIAN_POINT('Ctrl Pts',(2.4547099138238,-0.461688823638722,-9.29277948430495));
#15046=CARTESIAN_POINT('Ctrl Pts',(2.4032065358682,-0.3235609397052,-9.3034363420057));
#15047=CARTESIAN_POINT('Ctrl Pts',(2.38105115370269,-0.23205400477592,-9.31044613798432));
#15048=CARTESIAN_POINT('Ctrl Pts',(2.36776221812918,-0.120154030170058,
-9.31847448961641));
#15049=CARTESIAN_POINT('Ctrl Pts',(2.36598754836386,-0.1013655624945,-9.31980316502493));
#15050=CARTESIAN_POINT('Ctrl Pts',(2.36427393903611,-0.0769748602457808,
-9.32149647978916));
#15051=CARTESIAN_POINT('Ctrl Pts',(2.36392241400495,-0.0714055493996037,
-9.32188100003162));
#15052=CARTESIAN_POINT('Ctrl Pts',(2.36342249161714,-0.0624760496777101,
-9.32249388965029));
#15053=CARTESIAN_POINT('Ctrl Pts',(2.36324888538704,-0.0591174422917492,
-9.32272359107107));
#15054=CARTESIAN_POINT('Ctrl Pts',(2.36295154953094,-0.0528440087180422,
-9.32315105203661));
#15055=CARTESIAN_POINT('Ctrl Pts',(2.3628242618068,-0.0499294305659315,
-9.32334899953403));
#15056=CARTESIAN_POINT('Ctrl Pts',(2.36258555840798,-0.0439544744893212,
-9.32375351656451));
#15057=CARTESIAN_POINT('Ctrl Pts',(2.36247524638575,-0.0408940626439322,
-9.32396002639935));
#15058=CARTESIAN_POINT('Ctrl Pts',(2.36219734518225,-0.0322474474697368,
-9.32454162996615));
#15059=CARTESIAN_POINT('Ctrl Pts',(2.36205757558635,-0.0266603409708362,
-9.32491525783357));
#15060=CARTESIAN_POINT('Ctrl Pts',(2.36183421626548,-0.0141785942426367,
-9.32574550289169));
#15061=CARTESIAN_POINT('Ctrl Pts',(2.36177138964286,-0.00728375808849353,
-9.3262010936582));
#15062=CARTESIAN_POINT('Ctrl Pts',(2.36176911453502,-0.000388607634483833,
-9.32665402875837));
#15063=CARTESIAN_POINT('Ctrl Pts',(2.36176909431237,-0.000321529814770908,
-9.3256328853208));
#15064=CARTESIAN_POINT('Ctrl Pts',(2.36175642361669,0.0460906863625701,
-9.32878688485889));
#15065=CARTESIAN_POINT('Ctrl Pts',(2.36449151834104,0.0926118372533591,
-9.33194088439699));
#15066=CARTESIAN_POINT('Ctrl Pts',(2.36998689602592,0.138887012824616,-9.33509488393508));
#15067=CARTESIAN_POINT('Ctrl Pts',(2.3754744886328,0.185096632237267,-9.33824441533034));
#15068=CARTESIAN_POINT('Ctrl Pts',(2.38371456675781,0.231060407841111,-9.34139394672561));
#15069=CARTESIAN_POINT('Ctrl Pts',(2.39466767807415,0.276424307417029,-9.34454347812087));
#15070=CARTESIAN_POINT('Ctrl Pts',(2.40561027401928,0.321744656057508,-9.34768998585547));
#15071=CARTESIAN_POINT('Ctrl Pts',(2.41926061835923,0.366465719637589,-9.35083649359008));
#15072=CARTESIAN_POINT('Ctrl Pts',(2.43552796540056,0.410242302415289,-9.35398300132468));
#15073=CARTESIAN_POINT('Ctrl Pts',(2.45178712202367,0.453996844197589,-9.35712792482959));
#15074=CARTESIAN_POINT('Ctrl Pts',(2.47066047495875,0.496807316693356,-9.36027284833449));
#15075=CARTESIAN_POINT('Ctrl Pts',(2.49200790654631,0.538345117888293,-9.3634177718394));
#15076=CARTESIAN_POINT('Ctrl Pts',(2.5133705567216,0.579912531389026,-9.36656493736082));
#15077=CARTESIAN_POINT('Ctrl Pts',(2.53721055893679,0.620204951373926,-9.36971210288225));
#15078=CARTESIAN_POINT('Ctrl Pts',(2.56334109987532,0.658917044372467,-9.37285926840368));
#15079=CARTESIAN_POINT('Ctrl Pts',(2.58947920398484,0.69764034212103,-9.37600734483434));
#15080=CARTESIAN_POINT('Ctrl Pts',(2.61790882911757,0.734781945756841,-9.37915542126499));
#15081=CARTESIAN_POINT('Ctrl Pts',(2.64840110485756,0.770067444832761,-9.38230349769565));
#15082=CARTESIAN_POINT('Ctrl Pts',(2.67895463818698,0.805423830864873,-9.38545789846809));
#15083=CARTESIAN_POINT('Ctrl Pts',(2.71157870879086,0.83891625046055,-9.38861229924053));
#15084=CARTESIAN_POINT('Ctrl Pts',(2.74600665764102,0.870306351235832,-9.39176670001297));
#15085=CARTESIAN_POINT('Ctrl Pts',(2.779527135029,0.900869053876759,-9.39483795529528));
#15086=CARTESIAN_POINT('Ctrl Pts',(2.81475708886051,0.929438704869481,-9.3979092105776));
#15087=CARTESIAN_POINT('Ctrl Pts',(2.85142333164823,0.955834370748326,-9.40098046585991));
#15088=CARTESIAN_POINT('Ctrl Pts',(2.89072087851314,0.984124286432069,-9.40427212568689));
#15089=CARTESIAN_POINT('Ctrl Pts',(2.93185630826946,1.01005172441407,-9.40756378551388));
#15090=CARTESIAN_POINT('Ctrl Pts',(2.97451190062849,1.03337407708007,-9.41085544534086));
#15091=CARTESIAN_POINT('Ctrl Pts',(3.01561844267913,1.0558494716899,-9.41402756757879));
#15092=CARTESIAN_POINT('Ctrl Pts',(3.0581360867317,1.07590545684509,-9.41719968981672));
#15093=CARTESIAN_POINT('Ctrl Pts',(3.10174938394377,1.09336763332864,-9.42037181205466));
#15094=CARTESIAN_POINT('Ctrl Pts',(3.14531933553677,1.11081245481043,-9.42354078163936));
#15095=CARTESIAN_POINT('Ctrl Pts',(3.18998226970298,1.12566836352484,-9.42670975122407));
#15096=CARTESIAN_POINT('Ctrl Pts',(3.23540026985237,1.13780790549382,-9.42987872080878));
#15097=CARTESIAN_POINT('Ctrl Pts',(3.28079312827094,1.14994072745983,-9.43304593616873));
#15098=CARTESIAN_POINT('Ctrl Pts',(3.32693968692441,1.15936001758168,-9.43621315152868));
#15099=CARTESIAN_POINT('Ctrl Pts',(3.3734868825787,1.16598815677559,-9.43938036688863));
#15100=CARTESIAN_POINT('Ctrl Pts',(3.42002880465217,1.17261554503214,-9.44254722341781));
#15101=CARTESIAN_POINT('Ctrl Pts',(3.46697072159953,1.17645233371627,-9.44571407994698));
#15102=CARTESIAN_POINT('Ctrl Pts',(3.51395210476496,1.17747245988589,-9.44888093647616));
#15103=CARTESIAN_POINT('Ctrl Pts',(3.56098104504664,1.1784936186828,-9.45205099867009));
#15104=CARTESIAN_POINT('Ctrl Pts',(3.60804897288831,1.17669241563071,-9.45522106086403));
#15105=CARTESIAN_POINT('Ctrl Pts',(3.6547950087258,1.17209492616314,-9.45839112305796));
#15106=CARTESIAN_POINT('Ctrl Pts',(3.70156953762244,1.16749463439294,-9.46156311749637));
#15107=CARTESIAN_POINT('Ctrl Pts',(3.74802123333352,1.16009475239235,-9.46473511193478));
#15108=CARTESIAN_POINT('Ctrl Pts',(3.79379763126187,1.14997281090753,-9.46790710637319));
#15109=CARTESIAN_POINT('Ctrl Pts',(3.83965631247037,1.13983267518759,-9.47108480248579));
#15110=CARTESIAN_POINT('Ctrl Pts',(3.8848367398193,1.12696087545485,-9.4742624985984));
#15111=CARTESIAN_POINT('Ctrl Pts',(3.92900174489472,1.11148472468453,-9.47744019471101));
#15112=CARTESIAN_POINT('Ctrl Pts',(3.94076958281003,1.10736107897211,-9.47828689704317));
#15113=CARTESIAN_POINT('Ctrl Pts',(3.95246544776122,1.10305279483476,-9.47913359937533));
#15114=CARTESIAN_POINT('Ctrl Pts',(3.96408323881276,1.09856283954853,-9.47998030170749));
#15115=CARTESIAN_POINT('Ctrl Pts',(4.00924883554026,1.0811075841663,-9.48327196153448));
#15116=CARTESIAN_POINT('Ctrl Pts',(4.05344000235874,1.0608222044012,-9.48656362136146));
#15117=CARTESIAN_POINT('Ctrl Pts',(4.09627994886804,1.03784024033695,-9.48985528118844));
#15118=CARTESIAN_POINT('Ctrl Pts',(4.13756422331136,1.01569283379271,-9.49302740904442));
#15119=CARTESIAN_POINT('Ctrl Pts',(4.17759319139836,0.991041627729338,-9.49619953690041));
#15120=CARTESIAN_POINT('Ctrl Pts',(4.21604842842676,0.964055529104958,-9.4993716647564));
#15121=CARTESIAN_POINT('Ctrl Pts',(4.25446544669328,0.937096250631923,-9.50254063999109));
#15122=CARTESIAN_POINT('Ctrl Pts',(4.29131137513436,0.907806991346767,-9.50570961522578));
#15123=CARTESIAN_POINT('Ctrl Pts',(4.32629483075051,0.876401126191668,-9.50887859046048));
#15124=CARTESIAN_POINT('Ctrl Pts',(4.36125892107534,0.845012645932292,-9.51204581149086));
#15125=CARTESIAN_POINT('Ctrl Pts',(4.39436216662497,0.811510252606919,-9.51521303252124));
#15126=CARTESIAN_POINT('Ctrl Pts',(4.42534664645601,0.776147236422549,-9.51838025355162));
#15127=CARTESIAN_POINT('Ctrl Pts',(4.45632761598408,0.740788226595598,-9.52154711576025));
#15128=CARTESIAN_POINT('Ctrl Pts',(4.48518993070384,0.703569432955103,-9.52471397796888));
#15129=CARTESIAN_POINT('Ctrl Pts',(4.5117147702804,0.664778568239782,-9.52788084017751));
#15130=CARTESIAN_POINT('Ctrl Pts',(4.53826645945181,0.625948437726135,-9.53105090802163));
#15131=CARTESIAN_POINT('Ctrl Pts',(4.56247563863267,0.585543522958146,-9.53422097586575));
#15132=CARTESIAN_POINT('Ctrl Pts',(4.58416696305745,0.543880318754466,-9.53739104370988));
#15133=CARTESIAN_POINT('Ctrl Pts',(4.6058715088721,0.502191719814401,-9.54056304378746));
#15134=CARTESIAN_POINT('Ctrl Pts',(4.62505491865147,0.459243814517834,-9.54373504386505));
#15135=CARTESIAN_POINT('Ctrl Pts',(4.64158954073585,0.41537416491831,-9.54690704394264));
#15136=CARTESIAN_POINT('Ctrl Pts',(4.65815388344539,0.371425660573533,-9.55008474562168));
#15137=CARTESIAN_POINT('Ctrl Pts',(4.67205977932429,0.326552639882582,-9.55326244730071));
#15138=CARTESIAN_POINT('Ctrl Pts',(4.68322962843374,0.281107054778652,-9.55644014897975));
#15139=CARTESIAN_POINT('Ctrl Pts',(4.68620570905126,0.268998589959227,-9.55728681183819));
#15140=CARTESIAN_POINT('Ctrl Pts',(4.68898784233463,0.256849522602019,-9.55813347469662));
#15141=CARTESIAN_POINT('Ctrl Pts',(4.69157518003766,0.244666582755543,-9.55898013755506));
#15142=CARTESIAN_POINT('Ctrl Pts',(4.70163424367916,0.197301692152735,-9.56227179738204));
#15143=CARTESIAN_POINT('Ctrl Pts',(4.70879057834815,0.149206535139714,-9.56556345720902));
#15144=CARTESIAN_POINT('Ctrl Pts',(4.71295014754609,0.100769652199884,-9.568855117036));
#15145=CARTESIAN_POINT('Ctrl Pts',(4.71695864328854,0.0540919724203997,
-9.57202722543814));
#15146=CARTESIAN_POINT('Ctrl Pts',(4.71818427734087,0.0070975774068678,
-9.57519933384028));
#15147=CARTESIAN_POINT('Ctrl Pts',(4.71659452666535,-0.0398545571900941,
-9.57837144224242));
#15148=CARTESIAN_POINT('Ctrl Pts',(4.71500635595994,-0.0867600285145284,
-9.58154039805181));
#15149=CARTESIAN_POINT('Ctrl Pts',(4.71060835732731,-0.13362276774729,-9.58470935386121));
#15150=CARTESIAN_POINT('Ctrl Pts',(4.7034200263374,-0.180082150046841,-9.5878783096706));
#15151=CARTESIAN_POINT('Ctrl Pts',(4.69623567436311,-0.22651581530468,-9.59104551134198));
#15152=CARTESIAN_POINT('Ctrl Pts',(4.68626413475648,-0.272546015795528,
-9.59421271301336));
#15153=CARTESIAN_POINT('Ctrl Pts',(4.67357661674705,-0.317818342395695,
-9.59737991468474));
#15154=CARTESIAN_POINT('Ctrl Pts',(4.66089053572761,-0.363085541446122,
-9.60054675763843));
#15155=CARTESIAN_POINT('Ctrl Pts',(4.64548923945076,-0.407594500986334,
-9.60371360059213));
#15156=CARTESIAN_POINT('Ctrl Pts',(4.62749413136536,-0.451004751359048,
-9.60688044354582));
#15157=CARTESIAN_POINT('Ctrl Pts',(4.60948080606262,-0.494458947784328,
-9.61005049243005));
#15158=CARTESIAN_POINT('Ctrl Pts',(4.58886864511359,-0.536811700499529,
-9.61322054131427));
#15159=CARTESIAN_POINT('Ctrl Pts',(4.56582691260045,-0.577743225432142,
-9.61639059019849));
#15160=CARTESIAN_POINT('Ctrl Pts',(4.5427711344045,-0.618699701232303,-9.61956257146784));
#15161=CARTESIAN_POINT('Ctrl Pts',(4.51728313985576,-0.658232756603897,
-9.62273455273718));
#15162=CARTESIAN_POINT('Ctrl Pts',(4.48957589663132,-0.696051040853093,
-9.62590653400653));
#15163=CARTESIAN_POINT('Ctrl Pts',(4.4618188463756,-0.733937307920058,-9.6290842172856));
#15164=CARTESIAN_POINT('Ctrl Pts',(4.43183494754508,-0.770102228310919,
-9.63226190056467));
#15165=CARTESIAN_POINT('Ctrl Pts',(4.3998765676401,-0.804288508601244,-9.63543958384374));
#15166=CARTESIAN_POINT('Ctrl Pts',(4.3913602233415,-0.813398549038413,-9.63628638036337));
#15167=CARTESIAN_POINT('Ctrl Pts',(4.38270385701534,-0.822368294345101,
-9.637133176883));
#15168=CARTESIAN_POINT('Ctrl Pts',(4.37391264430216,-0.831193354757727,
-9.63797997340262));
#15169=CARTESIAN_POINT('Ctrl Pts',(4.34092324961172,-0.864309764360973,
-9.64115761288422));
#15170=CARTESIAN_POINT('Ctrl Pts',(4.30588605809058,-0.895532622737997,
-9.6443352523658));
#15171=CARTESIAN_POINT('Ctrl Pts',(4.269046890181,-0.924599477351144,-9.6475128918474));
#15172=CARTESIAN_POINT('Ctrl Pts',(4.23226979794983,-0.953617352988332,
-9.65068517686151));
#15173=CARTESIAN_POINT('Ctrl Pts',(4.19369717942832,-0.980486080284995,
-9.65385746187562));
#15174=CARTESIAN_POINT('Ctrl Pts',(4.15361073600015,-1.00498082777981,-9.65702974688973));
#15175=CARTESIAN_POINT('Ctrl Pts',(4.1290093564398,-1.02001345549184,-9.65897660425675));
#15176=CARTESIAN_POINT('Ctrl Pts',(4.10383852032893,-1.0341526923382,-9.66092346162377));
#15177=CARTESIAN_POINT('Ctrl Pts',(4.07816926754759,-1.04735428871592,-9.66287031899079));
#15178=CARTESIAN_POINT('Origin',(3.53951905042299,8.32667268468867E-16,
0.924367114736157));
#15179=CARTESIAN_POINT('',(4.07816926754758,-1.04735428871592,-10.2615635160918));
#15180=CARTESIAN_POINT('',(4.07816926754651,-1.04735428871647,-10.1620324047392));
#15181=CARTESIAN_POINT('',(4.07816926754759,-1.04735428871592,0.924367114736157));
#15182=CARTESIAN_POINT('',(2.36176949287335,0.00102087787044271,-9.92436711477312));
#15183=CARTESIAN_POINT('Ctrl Pts',(2.36176949287335,0.00102087787044271,
-9.92436711477312));
#15184=CARTESIAN_POINT('Ctrl Pts',(2.36181953356955,0.0587510035938087,
-9.92826181891225));
#15185=CARTESIAN_POINT('Ctrl Pts',(2.36611819363635,0.11629608653358,-9.93215652305138));
#15186=CARTESIAN_POINT('Ctrl Pts',(2.3745609312197,0.173111648950421,-9.9360512271905));
#15187=CARTESIAN_POINT('Ctrl Pts',(2.38247315541436,0.226357111473627,-9.93970120114935));
#15188=CARTESIAN_POINT('Ctrl Pts',(2.39402444443252,0.278962151827222,-9.9433511751082));
#15189=CARTESIAN_POINT('Ctrl Pts',(2.4090909796731,0.330495747870812,-9.94700114906705));
#15190=CARTESIAN_POINT('Ctrl Pts',(2.42267844888313,0.376970344607428,-9.95029280889403));
#15191=CARTESIAN_POINT('Ctrl Pts',(2.43916788388295,0.422712270937087,-9.95358446872101));
#15192=CARTESIAN_POINT('Ctrl Pts',(2.45845795274245,0.46733496079551,-9.95687612854799));
#15193=CARTESIAN_POINT('Ctrl Pts',(2.47705158102658,0.510346611728898,-9.96004894766578));
#15194=CARTESIAN_POINT('Ctrl Pts',(2.49824681331542,0.552317904399127,-9.96322176678355));
#15195=CARTESIAN_POINT('Ctrl Pts',(2.52190210798983,0.592917212579454,-9.96639458590133));
#15196=CARTESIAN_POINT('Ctrl Pts',(2.5455338523531,0.633476101633617,-9.96956424628115));
#15197=CARTESIAN_POINT('Ctrl Pts',(2.57162053225186,0.672665230260555,-9.97273390666096));
#15198=CARTESIAN_POINT('Ctrl Pts',(2.59997401872786,0.710176172450892,-9.97590356704077));
#15199=CARTESIAN_POINT('Ctrl Pts',(2.62831174726544,0.747666267289082,-9.97907146582724));
#15200=CARTESIAN_POINT('Ctrl Pts',(2.65891345126779,0.783479579408872,-9.98223936461371));
#15201=CARTESIAN_POINT('Ctrl Pts',(2.69154840817892,0.817337661185501,-9.98540726340017));
#15202=CARTESIAN_POINT('Ctrl Pts',(2.72417957927749,0.851191815261177,-9.98857479469509));
#15203=CARTESIAN_POINT('Ctrl Pts',(2.75884314694137,0.883090789708585,-9.99174232599001));
#15204=CARTESIAN_POINT('Ctrl Pts',(2.79527079042507,0.912792194308251,-9.99490985728492));
#15205=CARTESIAN_POINT('Ctrl Pts',(2.83173509727546,0.942523492510248,-9.99808057660822));
#15206=CARTESIAN_POINT('Ctrl Pts',(2.86996658891186,0.970052456226129,-10.0012512959315));
#15207=CARTESIAN_POINT('Ctrl Pts',(2.90966459695419,0.995177587139862,-10.0044220152548));
#15208=CARTESIAN_POINT('Ctrl Pts',(2.94938667711143,1.02031795345377,-10.0075946572418));
#15209=CARTESIAN_POINT('Ctrl Pts',(2.99057655522839,1.04305131694122,-10.0107672992288));
#15210=CARTESIAN_POINT('Ctrl Pts',(3.03290854097937,1.06322192143563,-10.0139399412159));
#15211=CARTESIAN_POINT('Ctrl Pts',(3.07531633179523,1.08342864599281,-10.0171182645412));
#15212=CARTESIAN_POINT('Ctrl Pts',(3.11886979281923,1.10106325107664,-10.0202965878665));
#15213=CARTESIAN_POINT('Ctrl Pts',(3.1632246654204,1.11601863708252,-10.0234749111918));
#15214=CARTESIAN_POINT('Ctrl Pts',(3.1749754814627,1.11998072691596,-10.0243169357661));
#15215=CARTESIAN_POINT('Ctrl Pts',(3.18678247904297,1.12375504775244,-10.0251589603403));
#15216=CARTESIAN_POINT('Ctrl Pts',(3.19863913383181,1.12734020817355,-10.0260009849146));
#15217=CARTESIAN_POINT('Ctrl Pts',(3.24498941319832,1.14135539121225,-10.0292926447416));
#15218=CARTESIAN_POINT('Ctrl Pts',(3.29231139987383,1.15253933461149,-10.0325843045686));
#15219=CARTESIAN_POINT('Ctrl Pts',(3.3402259338014,1.16076583175387,-10.0358759643956));
#15220=CARTESIAN_POINT('Ctrl Pts',(3.38641503190162,1.16869608698927,-10.0390490892535));
#15221=CARTESIAN_POINT('Ctrl Pts',(3.43315411987754,1.17387817845893,-10.0422222141114));
#15222=CARTESIAN_POINT('Ctrl Pts',(3.48008801368417,1.17624955446204,-10.0453953389693));
#15223=CARTESIAN_POINT('Ctrl Pts',(3.52697541066531,1.1786185811724,-10.0485653202519));
#15224=CARTESIAN_POINT('Ctrl Pts',(3.57405667746869,1.17818237585373,-10.0517353015344));
#15225=CARTESIAN_POINT('Ctrl Pts',(3.62097062587361,1.17493008445465,-10.0549052828169));
#15226=CARTESIAN_POINT('Ctrl Pts',(3.66785871588435,1.17167958567879,-10.0580735168446));
#15227=CARTESIAN_POINT('Ctrl Pts',(3.7145791152668,1.16561611412995,-10.0612417508722));
#15228=CARTESIAN_POINT('Ctrl Pts',(3.7607724888495,1.15678086882713,-10.0644099848999));
#15229=CARTESIAN_POINT('Ctrl Pts',(3.80696070168783,1.14794661060187,-10.067577864971));
#15230=CARTESIAN_POINT('Ctrl Pts',(3.85262145907468,1.13634130014388,-10.0707457450422));
#15231=CARTESIAN_POINT('Ctrl Pts',(3.89740509739597,1.12205732468625,-10.0739136251133));
#15232=CARTESIAN_POINT('Ctrl Pts',(3.94223404549111,1.10775889743948,-10.077084710282));
#15233=CARTESIAN_POINT('Ctrl Pts',(3.9861835727123,1.09077656889708,-10.0802557954507));
#15234=CARTESIAN_POINT('Ctrl Pts',(4.02892060096838,1.07125215744183,-10.0834268806194));
#15235=CARTESIAN_POINT('Ctrl Pts',(4.07168368041955,1.05171584449803,-10.0865998987853));
#15236=CARTESIAN_POINT('Ctrl Pts',(4.11323229801876,1.02963462662897,-10.0897729169513));
#15237=CARTESIAN_POINT('Ctrl Pts',(4.15325802535948,1.00519626598188,-10.0929459351172));
#15238=CARTESIAN_POINT('Ctrl Pts',(4.19335555928565,0.98071406265287,-10.0961246457119));
#15239=CARTESIAN_POINT('Ctrl Pts',(4.23192429809895,0.953866601677069,-10.0993033563066));
#15240=CARTESIAN_POINT('Ctrl Pts',(4.26868642707439,0.924883776118556,-10.1024820669012));
#15241=CARTESIAN_POINT('Ctrl Pts',(4.27839631326216,0.917228617252182,-10.1033216515216));
#15242=CARTESIAN_POINT('Ctrl Pts',(4.28798035801678,0.909424693745959,-10.1041612361419));
#15243=CARTESIAN_POINT('Ctrl Pts',(4.29743387338196,0.901476668383086,-10.1050008207622));
#15244=CARTESIAN_POINT('Ctrl Pts',(4.33449714967136,0.870315788160264,-10.1082924805892));
#15245=CARTESIAN_POINT('Ctrl Pts',(4.36972230568576,0.8367923660712,-10.1115841404162));
#15246=CARTESIAN_POINT('Ctrl Pts',(4.40279526343513,0.801154942908937,-10.1148758002431));
#15247=CARTESIAN_POINT('Ctrl Pts',(4.43462101281622,0.766861436209441,-10.1180433288777));
#15248=CARTESIAN_POINT('Ctrl Pts',(4.46445357566618,0.73061098662132,-10.1212108575123));
#15249=CARTESIAN_POINT('Ctrl Pts',(4.4920468384816,0.692665774725574,-10.1243783861469));
#15250=CARTESIAN_POINT('Ctrl Pts',(4.51961266769324,0.654758288484654,-10.1275427655807));
#15251=CARTESIAN_POINT('Ctrl Pts',(4.54494327521734,0.615159824770047,-10.1307071450144));
#15252=CARTESIAN_POINT('Ctrl Pts',(4.56783251589978,0.574165898690546,-10.1338715244482));
#15253=CARTESIAN_POINT('Ctrl Pts',(4.59070915590108,0.533194540043413,-10.1370341618698));
#15254=CARTESIAN_POINT('Ctrl Pts',(4.61114681879182,0.490829728170074,-10.1401967992914));
#15255=CARTESIAN_POINT('Ctrl Pts',(4.62898394364436,0.447393908025294,-10.143359436713));
#15256=CARTESIAN_POINT('Ctrl Pts',(4.64681916300776,0.403962728005233,-10.146521736279));
#15257=CARTESIAN_POINT('Ctrl Pts',(4.66205418551195,0.359461284843025,-10.1496840358451));
#15258=CARTESIAN_POINT('Ctrl Pts',(4.6745755997863,0.314231908385285,-10.1528463354111));
#15259=CARTESIAN_POINT('Ctrl Pts',(4.68710996144185,0.26895576388955,-10.1560119048552));
#15260=CARTESIAN_POINT('Ctrl Pts',(4.69692496872652,0.222950724747961,-10.1591774742994));
#15261=CARTESIAN_POINT('Ctrl Pts',(4.70395767352118,0.176572238863296,-10.1623430437435));
#15262=CARTESIAN_POINT('Ctrl Pts',(4.71099474300782,0.130164969201755,-10.165510577828));
#15263=CARTESIAN_POINT('Ctrl Pts',(4.71524602425287,0.0833843488712431,
-10.1686781119124));
#15264=CARTESIAN_POINT('Ctrl Pts',(4.71670052190024,0.0365902406477502,
-10.1718456459969));
#15265=CARTESIAN_POINT('Ctrl Pts',(4.71815767980926,-0.0102894535315625,
-10.1750189734695));
#15266=CARTESIAN_POINT('Ctrl Pts',(4.71680787049338,-0.0571821265167829,
-10.1781923009422));
#15267=CARTESIAN_POINT('Ctrl Pts',(4.71269210976297,-0.103730590178981,
-10.1813656284148));
#15268=CARTESIAN_POINT('Ctrl Pts',(4.71155291169594,-0.116614701598565,
-10.1822439711464));
#15269=CARTESIAN_POINT('Ctrl Pts',(4.71020211070252,-0.1294724971845,-10.1831223138781));
#15270=CARTESIAN_POINT('Ctrl Pts',(4.70864126534676,-0.142296553267261,
-10.1840006566098));
#15271=CARTESIAN_POINT('Ctrl Pts',(4.70289827039364,-0.189481554068203,
-10.1872324424215));
#15272=CARTESIAN_POINT('Ctrl Pts',(4.69428146431621,-0.236422911045137,
-10.1904642282333));
#15273=CARTESIAN_POINT('Ctrl Pts',(4.68282581482345,-0.282744946862258,
-10.193696014045));
#15274=CARTESIAN_POINT('Ctrl Pts',(4.67156026021599,-0.328298315473704,
-10.1968741716488));
#15275=CARTESIAN_POINT('Ctrl Pts',(4.65754948265448,-0.373252197257797,
-10.2000523292526));
#15276=CARTESIAN_POINT('Ctrl Pts',(4.64087870123871,-0.417255296018016,
-10.2032304868564));
#15277=CARTESIAN_POINT('Ctrl Pts',(4.62422490200448,-0.461213569728162,
-10.2064054069366));
#15278=CARTESIAN_POINT('Ctrl Pts',(4.60491665903401,-0.504222460847839,
-10.2095803270167));
#15279=CARTESIAN_POINT('Ctrl Pts',(4.5830889618682,-0.545945878660368,-10.2127552470968));
#15280=CARTESIAN_POINT('Ctrl Pts',(4.56127398657655,-0.587644978741763,
-10.2159283167329));
#15281=CARTESIAN_POINT('Ctrl Pts',(4.53694272347648,-0.628059598796641,
-10.2191013863689));
#15282=CARTESIAN_POINT('Ctrl Pts',(4.51027712176019,-0.666876172489078,
-10.2222744560049));
#15283=CARTESIAN_POINT('Ctrl Pts',(4.48276258672367,-0.706928521137399,
-10.2255485443455));
#15284=CARTESIAN_POINT('Ctrl Pts',(4.45276281347156,-0.745278770559472,
-10.228822632686));
#15285=CARTESIAN_POINT('Ctrl Pts',(4.42052580014014,-0.78161510313761,-10.2320967210266));
#15286=CARTESIAN_POINT('Ctrl Pts',(4.3892593963524,-0.816857401636967,-10.2352722313334));
#15287=CARTESIAN_POINT('Ctrl Pts',(4.3558890494958,-0.850204999571246,-10.2384477416401));
#15288=CARTESIAN_POINT('Ctrl Pts',(4.32067953260879,-0.88140987263092,-10.2416232519469));
#15289=CARTESIAN_POINT('Ctrl Pts',(4.28383049107333,-0.914067794839122,
-10.2449466293044));
#15290=CARTESIAN_POINT('Ctrl Pts',(4.24496726564072,-0.944378053767438,
-10.2482700066618));
#15291=CARTESIAN_POINT('Ctrl Pts',(4.20443028105735,-0.972104993236993,
-10.2515933840193));
#15292=CARTESIAN_POINT('Ctrl Pts',(4.16389329647398,-0.999831932706549,
-10.2549167613768));
#15293=CARTESIAN_POINT('Ctrl Pts',(4.12168317836847,-1.02497525445393,-10.2582401387343));
#15294=CARTESIAN_POINT('Ctrl Pts',(4.07816926754758,-1.04735428871592,-10.2615635160918));
#15295=CARTESIAN_POINT('Ctrl Pts',(2.36176947427292,0.000999188840285452,
-9.92471602642876));
#15296=CARTESIAN_POINT('Ctrl Pts',(2.36171985495268,-0.0574873864968981,
-9.92108038399836));
#15297=CARTESIAN_POINT('Ctrl Pts',(2.36602676942147,-0.115891305276079,
-9.91739771552307));
#15298=CARTESIAN_POINT('Ctrl Pts',(2.37613384376762,-0.183659141572686,
-9.91292448630051));
#15299=CARTESIAN_POINT('Ctrl Pts',(2.37774134962737,-0.193567516473714,
-9.91226553567381));
#15300=CARTESIAN_POINT('Ctrl Pts',(2.38060667704903,-0.209904904468701,
-9.91117023956932));
#15301=CARTESIAN_POINT('Ctrl Pts',(2.3817918569559,-0.216346251945307,-9.91073612887373));
#15302=CARTESIAN_POINT('Ctrl Pts',(2.38401615399669,-0.227893092503701,
-9.90995369002595));
#15303=CARTESIAN_POINT('Ctrl Pts',(2.38503554800162,-0.233002245542662,
-9.90960598394544));
#15304=CARTESIAN_POINT('Ctrl Pts',(2.38718478374653,-0.243413617835199,
-9.90889428461842));
#15305=CARTESIAN_POINT('Ctrl Pts',(2.38831740243396,-0.248715129197281,
-9.90853021179256));
#15306=CARTESIAN_POINT('Ctrl Pts',(2.39083032104041,-0.260092454666618,
-9.90774520196162));
#15307=CARTESIAN_POINT('Ctrl Pts',(2.39222230963744,-0.266165489856491,
-9.90732390459827));
#15308=CARTESIAN_POINT('Ctrl Pts',(2.39611373268057,-0.282545244363976,
-9.90618131584407));
#15309=CARTESIAN_POINT('Ctrl Pts',(2.39870425299437,-0.292829508341833,
-9.90545715702933));
#15310=CARTESIAN_POINT('Ctrl Pts',(2.412913361162,-0.346186177086252,-9.90166368125109));
#15311=CARTESIAN_POINT('Ctrl Pts',(2.42683209708736,-0.388602766155844,
-9.89852178737399));
#15312=CARTESIAN_POINT('Ctrl Pts',(2.45979983240075,-0.472638530044206,
-9.89203959553921));
#15313=CARTESIAN_POINT('Ctrl Pts',(2.47893640772502,-0.51414463458435,-9.88870171058853));
#15314=CARTESIAN_POINT('Ctrl Pts',(2.51827352045945,-0.587868078467815,
-9.88257008750968));
#15315=CARTESIAN_POINT('Ctrl Pts',(2.53771801808256,-0.620424161851659,
-9.87978432708926));
#15316=CARTESIAN_POINT('Ctrl Pts',(2.57882726402113,-0.682267112639189,
-9.87439360672218));
#15317=CARTESIAN_POINT('Ctrl Pts',(2.60034945991651,-0.711602532803979,
-9.87178881143956));
#15318=CARTESIAN_POINT('Ctrl Pts',(2.62737382128112,-0.745070701398977,
-9.86879952549719));
#15319=CARTESIAN_POINT('Ctrl Pts',(2.63159465256203,-0.750208345752129,
-9.86834014864454));
#15320=CARTESIAN_POINT('Ctrl Pts',(2.63816368885226,-0.758067602860315,
-9.86763700759519));
#15321=CARTESIAN_POINT('Ctrl Pts',(2.64048113861525,-0.760814571587972,
-9.86739116662242));
#15322=CARTESIAN_POINT('Ctrl Pts',(2.6447856478766,-0.765869751563662,-9.86693867331643));
#15323=CARTESIAN_POINT('Ctrl Pts',(2.64676908223398,-0.768180859327639,
-9.86673178148662));
#15324=CARTESIAN_POINT('Ctrl Pts',(2.65131666329256,-0.773438321231054,
-9.86626104769743));
#15325=CARTESIAN_POINT('Ctrl Pts',(2.65388651937638,-0.776379635423801,
-9.86599762577208));
#15326=CARTESIAN_POINT('Ctrl Pts',(2.66065884799994,-0.78405348233827,-9.86531001466876));
#15327=CARTESIAN_POINT('Ctrl Pts',(2.66488498542338,-0.788765095088173,
-9.86488748374285));
#15328=CARTESIAN_POINT('Ctrl Pts',(2.699002108824,-0.826190013230937,-9.86152625311498));
#15329=CARTESIAN_POINT('Ctrl Pts',(2.73068340761933,-0.857230733093855,
-9.85870690131269));
#15330=CARTESIAN_POINT('Ctrl Pts',(2.80454029338702,-0.921844111327772,
-9.85256218201608));
#15331=CARTESIAN_POINT('Ctrl Pts',(2.84741896244193,-0.95445695610894,-9.84926337956484));
#15332=CARTESIAN_POINT('Ctrl Pts',(2.92853813529274,-1.00780476468787,-9.84323059024306));
#15333=CARTESIAN_POINT('Ctrl Pts',(2.96597879804629,-1.02957236508432,-9.84051764285344));
#15334=CARTESIAN_POINT('Ctrl Pts',(3.02021786676085,-1.05722818015854,-9.83661112625502));
#15335=CARTESIAN_POINT('Ctrl Pts',(3.03608219309112,-1.06487390175581,-9.83547144438125));
#15336=CARTESIAN_POINT('Ctrl Pts',(3.0643908576592,-1.07774310988006,-9.83343840158799));
#15337=CARTESIAN_POINT('Ctrl Pts',(3.07676491471131,-1.08311384263397,-9.83254995348445));
#15338=CARTESIAN_POINT('Ctrl Pts',(3.09530114928997,-1.09078353273428,-9.83121804560526));
#15339=CARTESIAN_POINT('Ctrl Pts',(3.1013950368387,-1.09324544579801,-9.83078001515608));
#15340=CARTESIAN_POINT('Ctrl Pts',(3.10754343191573,-1.09566971705732,-9.83033782098026));
#15341=CARTESIAN_POINT('Ctrl Pts',(3.10757775536683,-1.09568324870211,-9.83033535242107));
#15342=CARTESIAN_POINT('Ctrl Pts',(3.1076483549733,-1.09571107799099,-9.8303302748475));
#15343=CARTESIAN_POINT('Ctrl Pts',(3.10768463120147,-1.09572537544587,-9.830327665827));
#15344=CARTESIAN_POINT('Ctrl Pts',(3.10775925492901,-1.09575478241887,-9.83032229880059));
#15345=CARTESIAN_POINT('Ctrl Pts',(3.1077976025227,-1.09576989172988,-9.83031954078689));
#15346=CARTESIAN_POINT('Ctrl Pts',(3.10787649559497,-1.09580097155484,-9.83031386666474));
#15347=CARTESIAN_POINT('Ctrl Pts',(3.10791704115353,-1.0958169418263,-9.8303109505494));
#15348=CARTESIAN_POINT('Ctrl Pts',(3.10800046529989,-1.09584979596521,-9.83030495050062));
#15349=CARTESIAN_POINT('Ctrl Pts',(3.10804334399795,-1.09586667956857,-9.83030186655797));
#15350=CARTESIAN_POINT('Ctrl Pts',(3.10813157885383,-1.09590141630034,-9.83029552046282));
#15351=CARTESIAN_POINT('Ctrl Pts',(3.10817693513293,-1.09591926913118,-9.83029225830016));
#15352=CARTESIAN_POINT('Ctrl Pts',(3.10827027958136,-1.09595600404714,-9.83028554465343));
#15353=CARTESIAN_POINT('Ctrl Pts',(3.10831826787693,-1.09597488579395,-9.83028209315867));
#15354=CARTESIAN_POINT('Ctrl Pts',(3.10841704153571,-1.0960137423461,-9.83027498896254));
#15355=CARTESIAN_POINT('Ctrl Pts',(3.10846782704737,-1.09603371677359,-9.83027133624868));
#15356=CARTESIAN_POINT('Ctrl Pts',(3.10857237196038,-1.0960748268977,-9.83026381689092));
#15357=CARTESIAN_POINT('Ctrl Pts',(3.10862613152371,-1.0960959621672,-9.8302599502333));
#15358=CARTESIAN_POINT('Ctrl Pts',(3.1087368138989,-1.09613946691829,-9.830251989362));
#15359=CARTESIAN_POINT('Ctrl Pts',(3.10879373690068,-1.09616183592192,-9.83024789513233));
#15360=CARTESIAN_POINT('Ctrl Pts',(3.10891094908999,-1.09620788619768,-9.83023946451329));
#15361=CARTESIAN_POINT('Ctrl Pts',(3.108971238489,-1.09623156693029,-9.83023512810609));
#15362=CARTESIAN_POINT('Ctrl Pts',(3.1090954010752,-1.09628032422859,-9.83022619747242));
#15363=CARTESIAN_POINT('Ctrl Pts',(3.10915927449812,-1.09630540018487,-9.83022160322605));
#15364=CARTESIAN_POINT('Ctrl Pts',(3.10929083859044,-1.09635703743392,-9.83021214011275));
#15365=CARTESIAN_POINT('Ctrl Pts',(3.10935852952489,-1.09638359803866,-9.83020727122342));
#15366=CARTESIAN_POINT('Ctrl Pts',(3.10949797923664,-1.09643830048801,-9.83019724078879));
#15367=CARTESIAN_POINT('Ctrl Pts',(3.10956973831804,-1.0964664415575,-9.83019207921782));
#15368=CARTESIAN_POINT('Ctrl Pts',(3.11420107955089,-1.09828214559106,-9.82985894846596));
#15369=CARTESIAN_POINT('Ctrl Pts',(3.11877170467261,-1.10004123444432,-9.82953004497875));
#15370=CARTESIAN_POINT('Ctrl Pts',(3.12909485118052,-1.10394053754667,-9.82878680423127));
#15371=CARTESIAN_POINT('Ctrl Pts',(3.1348533622849,-1.10606437974786,-9.82837193837223));
#15372=CARTESIAN_POINT('Ctrl Pts',(3.15044324331368,-1.11167616606449,-9.82724792050189));
#15373=CARTESIAN_POINT('Ctrl Pts',(3.16030459128452,-1.11507859082579,-9.82653600192459));
#15374=CARTESIAN_POINT('Ctrl Pts',(3.20818679353909,-1.13089059927671,-9.82307386110841));
#15375=CARTESIAN_POINT('Ctrl Pts',(3.24677388441622,-1.14148772953117,-9.82026618572278));
#15376=CARTESIAN_POINT('Ctrl Pts',(3.36770775654436,-1.16816419057322,-9.81141165563014));
#15377=CARTESIAN_POINT('Ctrl Pts',(3.45128491175312,-1.17742896249921,-9.80519607767987));
#15378=CARTESIAN_POINT('Ctrl Pts',(3.56296907476481,-1.17784570040957,-9.79706445952686));
#15379=CARTESIAN_POINT('Ctrl Pts',(3.59081057252225,-1.17696209914155,-9.79505415112404));
#15380=CARTESIAN_POINT('Ctrl Pts',(3.62946521644012,-1.17436085550939,-9.79230689377025));
#15381=CARTESIAN_POINT('Ctrl Pts',(3.64032394472411,-1.173478642301,-9.79154000090286));
#15382=CARTESIAN_POINT('Ctrl Pts',(3.65925690341835,-1.17167568538445,-9.79021305861677));
#15383=CARTESIAN_POINT('Ctrl Pts',(3.66733661464515,-1.17082182443387,-9.78965003199249));
#15384=CARTESIAN_POINT('Ctrl Pts',(3.67927879441322,-1.16943467905838,-9.7888232889936));
#15385=CARTESIAN_POINT('Ctrl Pts',(3.68314828502214,-1.16896573888598,-9.78855625530948));
#15386=CARTESIAN_POINT('Ctrl Pts',(3.69003885347894,-1.16809594556067,-9.78808233029557));
#15387=CARTESIAN_POINT('Ctrl Pts',(3.69306077501046,-1.16770256858485,-9.78787503813181));
#15388=CARTESIAN_POINT('Ctrl Pts',(3.69965590172444,-1.1668180061097,-9.78742385308767));
#15389=CARTESIAN_POINT('Ctrl Pts',(3.70322839545239,-1.16632213463915,-9.78718022116522));
#15390=CARTESIAN_POINT('Ctrl Pts',(3.71324223751461,-1.16488526984143,-9.78649932710392));
#15391=CARTESIAN_POINT('Ctrl Pts',(3.71967826518759,-1.16390725563635,-9.78606405020752));
#15392=CARTESIAN_POINT('Ctrl Pts',(3.7578224088654,-1.15778691154034,-9.78349645671845));
#15393=CARTESIAN_POINT('Ctrl Pts',(3.78932058012659,-1.15140197073065,-9.78142599397901));
#15394=CARTESIAN_POINT('Ctrl Pts',(3.89799492378891,-1.12470200325839,-9.77433422040861));
#15395=CARTESIAN_POINT('Ctrl Pts',(3.97333713010549,-1.09784460183248,-9.76949720051125));
#15396=CARTESIAN_POINT('Ctrl Pts',(4.05640124512457,-1.05833670225327,-9.76374217171437));
#15397=CARTESIAN_POINT('Ctrl Pts',(4.06732943040864,-1.05292917485303,-9.76297641879315));
#15398=CARTESIAN_POINT('Ctrl Pts',(4.07816928770683,-1.0473542783481,-9.76220700099567));
#15399=CARTESIAN_POINT('',(2.36176926760077,-0.000715235775294672,-9.82563288520559));
#15400=CARTESIAN_POINT('Ctrl Pts',(4.07816926754759,-1.04735428871592,-9.66287031899079));
#15401=CARTESIAN_POINT('Ctrl Pts',(4.03640204496254,-1.06883500804511,-9.66603810987595));
#15402=CARTESIAN_POINT('Ctrl Pts',(3.9933141503434,-1.08783078014696,-9.66920590076111));
#15403=CARTESIAN_POINT('Ctrl Pts',(3.94923246509231,-1.10418747517802,-9.67237369164627));
#15404=CARTESIAN_POINT('Ctrl Pts',(3.90516395949031,-1.12053927984476,-9.67554053541764));
#15405=CARTESIAN_POINT('Ctrl Pts',(3.86010277492871,-1.13425337867765,-9.67870737918901));
#15406=CARTESIAN_POINT('Ctrl Pts',(3.81439467726135,-1.14522419301647,-9.68187422296037));
#15407=CARTESIAN_POINT('Ctrl Pts',(3.76864638056048,-1.15620465588926,-9.68504385188503));
#15408=CARTESIAN_POINT('Ctrl Pts',(3.72225057715234,-1.16443688268081,-9.68821348080969));
#15409=CARTESIAN_POINT('Ctrl Pts',(3.67556517756882,-1.16986602386283,-9.69138310973436));
#15410=CARTESIAN_POINT('Ctrl Pts',(3.62885909613471,-1.1752975701798,-9.69455414281947));
#15411=CARTESIAN_POINT('Ctrl Pts',(3.5818637204158,-1.17792352262935,-9.69772517590458));
#15412=CARTESIAN_POINT('Ctrl Pts',(3.53494037375074,-1.17774109982624,-9.7008962089897));
#15413=CARTESIAN_POINT('Ctrl Pts',(3.48792659891677,-1.17755832546765,-9.7040733531205));
#15414=CARTESIAN_POINT('Ctrl Pts',(3.44098568817978,-1.17455640149661,-9.70725049725131));
#15415=CARTESIAN_POINT('Ctrl Pts',(3.3944756066763,-1.16878460886773,-9.71042764138211));
#15416=CARTESIAN_POINT('Ctrl Pts',(3.36250330188285,-1.16481692041891,-9.71261169733814));
#15417=CARTESIAN_POINT('Ctrl Pts',(3.33073447233927,-1.15954140798911,-9.71479575329416));
#15418=CARTESIAN_POINT('Ctrl Pts',(3.29928186879577,-1.15298792667738,-9.71697980925019));
#15419=CARTESIAN_POINT('Ctrl Pts',(3.25187865494836,-1.14311096766395,-9.72027146907716));
#15420=CARTESIAN_POINT('Ctrl Pts',(3.20497661177928,-1.13028308409168,-9.72356312890415));
#15421=CARTESIAN_POINT('Ctrl Pts',(3.15896922680476,-1.11457475937872,-9.72685478873113));
#15422=CARTESIAN_POINT('Ctrl Pts',(3.11463212633289,-1.09943672074799,-9.73002694582176));
#15423=CARTESIAN_POINT('Ctrl Pts',(3.07112641688879,-1.08162400884126,-9.73319910291238));
#15424=CARTESIAN_POINT('Ctrl Pts',(3.02879375923831,-1.0612514967925,-9.73637126000301));
#15425=CARTESIAN_POINT('Ctrl Pts',(2.98650317201939,-1.04089923105998,-9.73954026458621));
#15426=CARTESIAN_POINT('Ctrl Pts',(2.9453838294259,-1.01799244096358,-9.7427092691694));
#15427=CARTESIAN_POINT('Ctrl Pts',(2.9057579425434,-0.99269427349977,-9.7458782737526));
#15428=CARTESIAN_POINT('Ctrl Pts',(2.86615398990713,-0.96741010941299,-9.74904552418637));
#15429=CARTESIAN_POINT('Ctrl Pts',(2.82804232459403,-0.939737489628927,
-9.75221277462014));
#15430=CARTESIAN_POINT('Ctrl Pts',(2.79171863284347,-0.909884387143714,
-9.75538002505391));
#15431=CARTESIAN_POINT('Ctrl Pts',(2.7553990562947,-0.880034666791066,-9.75854691666196));
#15432=CARTESIAN_POINT('Ctrl Pts',(2.72086748032072,-0.848005309651611,
-9.76171380827001));
#15433=CARTESIAN_POINT('Ctrl Pts',(2.6883866096355,-0.814044612253605,-9.76488069987807));
#15434=CARTESIAN_POINT('Ctrl Pts',(2.65587286301626,-0.780049541095812,
-9.76805079689649));
#15435=CARTESIAN_POINT('Ctrl Pts',(2.62541434795704,-0.744119633990367,
-9.7712208939149));
#15436=CARTESIAN_POINT('Ctrl Pts',(2.59723555364959,-0.706538657264058,
-9.77439099093332));
#15437=CARTESIAN_POINT('Ctrl Pts',(2.56903958472873,-0.668934775414841,
-9.77756302008518));
#15438=CARTESIAN_POINT('Ctrl Pts',(2.54312640863249,-0.629678286970802,
-9.78073504923704));
#15439=CARTESIAN_POINT('Ctrl Pts',(2.51967688301253,-0.58908150206193,-9.7839070783889));
#15440=CARTESIAN_POINT('Ctrl Pts',(2.49618521099785,-0.548411751578014,
-9.78708480870482));
#15441=CARTESIAN_POINT('Ctrl Pts',(2.47516626853492,-0.50639739884094,-9.79026253902073));
#15442=CARTESIAN_POINT('Ctrl Pts',(2.45675386851054,-0.46337309302342,-9.79344026933665));
#15443=CARTESIAN_POINT('Ctrl Pts',(2.45184931948999,-0.451912619827236,
-9.79428672792368));
#15444=CARTESIAN_POINT('Ctrl Pts',(2.44712944272375,-0.440380575424196,
-9.79513318651071));
#15445=CARTESIAN_POINT('Ctrl Pts',(2.4425961684122,-0.428783457494737,-9.79597964509774));
#15446=CARTESIAN_POINT('Ctrl Pts',(2.42336625378943,-0.379589084437358,
-9.79957027854317));
#15447=CARTESIAN_POINT('Ctrl Pts',(2.40742663073616,-0.329040465405448,
-9.80316091198859));
#15448=CARTESIAN_POINT('Ctrl Pts',(2.39494311029787,-0.277562569138398,
-9.80675154543401));
#15449=CARTESIAN_POINT('Ctrl Pts',(2.38255303096995,-0.226469993006811,
-9.81031530242437));
#15450=CARTESIAN_POINT('Ctrl Pts',(2.37356764353218,-0.174462259850974,
-9.81387905941473));
#15451=CARTESIAN_POINT('Ctrl Pts',(2.36810239749475,-0.121975767029384,
-9.81744281640509));
#15452=CARTESIAN_POINT('Ctrl Pts',(2.36391573519994,-0.0817683877132421,
-9.82017283933859));
#15453=CARTESIAN_POINT('Ctrl Pts',(2.36179390249004,-0.0412805101726955,
-9.82290286227209));
#15454=CARTESIAN_POINT('Ctrl Pts',(2.36176926760077,-0.000715235775294672,
-9.82563288520559));
#15455=CARTESIAN_POINT('Ctrl Pts',(4.07816926754606,-1.0473542887167,-10.1620324047393));
#15456=CARTESIAN_POINT('Ctrl Pts',(4.11166851029021,-1.03012575910453,-10.1593451640671));
#15457=CARTESIAN_POINT('Ctrl Pts',(4.14432478142673,-1.01129850207866,-10.1567044894124));
#15458=CARTESIAN_POINT('Ctrl Pts',(4.18465099112637,-0.985395825742646,
-10.1534149717822));
#15459=CARTESIAN_POINT('Ctrl Pts',(4.19320386985264,-0.979742988069625,
-10.152715498407));
#15460=CARTESIAN_POINT('Ctrl Pts',(4.20672468889827,-0.970550812183664,
-10.1516065546902));
#15461=CARTESIAN_POINT('Ctrl Pts',(4.21174066747047,-0.967083420925472,
-10.1511944434489));
#15462=CARTESIAN_POINT('Ctrl Pts',(4.22074020716762,-0.960758465173311,
-10.1504536576296));
#15463=CARTESIAN_POINT('Ctrl Pts',(4.22473325419787,-0.95791470861673,-10.1501244753992));
#15464=CARTESIAN_POINT('Ctrl Pts',(4.23410144147423,-0.951154348163961,
-10.1493509172429));
#15465=CARTESIAN_POINT('Ctrl Pts',(4.23946143132522,-0.947216954268419,
-10.1489073430298));
#15466=CARTESIAN_POINT('Ctrl Pts',(4.25509170414454,-0.935529991508297,
-10.1476106700208));
#15467=CARTESIAN_POINT('Ctrl Pts',(4.26526891203165,-0.927657128079991,
-10.1467623263627));
#15468=CARTESIAN_POINT('Ctrl Pts',(4.28812280417377,-0.909371496965137,
-10.1448462017761));
#15469=CARTESIAN_POINT('Ctrl Pts',(4.30071517653537,-0.89885738408202,-10.1437824169512));
#15470=CARTESIAN_POINT('Ctrl Pts',(4.34232059683862,-0.862616967717274,
-10.1402335078206));
#15471=CARTESIAN_POINT('Ctrl Pts',(4.37028296160212,-0.835721268162505,
-10.1377914920261));
#15472=CARTESIAN_POINT('Ctrl Pts',(4.44007817696513,-0.76161669609319,-10.1314454893765));
#15473=CARTESIAN_POINT('Ctrl Pts',(4.47953353278298,-0.712347593258341,
-10.1275960174921));
#15474=CARTESIAN_POINT('Ctrl Pts',(4.52146125685367,-0.650402488720235,
-10.1229045197741));
#15475=CARTESIAN_POINT('Ctrl Pts',(4.52791881486826,-0.640546475416325,
-10.1221619969));
#15476=CARTESIAN_POINT('Ctrl Pts',(4.55094777908877,-0.604220334616202,
-10.1194334243294));
#15477=CARTESIAN_POINT('Ctrl Pts',(4.5666110517894,-0.577193141720599,-10.1174189246061));
#15478=CARTESIAN_POINT('Ctrl Pts',(4.58419542312343,-0.543864030123283,
-10.1149139420247));
#15479=CARTESIAN_POINT('Ctrl Pts',(4.58716318576775,-0.538125048624946,
-10.1144818805222));
#15480=CARTESIAN_POINT('Ctrl Pts',(4.59170819704717,-0.529155914180496,
-10.113805056611));
#15481=CARTESIAN_POINT('Ctrl Pts',(4.59331818438885,-0.525942360125429,
-10.1135622444156));
#15482=CARTESIAN_POINT('Ctrl Pts',(4.59626448541928,-0.519993668047369,
-10.1131120993147));
#15483=CARTESIAN_POINT('Ctrl Pts',(4.59760493039593,-0.517260668413725,
-10.1129050227833));
#15484=CARTESIAN_POINT('Ctrl Pts',(4.60063984928993,-0.511011688587452,
-10.1124309444956));
#15485=CARTESIAN_POINT('Ctrl Pts',(4.60232744217774,-0.50749247972229,-10.1121635374083));
#15486=CARTESIAN_POINT('Ctrl Pts',(4.607494848954,-0.496577846909258,-10.1113330310723));
#15487=CARTESIAN_POINT('Ctrl Pts',(4.61091510449656,-0.489154730425527,
-10.1107665613824));
#15488=CARTESIAN_POINT('Ctrl Pts',(4.61874976709229,-0.471674412298479,
-10.1094297944437));
#15489=CARTESIAN_POINT('Ctrl Pts',(4.62310123497383,-0.46158999227168,-10.108656453785));
#15490=CARTESIAN_POINT('Ctrl Pts',(4.6381243482863,-0.425390762409366,-10.1058763677648));
#15491=CARTESIAN_POINT('Ctrl Pts',(4.64799747922974,-0.398956466529585,
-10.1038389034186));
#15492=CARTESIAN_POINT('Ctrl Pts',(4.68385429048858,-0.291308292914443,
-10.0955740863451));
#15493=CARTESIAN_POINT('Ctrl Pts',(4.70193773390399,-0.207723903788031,
-10.0892529308968));
#15494=CARTESIAN_POINT('Ctrl Pts',(4.71484627096173,-0.0847143797604495,
-10.0804227366325));
#15495=CARTESIAN_POINT('Ctrl Pts',(4.71698423271749,-0.046334865646207,
-10.077728572741));
#15496=CARTESIAN_POINT('Ctrl Pts',(4.71731162056922,0.00237606310295109,
-10.0743850355434));
#15497=CARTESIAN_POINT('Ctrl Pts',(4.71724588958997,0.0126683837430763,
-10.0736827767839));
#15498=CARTESIAN_POINT('Ctrl Pts',(4.71692632293037,0.0290585234999041,
-10.0725708597118));
#15499=CARTESIAN_POINT('Ctrl Pts',(4.71675999798506,0.035157317066796,-10.0721585254195));
#15500=CARTESIAN_POINT('Ctrl Pts',(4.71637489167241,0.0461447013263969,
-10.0714181288078));
#15501=CARTESIAN_POINT('Ctrl Pts',(4.71617302108258,0.0510337056252975,
-10.0710895529949));
#15502=CARTESIAN_POINT('Ctrl Pts',(4.71562621948057,0.0625368070761503,
-10.0703184501178));
#15503=CARTESIAN_POINT('Ctrl Pts',(4.71525595287784,0.0691495811071611,
-10.0698767148851));
#15504=CARTESIAN_POINT('Ctrl Pts',(4.71400925872773,0.0884905607197706,
-10.0685890079186));
#15505=CARTESIAN_POINT('Ctrl Pts',(4.71298175637836,0.101208335222971,-10.0677477037715));
#15506=CARTESIAN_POINT('Ctrl Pts',(4.71017765634749,0.130065538128462,-10.0658494040565));
#15507=CARTESIAN_POINT('Ctrl Pts',(4.70827355971496,0.146190120920674,-10.0647963057246));
#15508=CARTESIAN_POINT('Ctrl Pts',(4.70077428492776,0.200100227503268,-10.0612945272852));
#15509=CARTESIAN_POINT('Ctrl Pts',(4.69367465118615,0.237653143985456,-10.0588876915591));
#15510=CARTESIAN_POINT('Ctrl Pts',(4.67415255596877,0.319013340144446,-10.0536696874119));
#15511=CARTESIAN_POINT('Ctrl Pts',(4.66099126336457,0.362578016086178,-10.0508736958156));
#15512=CARTESIAN_POINT('Ctrl Pts',(4.63926941170991,0.421848134245943,-10.0469577753029));
#15513=CARTESIAN_POINT('Ctrl Pts',(4.63282295101693,0.438284452225309,-10.0458592209155));
#15514=CARTESIAN_POINT('Ctrl Pts',(4.61758362514522,0.474708786187078,-10.0433843037041));
#15515=CARTESIAN_POINT('Ctrl Pts',(4.60859965759033,0.494609162824384,-10.0420042452341));
#15516=CARTESIAN_POINT('Ctrl Pts',(4.58909230452171,0.534801884064379,-10.0391372178779));
#15517=CARTESIAN_POINT('Ctrl Pts',(4.57852104891252,0.555060134746424,-10.0376488897872));
#15518=CARTESIAN_POINT('Ctrl Pts',(4.56445605752608,0.580202357629179,-10.0357302556828));
#15519=CARTESIAN_POINT('Ctrl Pts',(4.56150439207674,0.585385857413958,-10.0353307671316));
#15520=CARTESIAN_POINT('Ctrl Pts',(4.55678584467183,0.593527762009445,-10.0346966880801));
#15521=CARTESIAN_POINT('Ctrl Pts',(4.55504508620572,0.596501303299116,-10.0344637135381));
#15522=CARTESIAN_POINT('Ctrl Pts',(4.55172798568358,0.602110926384337,-10.0340214661289));
#15523=CARTESIAN_POINT('Ctrl Pts',(4.55015435338888,0.604748526081976,-10.033812363926));
#15524=CARTESIAN_POINT('Ctrl Pts',(4.54643392897759,0.610929335547352,-10.0333196657103));
#15525=CARTESIAN_POINT('Ctrl Pts',(4.54427873953443,0.614467404762811,-10.0330355402782));
#15526=CARTESIAN_POINT('Ctrl Pts',(4.53714005011039,0.626048665975641,-10.0320988013784));
#15527=CARTESIAN_POINT('Ctrl Pts',(4.53207843790301,0.634042931796248,-10.031441511686));
#15528=CARTESIAN_POINT('Ctrl Pts',(4.50327938562384,0.678337876130907,-10.0277431665269));
#15529=CARTESIAN_POINT('Ctrl Pts',(4.4776491818813,0.713363398421631,-10.0246059439746));
#15530=CARTESIAN_POINT('Ctrl Pts',(4.43054094908304,0.770798977324831,-10.0191785866802));
#15531=CARTESIAN_POINT('Ctrl Pts',(4.40999900225179,0.793924249159746,-10.0169054365728));
#15532=CARTESIAN_POINT('Ctrl Pts',(4.3344886010232,0.872472576280763,-10.0089163017177));
#15533=CARTESIAN_POINT('Ctrl Pts',(4.27493989952936,0.923225416383328,-10.0032684650201));
#15534=CARTESIAN_POINT('Ctrl Pts',(4.19806104426981,0.976554032701125,-9.99678410147741));
#15535=CARTESIAN_POINT('Ctrl Pts',(4.1851508866706,0.985136999673151,-9.99571908618209));
#15536=CARTESIAN_POINT('Ctrl Pts',(4.16610062426853,0.997266638836645,-9.99418116447606));
#15537=CARTESIAN_POINT('Ctrl Pts',(4.1600924516165,1.00101642101442,-9.99370087620955));
#15538=CARTESIAN_POINT('Ctrl Pts',(4.14937351447643,1.00757265518793,-9.99285226109225));
#15539=CARTESIAN_POINT('Ctrl Pts',(4.14467633717077,1.01040080307155,-9.99248315717797));
#15540=CARTESIAN_POINT('Ctrl Pts',(4.13483901364542,1.01623059964736,-9.99171580851009));
#15541=CARTESIAN_POINT('Ctrl Pts',(4.12969550654026,1.01922629632226,-9.99131778472036));
#15542=CARTESIAN_POINT('Ctrl Pts',(4.1162118682032,1.02694318165454,-9.99028250046438));
#15543=CARTESIAN_POINT('Ctrl Pts',(4.10783632060286,1.03160185815931,-9.98964746137561));
#15544=CARTESIAN_POINT('Ctrl Pts',(4.06924341848271,1.05245544578049,-9.98675652842602));
#15545=CARTESIAN_POINT('Ctrl Pts',(4.03838308966577,1.06742933588016,-9.98454324538067));
#15546=CARTESIAN_POINT('Ctrl Pts',(3.94565303397733,1.10752166517873,-9.97812004127294));
#15547=CARTESIAN_POINT('Ctrl Pts',(3.88225426486694,1.12875250755144,-9.97402125003092));
#15548=CARTESIAN_POINT('Ctrl Pts',(3.75907413967879,1.15865981026454,-9.96616716643602));
#15549=CARTESIAN_POINT('Ctrl Pts',(3.69976260098377,1.16833948092059,-9.96242746122153));
#15550=CARTESIAN_POINT('Ctrl Pts',(3.62998104457627,1.17431359318376,-9.95781965141308));
#15551=CARTESIAN_POINT('Ctrl Pts',(3.61997130881696,1.1750417887249,-9.95715367202727));
#15552=CARTESIAN_POINT('Ctrl Pts',(3.60601834603003,1.17587773615314,-9.95621683256612));
#15553=CARTESIAN_POINT('Ctrl Pts',(3.60208170084995,1.17609375491992,-9.95595157385425));
#15554=CARTESIAN_POINT('Ctrl Pts',(3.59528856777066,1.17643231757813,-9.95549210065292));
#15555=CARTESIAN_POINT('Ctrl Pts',(3.59243254997252,1.17656423455301,-9.95529839567623));
#15556=CARTESIAN_POINT('Ctrl Pts',(3.58640729039202,1.17682055348271,-9.95488857072086));
#15557=CARTESIAN_POINT('Ctrl Pts',(3.58323799477549,1.17694255393065,-9.9546723159746));
#15558=CARTESIAN_POINT('Ctrl Pts',(3.57537144282337,1.17721355546381,-9.95413390646998));
#15559=CARTESIAN_POINT('Ctrl Pts',(3.57067375232767,1.17734724354175,-9.95381093208487));
#15560=CARTESIAN_POINT('Ctrl Pts',(3.55294431672716,1.17774561000984,-9.95258683915924));
#15561=CARTESIAN_POINT('Ctrl Pts',(3.53990984509297,1.17782204586383,-9.95167638161156));
#15562=CARTESIAN_POINT('Ctrl Pts',(3.50641952201881,1.17746255152787,-9.94931443980075));
#15563=CARTESIAN_POINT('Ctrl Pts',(3.4859719253822,1.1767099240049,-9.94785067109951));
#15564=CARTESIAN_POINT('Ctrl Pts',(3.4078203949716,1.17179225013658,-9.94219641426312));
#15565=CARTESIAN_POINT('Ctrl Pts',(3.35043286064573,1.16391055197607,-9.93792400994631));
#15566=CARTESIAN_POINT('Ctrl Pts',(3.22007496124566,1.13610831767881,-9.9281736756038));
#15567=CARTESIAN_POINT('Ctrl Pts',(3.14796290757953,1.11331680287793,-9.92275451057965));
#15568=CARTESIAN_POINT('Ctrl Pts',(3.06895501780716,1.07970945794833,-9.91684620350546));
#15569=CARTESIAN_POINT('Ctrl Pts',(3.0594476826702,1.07551593025369,-9.91613540986386));
#15570=CARTESIAN_POINT('Ctrl Pts',(3.0438803115349,1.06840185678349,-9.91497154925038));
#15571=CARTESIAN_POINT('Ctrl Pts',(3.03778775070248,1.06555431264159,-9.91451604999203));
#15572=CARTESIAN_POINT('Ctrl Pts',(3.02682293648184,1.06031467603284,-9.91369616307984));
#15573=CARTESIAN_POINT('Ctrl Pts',(3.02194223424367,1.05794081049147,-9.91333116714618));
#15574=CARTESIAN_POINT('Ctrl Pts',(3.01698178095538,1.05548561148612,-9.91296011997739));
#15575=CARTESIAN_POINT('Ctrl Pts',(3.01688552362932,1.05543795208819,-9.9129529197935));
#15576=CARTESIAN_POINT('Ctrl Pts',(3.01671703606709,1.05535450100128,-9.91294031662625));
#15577=CARTESIAN_POINT('Ctrl Pts',(3.01664480299475,1.05531871506887,-9.91293491344563));
#15578=CARTESIAN_POINT('Ctrl Pts',(3.01646257406813,1.05522841134728,-9.91292128230272));
#15579=CARTESIAN_POINT('Ctrl Pts',(3.01635258304072,1.05517388376421,-9.91291305467593));
#15580=CARTESIAN_POINT('Ctrl Pts',(3.01613910253037,1.0550680101256,-9.91289708566733));
#15581=CARTESIAN_POINT('Ctrl Pts',(3.01603561207763,1.05501666604117,-9.91288934421818));
#15582=CARTESIAN_POINT('Ctrl Pts',(3.01583473440515,1.05491696899766,-9.91287431778421));
#15583=CARTESIAN_POINT('Ctrl Pts',(3.01573734632957,1.05486861778104,-9.91286703274002));
#15584=CARTESIAN_POINT('Ctrl Pts',(3.01554829969533,1.05477472730295,-9.91285289117339));
#15585=CARTESIAN_POINT('Ctrl Pts',(3.01545664037686,1.05472918957985,-9.91284603459825));
#15586=CARTESIAN_POINT('Ctrl Pts',(3.00971714244538,1.05187678811162,-9.91241668943013));
#15587=CARTESIAN_POINT('Ctrl Pts',(3.00409184483775,1.04902457034529,-9.91199576439533));
#15588=CARTESIAN_POINT('Ctrl Pts',(2.98824145927402,1.04082716915612,-9.91080916586421));
#15589=CARTESIAN_POINT('Ctrl Pts',(2.97807143432156,1.03537663113004,-9.91004715541127));
#15590=CARTESIAN_POINT('Ctrl Pts',(2.95535603671599,1.02276936999385,-9.90834244044464));
#15591=CARTESIAN_POINT('Ctrl Pts',(2.94285879519073,1.01552950640833,-9.90740266706053));
#15592=CARTESIAN_POINT('Ctrl Pts',(2.90307992222631,0.991497047842256,-9.90440096582231));
#15593=CARTESIAN_POINT('Ctrl Pts',(2.87634825822561,0.973820256433688,-9.90236815363861));
#15594=CARTESIAN_POINT('Ctrl Pts',(2.80859602991565,0.924932492798933,-9.89712467840091));
#15595=CARTESIAN_POINT('Ctrl Pts',(2.76884532639873,0.892082264471316,-9.89395685010029));
#15596=CARTESIAN_POINT('Ctrl Pts',(2.68815696174492,0.815969955955608,-9.88708364091148));
#15597=CARTESIAN_POINT('Ctrl Pts',(2.64809324935974,0.771999095504211,-9.88337993285492));
#15598=CARTESIAN_POINT('Ctrl Pts',(2.60535368857308,0.7173078089846,-9.87881321617277));
#15599=CARTESIAN_POINT('Ctrl Pts',(2.59928650732665,0.709336425606377,-9.87814845109279));
#15600=CARTESIAN_POINT('Ctrl Pts',(2.59097720743559,0.698125304851623,-9.8772131594298));
#15601=CARTESIAN_POINT('Ctrl Pts',(2.58864834471278,0.694949975962603,-9.87694821776404));
#15602=CARTESIAN_POINT('Ctrl Pts',(2.5846577669473,0.689451340370706,-9.87648924413703));
#15603=CARTESIAN_POINT('Ctrl Pts',(2.58298848090638,0.687133531824313,-9.87629572061605));
#15604=CARTESIAN_POINT('Ctrl Pts',(2.57948395736393,0.682229973594607,-9.87588613299414));
#15605=CARTESIAN_POINT('Ctrl Pts',(2.57765071123529,0.67964285773079,-9.87566993348663));
#15606=CARTESIAN_POINT('Ctrl Pts',(2.57312642654383,0.673203122140363,-9.87513159090387));
#15607=CARTESIAN_POINT('Ctrl Pts',(2.57044798030795,0.669341770944382,-9.87480862778345));
#15608=CARTESIAN_POINT('Ctrl Pts',(2.56042509775549,0.654706133376354,-9.87358419142916));
#15609=CARTESIAN_POINT('Ctrl Pts',(2.55323697441191,0.643826623006103,-9.87267336829594));
#15610=CARTESIAN_POINT('Ctrl Pts',(2.53523147034626,0.615565274819328,-9.87031013372975));
#15611=CARTESIAN_POINT('Ctrl Pts',(2.52468426828429,0.598017070539264,-9.86884541681277));
#15612=CARTESIAN_POINT('Ctrl Pts',(2.46871959008831,0.499156599838894,-9.86064221196433));
#15613=CARTESIAN_POINT('Ctrl Pts',(2.43261202885941,0.412950812776566,-9.85370125799127));
#15614=CARTESIAN_POINT('Ctrl Pts',(2.39671037874418,0.287223833775087,-9.844334975543));
#15615=CARTESIAN_POINT('Ctrl Pts',(2.38812180487821,0.250587509652377,-9.84168526405144));
#15616=CARTESIAN_POINT('Ctrl Pts',(2.37916376817953,0.20201355784022,-9.83827640048387));
#15617=CARTESIAN_POINT('Ctrl Pts',(2.37720100497103,0.1903960011619,-9.83746871041783));
#15618=CARTESIAN_POINT('Ctrl Pts',(2.37434104438738,0.171770618151118,-9.83618557881491));
#15619=CARTESIAN_POINT('Ctrl Pts',(2.37333203921694,0.164781035508374,-9.83570668952124));
#15620=CARTESIAN_POINT('Ctrl Pts',(2.37165218572722,0.15235500247942,-9.83485986347754));
#15621=CARTESIAN_POINT('Ctrl Pts',(2.37095628930806,0.146922209039614,-9.83449115792062));
#15622=CARTESIAN_POINT('Ctrl Pts',(2.36968822413248,0.136442995899603,-9.83378284684814));
#15623=CARTESIAN_POINT('Ctrl Pts',(2.36911074985229,0.13139735382971,-9.83344308449042));
#15624=CARTESIAN_POINT('Ctrl Pts',(2.36793837113065,0.120532125987115,-9.83271412241372));
#15625=CARTESIAN_POINT('Ctrl Pts',(2.36735414986538,0.114711505266053,-9.83232525977258));
#15626=CARTESIAN_POINT('Ctrl Pts',(2.36604434526003,0.100604956054645,-9.83138667198957));
#15627=CARTESIAN_POINT('Ctrl Pts',(2.36536311530124,0.0923151481298986,
-9.83083830820046));
#15628=CARTESIAN_POINT('Ctrl Pts',(2.36275423588792,0.0558377771113773,
-9.82843851337979));
#15629=CARTESIAN_POINT('Ctrl Pts',(2.36175332805078,0.0275923818668629,
-9.82661507307611));
#15630=CARTESIAN_POINT('Ctrl Pts',(2.36176923710637,-0.000663123418161781,
-9.82481492042546));
#15631=CARTESIAN_POINT('Origin',(3.53951905042299,8.32667268468867E-16,
0.));
#15632=CARTESIAN_POINT('',(2.07451448579446,-0.00104776130442043,-0.160655045842906));
#15633=CARTESIAN_POINT('',(2.07598378213352,-0.00160958027810672,-0.0893449541570843));
#15634=CARTESIAN_POINT('',(2.07601905042299,1.01189432752408E-15,0.));
#15635=CARTESIAN_POINT('',(4.17447558192119,-1.32104331271118,-3.52050110134855E-5));
#15636=CARTESIAN_POINT('Ctrl Pts',(2.07451448579446,-0.00104776130442043,
-0.160655045842906));
#15637=CARTESIAN_POINT('Ctrl Pts',(2.07407030736436,-0.059925529006458,
-0.157443865218375));
#15638=CARTESIAN_POINT('Ctrl Pts',(2.10392157786283,-0.601150164264895,
-0.127899405977995));
#15639=CARTESIAN_POINT('Ctrl Pts',(2.74920669632528,-1.50947517628745,-0.0743594590340226));
#15640=CARTESIAN_POINT('Ctrl Pts',(3.77694222363607,-1.50905204600162,-0.0240306927145928));
#15641=CARTESIAN_POINT('Ctrl Pts',(4.17447558192119,-1.32104331271118,-3.52050110134856E-5));
#15642=CARTESIAN_POINT('',(2.90551195584778,-1.31904027763685,0.));
#15643=CARTESIAN_POINT('Origin',(3.53951905042299,8.32667268468867E-16,
0.));
#15644=CARTESIAN_POINT('Ctrl Pts',(2.90551195584777,-1.31904027763685,-4.5102810375397E-16));
#15645=CARTESIAN_POINT('Ctrl Pts',(2.46902340624,-1.10923861968598,-0.0263332786158544));
#15646=CARTESIAN_POINT('Ctrl Pts',(2.10648828248685,-0.609902210944796,
-0.0561149300015489));
#15647=CARTESIAN_POINT('Ctrl Pts',(2.0743190278226,-0.0648117932209503,
-0.0858965813872436));
#15648=CARTESIAN_POINT('Ctrl Pts',(2.07482541103651,-0.00161085424212562,
-0.0893449541570843));
#15649=CARTESIAN_POINT('Origin',(3.53951905042299,8.32667268468867E-16,
0.));
#15650=CARTESIAN_POINT('',(2.07827644886075,-0.000378700063536769,-0.660655045842906));
#15651=CARTESIAN_POINT('',(2.07601908529222,-0.000319471822349998,-0.589344954125452));
#15652=CARTESIAN_POINT('',(2.07601905042299,1.01189432752408E-15,0.));
#15653=CARTESIAN_POINT('Ctrl Pts',(2.07827644886075,-0.000378700063536769,
-0.660655045842906));
#15654=CARTESIAN_POINT('Ctrl Pts',(2.07776587840242,-0.219619213994846,
-0.648776870246833));
#15655=CARTESIAN_POINT('Ctrl Pts',(2.22661874708729,-0.924244535467465,
-0.610565416034906));
#15656=CARTESIAN_POINT('Ctrl Pts',(3.31520031757397,-1.7123247414839,-0.546020683207126));
#15657=CARTESIAN_POINT('Ctrl Pts',(4.85108637608084,-1.12351020784619,-0.467020847359564));
#15658=CARTESIAN_POINT('Ctrl Pts',(5.19709361453891,0.484647885353767,-0.388021011512002));
#15659=CARTESIAN_POINT('Ctrl Pts',(4.03936404899096,1.65296550581617,-0.309021175664439));
#15660=CARTESIAN_POINT('Ctrl Pts',(2.49361202232558,1.33546458710318,-0.233232520441406));
#15661=CARTESIAN_POINT('Ctrl Pts',(2.07771279146056,0.42290145659918,-0.183777143834229));
#15662=CARTESIAN_POINT('Ctrl Pts',(2.07451448579446,-0.00104776130442043,
-0.160655045842906));
#15663=CARTESIAN_POINT('Ctrl Pts',(2.07601993550036,-0.00160954051702442,
-0.0893449541570843));
#15664=CARTESIAN_POINT('Ctrl Pts',(2.07596079908734,0.0521611394986531,
-0.0922812167265794));
#15665=CARTESIAN_POINT('Ctrl Pts',(2.07886922409737,0.10606434640489,-0.0952174792960745));
#15666=CARTESIAN_POINT('Ctrl Pts',(2.08476241956241,0.159735390465519,-0.0981537418655696));
#15667=CARTESIAN_POINT('Ctrl Pts',(2.09064824768661,0.213339338011707,-0.101086333685085));
#15668=CARTESIAN_POINT('Ctrl Pts',(2.09951141065111,0.266711150229533,-0.1040189255046));
#15669=CARTESIAN_POINT('Ctrl Pts',(2.11131711806971,0.319486291446668,-0.106951517324116));
#15670=CARTESIAN_POINT('Ctrl Pts',(2.12311320475964,0.372218425049299,-0.109881719310547));
#15671=CARTESIAN_POINT('Ctrl Pts',(2.13784697264489,0.424354310406159,-0.112811921296979));
#15672=CARTESIAN_POINT('Ctrl Pts',(2.15543217948843,0.475537363102618,-0.115742123283411));
#15673=CARTESIAN_POINT('Ctrl Pts',(2.17301070165289,0.526700959543301,-0.11867121140976));
#15674=CARTESIAN_POINT('Ctrl Pts',(2.19343833596986,0.576911916944637,-0.121600299536108));
#15675=CARTESIAN_POINT('Ctrl Pts',(2.21657913201178,0.625829227724427,-0.124529387662457));
#15676=CARTESIAN_POINT('Ctrl Pts',(2.23973792130799,0.674784574430474,-0.127460753317521));
#15677=CARTESIAN_POINT('Ctrl Pts',(2.26561385320264,0.722443760890151,-0.130392118972585));
#15678=CARTESIAN_POINT('Ctrl Pts',(2.29402375449186,0.768487942529639,-0.133323484627649));
#15679=CARTESIAN_POINT('Ctrl Pts',(2.32244395550627,0.814548817026053,-0.136255913019974));
#15680=CARTESIAN_POINT('Ctrl Pts',(2.35339963776276,0.858993065166078,-0.1391883414123));
#15681=CARTESIAN_POINT('Ctrl Pts',(2.38666476771661,0.901531615000586,-0.142120769804625));
#15682=CARTESIAN_POINT('Ctrl Pts',(2.41999288509549,0.944150711453193,-0.145058750741424));
#15683=CARTESIAN_POINT('Ctrl Pts',(2.45563881424911,0.984856488107153,-0.147996731678223));
#15684=CARTESIAN_POINT('Ctrl Pts',(2.4933377924311,1.02339485313661,-0.150934712615022));
#15685=CARTESIAN_POINT('Ctrl Pts',(2.52355602097499,1.05428590584754,-0.153289698975056));
#15686=CARTESIAN_POINT('Ctrl Pts',(2.55509253490114,1.08378502701655,-0.15564468533509));
#15687=CARTESIAN_POINT('Ctrl Pts',(2.58779640634575,1.11178067025409,-0.157999671695124));
#15688=CARTESIAN_POINT('Ctrl Pts',(2.62966525203463,1.14762184791584,-0.161014622407449));
#15689=CARTESIAN_POINT('Ctrl Pts',(2.67364777126532,1.18116844514286,-0.164029573119773));
#15690=CARTESIAN_POINT('Ctrl Pts',(2.71946292469062,1.21216343809274,-0.167044523832097));
#15691=CARTESIAN_POINT('Ctrl Pts',(2.76519681446833,1.24310345433741,-0.17005412684014));
#15692=CARTESIAN_POINT('Ctrl Pts',(2.81275645448268,1.27150055651047,-0.173063729848182));
#15693=CARTESIAN_POINT('Ctrl Pts',(2.86182791208697,1.29713799228179,-0.176073332856224));
#15694=CARTESIAN_POINT('Ctrl Pts',(2.91085085370823,1.32275008082562,-0.179079960329085));
#15695=CARTESIAN_POINT('Ctrl Pts',(2.96138218748599,1.34560766618287,-0.182086587801947));
#15696=CARTESIAN_POINT('Ctrl Pts',(3.01308075284201,1.3655383439655,-0.185093215274809));
#15697=CARTESIAN_POINT('Ctrl Pts',(3.06474843345596,1.38545711515385,-0.188098046587305));
#15698=CARTESIAN_POINT('Ctrl Pts',(3.11758147341645,1.40245225608464,-0.191102877899802));
#15699=CARTESIAN_POINT('Ctrl Pts',(3.17121805515847,1.41639917639314,-0.194107709212299));
#15700=CARTESIAN_POINT('Ctrl Pts',(3.22484357973953,1.43034322154931,-0.197111921079961));
#15701=CARTESIAN_POINT('Ctrl Pts',(3.27927180820599,1.44124016178639,-0.200116132947624));
#15702=CARTESIAN_POINT('Ctrl Pts',(3.33412727462733,1.44901568950633,-0.203120344815286));
#15703=CARTESIAN_POINT('Ctrl Pts',(3.38903176753004,1.45679816652029,-0.206127241664897));
#15704=CARTESIAN_POINT('Ctrl Pts',(3.4443637392852,1.46145358319522,-0.209134138514508));
#15705=CARTESIAN_POINT('Ctrl Pts',(3.49974055646164,1.46295930272109,-0.212141035364119));
#15706=CARTESIAN_POINT('Ctrl Pts',(3.55514192643853,1.46446568984818,-0.215149265402275));
#15707=CARTESIAN_POINT('Ctrl Pts',(3.61058765464483,1.46281961068625,-0.218157495440431));
#15708=CARTESIAN_POINT('Ctrl Pts',(3.66569633293303,1.45805059698845,-0.221165725478586));
#15709=CARTESIAN_POINT('Ctrl Pts',(3.72090676766773,1.45327277745639,-0.224179510119183));
#15710=CARTESIAN_POINT('Ctrl Pts',(3.77577838710661,1.44536057860399,-0.22719329475978));
#15711=CARTESIAN_POINT('Ctrl Pts',(3.82993728420081,1.43439516852553,-0.230207079400376));
#15712=CARTESIAN_POINT('Ctrl Pts',(3.87062482059872,1.4261572695722,-0.23247122211448));
#15713=CARTESIAN_POINT('Ctrl Pts',(3.91091025465529,1.41619723790657,-0.234735364828584));
#15714=CARTESIAN_POINT('Ctrl Pts',(3.95064122796382,1.40456783571819,-0.236999507542687));
#15715=CARTESIAN_POINT('Ctrl Pts',(4.00355245674629,1.38908052421907,-0.2400147513982));
#15716=CARTESIAN_POINT('Ctrl Pts',(4.05569412745601,1.37056799884676,-0.243029995253713));
#15717=CARTESIAN_POINT('Ctrl Pts',(4.10669745483237,1.34912597913302,-0.246045239109226));
#15718=CARTESIAN_POINT('Ctrl Pts',(4.15761312718257,1.32772080997189,-0.24905530092481));
#15719=CARTESIAN_POINT('Ctrl Pts',(4.20739385781659,1.30339634107968,-0.252065362740393));
#15720=CARTESIAN_POINT('Ctrl Pts',(4.25568671822785,1.27629781853255,-0.255075424555976));
#15721=CARTESIAN_POINT('Ctrl Pts',(4.30393346467842,1.24922517186423,-0.258082612119112));
#15722=CARTESIAN_POINT('Ctrl Pts',(4.35069469917369,1.21938397594076,-0.261089799682248));
#15723=CARTESIAN_POINT('Ctrl Pts',(4.39563987438938,1.18696646320404,-0.264096987245384));
#15724=CARTESIAN_POINT('Ctrl Pts',(4.44055970480858,1.1545672308558,-0.267102479041255));
#15725=CARTESIAN_POINT('Ctrl Pts',(4.48366508027645,1.11959486885137,-0.270107970837126));
#15726=CARTESIAN_POINT('Ctrl Pts',(4.52465431683852,1.08228497026633,-0.273113462632997));
#15727=CARTESIAN_POINT('Ctrl Pts',(4.5656364640684,1.04498152465011,-0.27611843461119));
#15728=CARTESIAN_POINT('Ctrl Pts',(4.60450281077932,1.00534169956904,-0.279123406589384));
#15729=CARTESIAN_POINT('Ctrl Pts',(4.64098642029402,0.963639913613693,-0.282128378567578));
#15730=CARTESIAN_POINT('Ctrl Pts',(4.67750444356329,0.921898791774464,-0.285136185034178));
#15731=CARTESIAN_POINT('Ctrl Pts',(4.71163489275568,0.878092220415177,-0.288143991500778));
#15732=CARTESIAN_POINT('Ctrl Pts',(4.74315025731674,0.832528778956924,-0.291151797967377));
#15733=CARTESIAN_POINT('Ctrl Pts',(4.77468047668128,0.786943861117909,-0.294161022167029));
#15734=CARTESIAN_POINT('Ctrl Pts',(4.80359287980309,0.739600872161782,-0.297170246366681));
#15735=CARTESIAN_POINT('Ctrl Pts',(4.82970438381255,0.690835765943307,-0.300179470566333));
#15736=CARTESIAN_POINT('Ctrl Pts',(4.85586519016987,0.641978584054687,-0.303194376622466));
#15737=CARTESIAN_POINT('Ctrl Pts',(4.87921431079296,0.59169439909078,-0.306209282678599));
#15738=CARTESIAN_POINT('Ctrl Pts',(4.89961605177496,0.54034100058517,-0.309224188734732));
#15739=CARTESIAN_POINT('Ctrl Pts',(4.91489844618696,0.501873553564261,-0.311482573619904));
#15740=CARTESIAN_POINT('Ctrl Pts',(4.92852803145527,0.462806618524378,-0.313740958505077));
#15741=CARTESIAN_POINT('Ctrl Pts',(4.94046634319924,0.423295325822175,-0.315999343390249));
#15742=CARTESIAN_POINT('Ctrl Pts',(4.95635677614093,0.370704008005316,-0.319005355826847));
#15743=CARTESIAN_POINT('Ctrl Pts',(4.96931596167814,0.317103188847384,-0.322011368263446));
#15744=CARTESIAN_POINT('Ctrl Pts',(4.97922093326692,0.26285117183618,-0.325017380700044));
#15745=CARTESIAN_POINT('Ctrl Pts',(4.98910798703044,0.208697295253879,-0.328017955341587));
#15746=CARTESIAN_POINT('Ctrl Pts',(4.99595169590336,0.153895075152804,-0.331018529983131));
#15747=CARTESIAN_POINT('Ctrl Pts',(4.99967913163957,0.0988169379286829,
-0.334019104624674));
#15748=CARTESIAN_POINT('Ctrl Pts',(5.00340281149231,0.0437942991970763,
-0.337016655791248));
#15749=CARTESIAN_POINT('Ctrl Pts',(5.00401640212075,-0.011503180103168,
-0.340014206957822));
#15750=CARTESIAN_POINT('Ctrl Pts',(5.00149850268767,-0.0666958106319766,
-0.343011758124395));
#15751=CARTESIAN_POINT('Ctrl Pts',(4.99898213816164,-0.121854795830687,
-0.346007481989072));
#15752=CARTESIAN_POINT('Ctrl Pts',(4.99333809084124,-0.176908530788052,
-0.349003205853748));
#15753=CARTESIAN_POINT('Ctrl Pts',(4.98459704397959,-0.231477520589845,
-0.351998929718424));
#15754=CARTESIAN_POINT('Ctrl Pts',(4.97585784659602,-0.286034964389003,
-0.354994019731608));
#15755=CARTESIAN_POINT('Ctrl Pts',(4.96402303449634,-0.340107343854895,
-0.357989109744792));
#15756=CARTESIAN_POINT('Ctrl Pts',(4.9491748277167,-0.39332281848687,-0.360984199757975));
#15757=CARTESIAN_POINT('Ctrl Pts',(4.93431305450028,-0.446586914772849,
-0.363982026310321));
#15758=CARTESIAN_POINT('Ctrl Pts',(4.91643252835284,-0.498992030536336,
-0.366979852862666));
#15759=CARTESIAN_POINT('Ctrl Pts',(4.89566567284574,-0.550180505371983,
-0.369977679415011));
#15760=CARTESIAN_POINT('Ctrl Pts',(4.87488947926561,-0.601391997737453,
-0.372976853977085));
#15761=CARTESIAN_POINT('Ctrl Pts',(4.851224596326,-0.651385278977384,-0.375976028539159));
#15762=CARTESIAN_POINT('Ctrl Pts',(4.82485070969782,-0.699824817840734,
-0.378975203101233));
#15763=CARTESIAN_POINT('Ctrl Pts',(4.79842676241049,-0.74835630049978,-0.381980070440316));
#15764=CARTESIAN_POINT('Ctrl Pts',(4.76928381965483,-0.795327698123873,
-0.384984937779399));
#15765=CARTESIAN_POINT('Ctrl Pts',(4.73764580991827,-0.840431150173138,
-0.387989805118483));
#15766=CARTESIAN_POINT('Ctrl Pts',(4.71304542864684,-0.875501691155599,
-0.390326263158259));
#15767=CARTESIAN_POINT('Ctrl Pts',(4.68693746454828,-0.909443422819982,
-0.392662721198036));
#15768=CARTESIAN_POINT('Ctrl Pts',(4.65944323801357,-0.942126352486538,
-0.394999179237812));
#15769=CARTESIAN_POINT('Ctrl Pts',(4.62401033794178,-0.984246140052329,
-0.398010265370414));
#15770=CARTESIAN_POINT('Ctrl Pts',(4.58612386983908,-1.02445232578511,-0.401021351503017));
#15771=CARTESIAN_POINT('Ctrl Pts',(4.54601836869901,-1.06244593853518,-0.404032437635619));
#15772=CARTESIAN_POINT('Ctrl Pts',(4.50598404157429,-1.10037212517412,-0.407038180085072));
#15773=CARTESIAN_POINT('Ctrl Pts',(4.46373887671099,-1.13609317132882,-0.410043922534525));
#15774=CARTESIAN_POINT('Ctrl Pts',(4.41955646896318,-1.16934442828839,-0.413049664983978));
#15775=CARTESIAN_POINT('Ctrl Pts',(4.37541771414053,-1.20256283247454,-0.416052437711841));
#15776=CARTESIAN_POINT('Ctrl Pts',(4.32934592773248,-1.2333159657241,-0.419055210439705));
#15777=CARTESIAN_POINT('Ctrl Pts',(4.28164882806824,-1.26137846942629,-0.422057983167568));
#15778=CARTESIAN_POINT('Ctrl Pts',(4.23398004890087,-1.28942431081455,-0.425058972977471));
#15779=CARTESIAN_POINT('Ctrl Pts',(4.18468832324541,-1.31478242218084,-0.428059962787374));
#15780=CARTESIAN_POINT('Ctrl Pts',(4.13410956048888,-1.33727124224653,-0.431060952597277));
#15781=CARTESIAN_POINT('Ctrl Pts',(4.08354088934381,-1.35975557528206,-0.434061343641582));
#15782=CARTESIAN_POINT('Ctrl Pts',(4.03168617302838,-1.37937153969727,-0.437061734685886));
#15783=CARTESIAN_POINT('Ctrl Pts',(3.97890298125976,-1.39598496099436,-0.44006212573019));
#15784=CARTESIAN_POINT('Ctrl Pts',(3.92607143124894,-1.41261360296728,-0.443065265635106));
#15785=CARTESIAN_POINT('Ctrl Pts',(3.87231021076956,-1.42623404721551,-0.446068405540022));
#15786=CARTESIAN_POINT('Ctrl Pts',(3.81799237375506,-1.43676193511395,-0.449071545444937));
#15787=CARTESIAN_POINT('Ctrl Pts',(3.76364988103339,-1.44729460178371,-0.452076048521551));
#15788=CARTESIAN_POINT('Ctrl Pts',(3.70875079196186,-1.45473184269594,-0.455080551598165));
#15789=CARTESIAN_POINT('Ctrl Pts',(3.65367540862629,-1.45904097813658,-0.458085054674778));
#15790=CARTESIAN_POINT('Ctrl Pts',(3.59849643401324,-1.46335821862921,-0.461095208920627));
#15791=CARTESIAN_POINT('Ctrl Pts',(3.54314103162798,-1.46453558876919,-0.464105363166476));
#15792=CARTESIAN_POINT('Ctrl Pts',(3.48799047191199,-1.46259258017967,-0.467115517412325));
#15793=CARTESIAN_POINT('Ctrl Pts',(3.44595179011842,-1.46111151597584,-0.469410016636675));
#15794=CARTESIAN_POINT('Ctrl Pts',(3.4040321614047,-1.4578185062013,-0.471704515861025));
#15795=CARTESIAN_POINT('Ctrl Pts',(3.36239712990682,-1.45274226044149,-0.473999015085375));
#15796=CARTESIAN_POINT('Ctrl Pts',(3.30776586996789,-1.4460814824466,-0.477009734161245));
#15797=CARTESIAN_POINT('Ctrl Pts',(3.25339662216762,-1.43632083089672,-0.480020453237115));
#15798=CARTESIAN_POINT('Ctrl Pts',(3.19966786019915,-1.42349338547934,-0.483031172312986));
#15799=CARTESIAN_POINT('Ctrl Pts',(3.14603419204231,-1.41068864318471,-0.486036562757743));
#15800=CARTESIAN_POINT('Ctrl Pts',(3.09303926940122,-1.39482800039746,-0.489041953202501));
#15801=CARTESIAN_POINT('Ctrl Pts',(3.04105416113814,-1.37599600440926,-0.492047343647258));
#15802=CARTESIAN_POINT('Ctrl Pts',(2.98912025649314,-1.35718255731635,-0.495049773881494));
#15803=CARTESIAN_POINT('Ctrl Pts',(2.93819468975831,-1.33540373367036,-0.498052204115729));
#15804=CARTESIAN_POINT('Ctrl Pts',(2.88863426307353,-1.31079412708367,-0.501054634349964));
#15805=CARTESIAN_POINT('Ctrl Pts',(2.8391030990692,-1.28619905110339,-0.504055291815835));
#15806=CARTESIAN_POINT('Ctrl Pts',(2.79093594931848,-1.25877673941732,-0.507055949281707));
#15807=CARTESIAN_POINT('Ctrl Pts',(2.74446833136837,-1.22870932450711,-0.510056606747578));
#15808=CARTESIAN_POINT('Ctrl Pts',(2.6980098185465,-1.19864780117648,-0.513056676247631));
#15809=CARTESIAN_POINT('Ctrl Pts',(2.65325061907654,-1.16594249059498,-0.516056745747683));
#15810=CARTESIAN_POINT('Ctrl Pts',(2.61049839019024,-1.13081955362503,-0.519056815247735));
#15811=CARTESIAN_POINT('Ctrl Pts',(2.56770671146066,-1.09566420678089,-0.522059653077644));
#15812=CARTESIAN_POINT('Ctrl Pts',(2.52692611194843,-1.05808711242691,-0.525062490907552));
#15813=CARTESIAN_POINT('Ctrl Pts',(2.48843098092148,-1.01835461414557,-0.528065328737461));
#15814=CARTESIAN_POINT('Ctrl Pts',(2.44991824179449,-0.978603941778695,
-0.531069540098709));
#15815=CARTESIAN_POINT('Ctrl Pts',(2.41369340085686,-0.936696300222253,
-0.534073751459957));
#15816=CARTESIAN_POINT('Ctrl Pts',(2.37999151608081,-0.892932330640086,
-0.537077962821206));
#15817=CARTESIAN_POINT('Ctrl Pts',(2.34622600212414,-0.849085734654586,
-0.540087846135478));
#15818=CARTESIAN_POINT('Ctrl Pts',(2.31499325836578,-0.803376246283152,
-0.543097729449751));
#15819=CARTESIAN_POINT('Ctrl Pts',(2.28648517007055,-0.756133814009735,
-0.546107612764024));
#15820=CARTESIAN_POINT('Ctrl Pts',(2.26472839905209,-0.720079387256038,
-0.548404692153662));
#15821=CARTESIAN_POINT('Ctrl Pts',(2.24455769051474,-0.68313273160179,-0.550701771543299));
#15822=CARTESIAN_POINT('Ctrl Pts',(2.22603962976519,-0.645448728799149,
-0.552998850932937));
#15823=CARTESIAN_POINT('Ctrl Pts',(2.20008110709051,-0.592623486758152,
-0.556218885051406));
#15824=CARTESIAN_POINT('Ctrl Pts',(2.17727459283289,-0.538151764158661,
-0.559438919169876));
#15825=CARTESIAN_POINT('Ctrl Pts',(2.15781501561044,-0.482417050053909,
-0.562658953288345));
#15826=CARTESIAN_POINT('Ctrl Pts',(2.13840278776736,-0.426817950618098,
-0.565871152364185));
#15827=CARTESIAN_POINT('Ctrl Pts',(2.12232144068049,-0.369962354887564,
-0.569083351440025));
#15828=CARTESIAN_POINT('Ctrl Pts',(2.10971870822468,-0.312255074337636,
-0.572295550515864));
#15829=CARTESIAN_POINT('Ctrl Pts',(2.09716077482401,-0.254752926416818,
-0.575496331156537));
#15830=CARTESIAN_POINT('Ctrl Pts',(2.0880569275909,-0.196405520176387,-0.578697111797209));
#15831=CARTESIAN_POINT('Ctrl Pts',(2.08250507126076,-0.137631807827395,
-0.581897892437881));
#15832=CARTESIAN_POINT('Ctrl Pts',(2.0781993490831,-0.092050066932825,-0.584380246333738));
#15833=CARTESIAN_POINT('Ctrl Pts',(2.07602910338516,-0.0462123413419456,
-0.586862600229595));
#15834=CARTESIAN_POINT('Ctrl Pts',(2.07601908529222,-0.000319471822342703,
-0.589344954125452));
#15835=CARTESIAN_POINT('Origin',(3.53951905042299,8.32667268468867E-16,
0.));
#15836=CARTESIAN_POINT('',(2.07601962146617,0.00129284301226723,-1.1606550458429));
#15837=CARTESIAN_POINT('',(2.07601961090303,0.00128082971605478,-1.08934495412291));
#15838=CARTESIAN_POINT('',(2.07601905042299,1.01189432752408E-15,0.));
#15839=CARTESIAN_POINT('Ctrl Pts',(2.0758314534516,0.00129136347877342,
-1.16065495629856));
#15840=CARTESIAN_POINT('Ctrl Pts',(2.07926274667652,-0.376316335126734,
-1.14010981557906));
#15841=CARTESIAN_POINT('Ctrl Pts',(2.42031344695339,-1.24341589865127,-1.09323139624372));
#15842=CARTESIAN_POINT('Ctrl Pts',(3.87665396597672,-1.6937405805654,-1.0200196982925));
#15843=CARTESIAN_POINT('Ctrl Pts',(5.14228190560365,-0.643094266804824,
-0.941019862444937));
#15844=CARTESIAN_POINT('Ctrl Pts',(4.95387049003743,0.990974037173808,-0.862020026597378));
#15845=CARTESIAN_POINT('Ctrl Pts',(3.48234893238356,1.72601944824263,-0.783020190749813));
#15846=CARTESIAN_POINT('Ctrl Pts',(2.27614682897861,1.02013058486133,-0.715898530498322));
#15847=CARTESIAN_POINT('Ctrl Pts',(2.07889778574151,0.266425253906884,-0.675110148862687));
#15848=CARTESIAN_POINT('Ctrl Pts',(2.07827644886075,-0.000378700063536769,
-0.660655045842906));
#15849=CARTESIAN_POINT('Ctrl Pts',(2.0760190852921,-0.000319471237557788,
-0.589344954157083));
#15850=CARTESIAN_POINT('Ctrl Pts',(2.07600660206653,0.0568662720460612,
-0.592438141706959));
#15851=CARTESIAN_POINT('Ctrl Pts',(2.07935021510889,0.114012335576273,-0.595531329256835));
#15852=CARTESIAN_POINT('Ctrl Pts',(2.08601001953359,0.170715398025394,-0.598624516806711));
#15853=CARTESIAN_POINT('Ctrl Pts',(2.0926839307849,0.227538569147198,-0.601724256359864));
#15854=CARTESIAN_POINT('Ctrl Pts',(2.10268800075576,0.283916388418001,-0.604823995913016));
#15855=CARTESIAN_POINT('Ctrl Pts',(2.11593075498151,0.339453406349121,-0.607923735466169));
#15856=CARTESIAN_POINT('Ctrl Pts',(2.12918839109451,0.3950528354392,-0.611026958431741));
#15857=CARTESIAN_POINT('Ctrl Pts',(2.14569182168071,0.449809122313612,-0.614130181397313));
#15858=CARTESIAN_POINT('Ctrl Pts',(2.16529992555855,0.503342872063173,-0.617233404362885));
#15859=CARTESIAN_POINT('Ctrl Pts',(2.18495683587771,0.557009872423416,-0.620344351546491));
#15860=CARTESIAN_POINT('Ctrl Pts',(2.20773366690345,0.609447815871552,-0.623455298730097));
#15861=CARTESIAN_POINT('Ctrl Pts',(2.2334416826662,0.660298538112488,-0.626566245913703));
#15862=CARTESIAN_POINT('Ctrl Pts',(2.24840575064842,0.689897620032354,-0.628377059535968));
#15863=CARTESIAN_POINT('Ctrl Pts',(2.2643620934822,0.718959412202586,-0.630187873158234));
#15864=CARTESIAN_POINT('Ctrl Pts',(2.28126677168813,0.747417857064255,-0.631998686780499));
#15865=CARTESIAN_POINT('Ctrl Pts',(2.30936925475481,0.794727421617148,-0.635008998987377));
#15866=CARTESIAN_POINT('Ctrl Pts',(2.34020265453032,0.840549132069048,-0.638019311194254));
#15867=CARTESIAN_POINT('Ctrl Pts',(2.37358438157033,0.884549940912008,-0.641029623401131));
#15868=CARTESIAN_POINT('Ctrl Pts',(2.40690680684453,0.928472583467816,-0.644034587867034));
#15869=CARTESIAN_POINT('Ctrl Pts',(2.44276825883579,0.970580326613127,-0.647039552332936));
#15870=CARTESIAN_POINT('Ctrl Pts',(2.4809420158884,1.01056761869553,-0.650044516798839));
#15871=CARTESIAN_POINT('Ctrl Pts',(2.51907802320109,1.05051536764692,-0.653046509678085));
#15872=CARTESIAN_POINT('Ctrl Pts',(2.55952144303372,1.08834643934595,-0.656048502557331));
#15873=CARTESIAN_POINT('Ctrl Pts',(2.60200548448817,1.12378848707761,-0.659050495436577));
#15874=CARTESIAN_POINT('Ctrl Pts',(2.64446428811698,1.15920948030996,-0.662050704969176));
#15875=CARTESIAN_POINT('Ctrl Pts',(2.68896090595273,1.19224392497055,-0.665050914501775));
#15876=CARTESIAN_POINT('Ctrl Pts',(2.73519359964849,1.22265809580455,-0.668051124034374));
#15877=CARTESIAN_POINT('Ctrl Pts',(2.78141708196249,1.25306620693239,-0.671050735806533));
#15878=CARTESIAN_POINT('Ctrl Pts',(2.82937551230304,1.28085479098956,-0.674050347578691));
#15879=CARTESIAN_POINT('Ctrl Pts',(2.87873806733833,1.30583335169296,-0.67704995935085));
#15880=CARTESIAN_POINT('Ctrl Pts',(2.92814598812326,1.33083486848384,-0.680052327861118));
#15881=CARTESIAN_POINT('Ctrl Pts',(2.9789601395582,1.35302096349533,-0.683054696371386));
#15882=CARTESIAN_POINT('Ctrl Pts',(3.03082631367031,1.37224777266173,-0.686057064881654));
#15883=CARTESIAN_POINT('Ctrl Pts',(3.08271609195816,1.39148333190446,-0.68906079976288));
#15884=CARTESIAN_POINT('Ctrl Pts',(3.13565834171609,1.40775676518443,-0.692064534644105));
#15885=CARTESIAN_POINT('Ctrl Pts',(3.18928329956362,1.42097402116294,-0.695068269525331));
#15886=CARTESIAN_POINT('Ctrl Pts',(3.24300941273362,1.43421620948349,-0.698077670495309));
#15887=CARTESIAN_POINT('Ctrl Pts',(3.29742028630907,1.44439060667992,-0.701087071465287));
#15888=CARTESIAN_POINT('Ctrl Pts',(3.35213671825168,1.45145448140479,-0.704096472435265));
#15889=CARTESIAN_POINT('Ctrl Pts',(3.39396736421813,1.45685480507862,-0.706397155832865));
#15890=CARTESIAN_POINT('Ctrl Pts',(3.43597638473564,1.46043822272066,-0.708697839230464));
#15891=CARTESIAN_POINT('Ctrl Pts',(3.47799436027132,1.46220619698514,-0.710998522628063));
#15892=CARTESIAN_POINT('Ctrl Pts',(3.53297023865442,1.46451939596508,-0.714008712649165));
#15893=CARTESIAN_POINT('Ctrl Pts',(3.58819220241263,1.46373267579113,-0.717018902670267));
#15894=CARTESIAN_POINT('Ctrl Pts',(3.64328157668237,1.45981697076869,-0.720029092691368));
#15895=CARTESIAN_POINT('Ctrl Pts',(3.69827309153389,1.45590822150897,-0.723033935484477));
#15896=CARTESIAN_POINT('Ctrl Pts',(3.75313196180096,1.44888155494064,-0.726038778277585));
#15897=CARTESIAN_POINT('Ctrl Pts',(3.80747842507802,1.43875989085549,-0.729043621070694));
#15898=CARTESIAN_POINT('Ctrl Pts',(3.86177115079996,1.42864823502936,-0.732045492687842));
#15899=CARTESIAN_POINT('Ctrl Pts',(3.91555195660093,1.41544774026222,-0.73504736430499));
#15900=CARTESIAN_POINT('Ctrl Pts',(3.96844699483531,1.39923302866328,-0.738049235922138));
#15901=CARTESIAN_POINT('Ctrl Pts',(4.02131062043758,1.3830279464509,-0.741049324825975));
#15902=CARTESIAN_POINT('Ctrl Pts',(4.07328901720444,1.36381234986653,-0.744049413729812));
#15903=CARTESIAN_POINT('Ctrl Pts',(4.12402158794504,1.34171123332492,-0.747049502633649));
#15904=CARTESIAN_POINT('Ctrl Pts',(4.17474406482655,1.319614514068,-0.750048994633481));
#15905=CARTESIAN_POINT('Ctrl Pts',(4.22422072407499,1.29463362581086,-0.753048486633313));
#15906=CARTESIAN_POINT('Ctrl Pts',(4.27211128175114,1.26694154269155,-0.756047978633146));
#15907=CARTESIAN_POINT('Ctrl Pts',(4.32004589092698,1.23922398737375,-0.759050229676248));
#15908=CARTESIAN_POINT('Ctrl Pts',(4.36639102558828,1.20879051971965,-0.762052480719351));
#15909=CARTESIAN_POINT('Ctrl Pts',(4.41083268022885,1.17585917886223,-0.765054731762454));
#15910=CARTESIAN_POINT('Ctrl Pts',(4.45529457724241,1.14291283837235,-0.768058350276816));
#15911=CARTESIAN_POINT('Ctrl Pts',(4.49785085945377,1.10746669525194,-0.771061968791179));
#15912=CARTESIAN_POINT('Ctrl Pts',(4.53822074234987,1.06977903351225,-0.774065587305542));
#15913=CARTESIAN_POINT('Ctrl Pts',(4.57866682389853,1.03202023584555,-0.777074875186947));
#15914=CARTESIAN_POINT('Ctrl Pts',(4.61691789626551,0.992011850335824,-0.780084163068352));
#15915=CARTESIAN_POINT('Ctrl Pts',(4.65273100036834,0.95004810641297,-0.783093450949757));
#15916=CARTESIAN_POINT('Ctrl Pts',(4.68012243889575,0.917952387797172,-0.785395086791713));
#15917=CARTESIAN_POINT('Ctrl Pts',(4.70608847507237,0.884713570282592,-0.787696722633669));
#15918=CARTESIAN_POINT('Ctrl Pts',(4.73053765491137,0.850474534458592,-0.789998358475625));
#15919=CARTESIAN_POINT('Ctrl Pts',(4.7625119027294,0.805697268975813,-0.793008401155264));
#15920=CARTESIAN_POINT('Ctrl Pts',(4.79202470621447,0.759020214552427,-0.796018443834904));
#15921=CARTESIAN_POINT('Ctrl Pts',(4.8188448036111,0.710744586493403,-0.799028486514543));
#15922=CARTESIAN_POINT('Ctrl Pts',(4.84561721419754,0.662554793719687,-0.802033177262316));
#15923=CARTESIAN_POINT('Ctrl Pts',(4.86970616548129,0.612772525820783,-0.805037868010089));
#15924=CARTESIAN_POINT('Ctrl Pts',(4.89092333713011,0.561728318557669,-0.808042558757862));
#15925=CARTESIAN_POINT('Ctrl Pts',(4.91211950875181,0.51073463309616,-0.811044275566025));
#15926=CARTESIAN_POINT('Ctrl Pts',(4.93044932963856,0.458481967818713,-0.814045992374187));
#15927=CARTESIAN_POINT('Ctrl Pts',(4.94577101057565,0.405324159860732,-0.81704770918235));
#15928=CARTESIAN_POINT('Ctrl Pts',(4.96108357933088,0.35219796616328,-0.820047640795433));
#15929=CARTESIAN_POINT('Ctrl Pts',(4.97339140809001,0.298168203226823,-0.823047572408517));
#15930=CARTESIAN_POINT('Ctrl Pts',(4.98260213412084,0.243605138585195,-0.8260475040216));
#15931=CARTESIAN_POINT('Ctrl Pts',(4.99181102070509,0.189052970570174,-0.829046836527304));
#15932=CARTESIAN_POINT('Ctrl Pts',(4.99792394503188,0.133968232852556,-0.832046169033009));
#15933=CARTESIAN_POINT('Ctrl Pts',(5.00089982697954,0.0787304001702604,
-0.835045501538713));
#15934=CARTESIAN_POINT('Ctrl Pts',(5.00387844426227,0.0234417946470128,
-0.838047590934485));
#15935=CARTESIAN_POINT('Ctrl Pts',(5.00371422988948,-0.0319996584614357,
-0.841049680330258));
#15936=CARTESIAN_POINT('Ctrl Pts',(5.00041820516007,-0.0872118666724785,
-0.84405176972603));
#15937=CARTESIAN_POINT('Ctrl Pts',(4.99712068065652,-0.142449197826518,
-0.847055225147961));
#15938=CARTESIAN_POINT('Ctrl Pts',(4.9906885665012,-0.197456550651928,-0.850058680569893));
#15939=CARTESIAN_POINT('Ctrl Pts',(4.98118474231087,-0.251857663837041,
-0.853062135991825));
#15940=CARTESIAN_POINT('Ctrl Pts',(4.97166297965463,-0.306361459110359,
-0.856071260435152));
#15941=CARTESIAN_POINT('Ctrl Pts',(4.95905804543009,-0.360256213337277,
-0.859080384878479));
#15942=CARTESIAN_POINT('Ctrl Pts',(4.94348359275872,-0.413177702525217,
-0.862089509321806));
#15943=CARTESIAN_POINT('Ctrl Pts',(4.93156440168926,-0.453678730370079,
-0.864392404322266));
#15944=CARTESIAN_POINT('Ctrl Pts',(4.91790705213559,-0.493609960797262,
-0.866695299322727));
#15945=CARTESIAN_POINT('Ctrl Pts',(4.90258136217741,-0.532816463967382,
-0.868998194323188));
#15946=CARTESIAN_POINT('Ctrl Pts',(4.88254883971817,-0.584064085278177,
-0.872008355428095));
#15947=CARTESIAN_POINT('Ctrl Pts',(4.85958004900699,-0.634288036042029,
-0.875018516533003));
#15948=CARTESIAN_POINT('Ctrl Pts',(4.83380094152019,-0.683130028894825,
-0.87802867763791));
#15949=CARTESIAN_POINT('Ctrl Pts',(4.80806764621134,-0.731885224403334,
-0.881033489370802));
#15950=CARTESIAN_POINT('Ctrl Pts',(4.77953418972623,-0.779262872458853,
-0.884038301103693));
#15951=CARTESIAN_POINT('Ctrl Pts',(4.74837454173321,-0.824924633605481,
-0.887043112836585));
#15952=CARTESIAN_POINT('Ctrl Pts',(4.71724571796304,-0.870541224527396,
-0.890044952103724));
#15953=CARTESIAN_POINT('Ctrl Pts',(4.68349614525756,-0.914444856972351,
-0.893046791370863));
#15954=CARTESIAN_POINT('Ctrl Pts',(4.64734473137058,-0.956323434112651,
-0.896048630638002));
#15955=CARTESIAN_POINT('Ctrl Pts',(4.6112148016848,-0.99817712349115,-0.899048685960563));
#15956=CARTESIAN_POINT('Ctrl Pts',(4.57268620437191,-1.03800774393927,-0.902048741283124));
#15957=CARTESIAN_POINT('Ctrl Pts',(4.53201861258053,-1.07553561964125,-0.905048796605685));
#15958=CARTESIAN_POINT('Ctrl Pts',(4.49135912810842,-1.11305601394449,-0.908048253849891));
#15959=CARTESIAN_POINT('Ctrl Pts',(4.44856188390119,-1.14827421724515,-0.911047711094098));
#15960=CARTESIAN_POINT('Ctrl Pts',(4.40392228318567,-1.18094847524752,-0.914047168338305));
#15961=CARTESIAN_POINT('Ctrl Pts',(4.35924164396133,-1.21365277166428,-0.917049383072511));
#15962=CARTESIAN_POINT('Ctrl Pts',(4.31271569143074,-1.24380813772664,-0.920051597806717));
#15963=CARTESIAN_POINT('Ctrl Pts',(4.26467048770375,-1.27121502626804,-0.923053812540923));
#15964=CARTESIAN_POINT('Ctrl Pts',(4.21660341469196,-1.2986343899163,-0.926057393827541));
#15965=CARTESIAN_POINT('Ctrl Pts',(4.16701618560658,-1.32330254651983,-0.929060975114158));
#15966=CARTESIAN_POINT('Ctrl Pts',(4.11625831286334,-1.34506656830053,-0.932064556400776));
#15967=CARTESIAN_POINT('Ctrl Pts',(4.06540465061443,-1.36687166282078,-0.935073806001513));
#15968=CARTESIAN_POINT('Ctrl Pts',(4.0133764290597,-1.38576149341699,-0.93808305560225));
#15969=CARTESIAN_POINT('Ctrl Pts',(3.96054082058473,-1.40163223387944,-0.941092305202986));
#15970=CARTESIAN_POINT('Ctrl Pts',(3.92012452316368,-1.41377246629725,-0.943394213525574));
#15971=CARTESIAN_POINT('Ctrl Pts',(3.87923617383144,-1.4241471248127,-0.945696121848163));
#15972=CARTESIAN_POINT('Ctrl Pts',(3.838043453164,-1.43273006214294,-0.947998030170751));
#15973=CARTESIAN_POINT('Ctrl Pts',(3.78417701582501,-1.44395370186357,-0.951008163961618));
#15974=CARTESIAN_POINT('Ctrl Pts',(3.72956356181104,-1.45215886917292,-0.954018297752485));
#15975=CARTESIAN_POINT('Ctrl Pts',(3.6745719787831,-1.45725528187115,-0.957028431543353));
#15976=CARTESIAN_POINT('Ctrl Pts',(3.6196781255751,-1.46234263733792,-0.960033215791305));
#15977=CARTESIAN_POINT('Ctrl Pts',(3.56440799855432,-1.4643321538756,-0.963038000039257));
#15978=CARTESIAN_POINT('Ctrl Pts',(3.5091400161177,-1.46318466513105,-0.966042784287209));
#15979=CARTESIAN_POINT('Ctrl Pts',(3.45392670874686,-1.46203831156496,-0.969044595986333));
#15980=CARTESIAN_POINT('Ctrl Pts',(3.39871606716211,-1.45776111121616,-0.972046407685458));
#15981=CARTESIAN_POINT('Ctrl Pts',(3.34388908541655,-1.45036587342352,-0.975048219384582));
#15982=CARTESIAN_POINT('Ctrl Pts',(3.28909468735574,-1.44297503062199,-0.978048247106494));
#15983=CARTESIAN_POINT('Ctrl Pts',(3.23468401953469,-1.43246989369792,-0.981048274828406));
#15984=CARTESIAN_POINT('Ctrl Pts',(3.18103319700848,-1.41891512885784,-0.984048302550318));
#15985=CARTESIAN_POINT('Ctrl Pts',(3.12739306986512,-1.40536306618322,-0.987047732211594));
#15986=CARTESIAN_POINT('Ctrl Pts',(3.07451299892883,-1.38876271224259,-0.99004716187287));
#15987=CARTESIAN_POINT('Ctrl Pts',(3.02275686200019,-1.36922937837912,-0.993046591534146));
#15988=CARTESIAN_POINT('Ctrl Pts',(2.97095313936148,-1.34967808514663,-0.996048778935832));
#15989=CARTESIAN_POINT('Ctrl Pts',(2.9202759104247,-1.32718861132417,-0.999050966337517));
#15990=CARTESIAN_POINT('Ctrl Pts',(2.87107045544903,-1.30192500777784,-1.0020531537392));
#15991=CARTESIAN_POINT('Ctrl Pts',(2.82184260126877,-1.2766499037866,-1.00505670779038));
#15992=CARTESIAN_POINT('Ctrl Pts',(2.77408831276069,-1.24859842065337,-1.00806026184155));
#15993=CARTESIAN_POINT('Ctrl Pts',(2.72812663831067,-1.21797972214916,-1.01106381589272));
#15994=CARTESIAN_POINT('Ctrl Pts',(2.68207821720197,-1.18730323484983,-1.01407303875995));
#15995=CARTESIAN_POINT('Ctrl Pts',(2.63782959208944,-1.15405017102663,-1.01708226162718));
#15996=CARTESIAN_POINT('Ctrl Pts',(2.59566833675573,-1.11847131403081,-1.02009148449441));
#15997=CARTESIAN_POINT('Ctrl Pts',(2.56341397212314,-1.09125264092274,-1.02239361166905));
#15998=CARTESIAN_POINT('Ctrl Pts',(2.53238062274949,-1.06267364595761,-1.02469573884368));
#15999=CARTESIAN_POINT('Ctrl Pts',(2.50268184001776,-1.03286051774627,-1.02699786601831));
#16000=CARTESIAN_POINT('Ctrl Pts',(2.46440187434825,-0.994433167550155,
-1.02996517110983));
#16001=CARTESIAN_POINT('Ctrl Pts',(2.42816981499792,-0.953782886790655,
-1.03293247620135));
#16002=CARTESIAN_POINT('Ctrl Pts',(2.39425915283785,-0.911159709920974,
-1.03589978129287));
#16003=CARTESIAN_POINT('Ctrl Pts',(2.3603968099121,-0.868597266730304,-1.03886285827733));
#16004=CARTESIAN_POINT('Ctrl Pts',(2.32884965458755,-0.824067911680846,
-1.04182593526179));
#16005=CARTESIAN_POINT('Ctrl Pts',(2.29985429238519,-0.777858301799942,
-1.04478901224625));
#16006=CARTESIAN_POINT('Ctrl Pts',(2.27088801612938,-0.73169504589225,-1.04774911689679));
#16007=CARTESIAN_POINT('Ctrl Pts',(2.24446875270438,-0.683855331074661,
-1.05070922154733));
#16008=CARTESIAN_POINT('Ctrl Pts',(2.22079118378885,-0.634656650294132,
-1.05366932619786));
#16009=CARTESIAN_POINT('Ctrl Pts',(2.19701071433124,-0.585244156560942,
-1.05664229519161));
#16010=CARTESIAN_POINT('Ctrl Pts',(2.17599612692328,-0.534461322803746,
-1.05961526418537));
#16011=CARTESIAN_POINT('Ctrl Pts',(2.15789816163111,-0.482655124963916,
-1.06258823317912));
#16012=CARTESIAN_POINT('Ctrl Pts',(2.13988519957987,-0.431092252528085,
-1.06554723861424));
#16013=CARTESIAN_POINT('Ctrl Pts',(2.12476167223662,-0.378516136810143,
-1.06850624404935));
#16014=CARTESIAN_POINT('Ctrl Pts',(2.11262697227371,-0.325286408131106,
-1.07146524948447));
#16015=CARTESIAN_POINT('Ctrl Pts',(2.10040637676334,-0.27167989249402,-1.07444520025754));
#16016=CARTESIAN_POINT('Ctrl Pts',(2.09121722873746,-0.217411015904341,
-1.07742515103061));
#16017=CARTESIAN_POINT('Ctrl Pts',(2.08510855901616,-0.162856908007408,
-1.08040510180369));
#16018=CARTESIAN_POINT('Ctrl Pts',(2.07899988929486,-0.108302800110476,
-1.08338505257676));
#16019=CARTESIAN_POINT('Ctrl Pts',(2.07597169914304,-0.0534640227951241,
-1.08636500334984));
#16020=CARTESIAN_POINT('Ctrl Pts',(2.07601961090303,0.00128082971604727,
-1.08934495412291));
#16021=CARTESIAN_POINT('Origin',(3.53951905042299,8.32667268468867E-16,
0.));
#16022=CARTESIAN_POINT('',(2.07601930830571,-0.000868805298815955,-1.6606550458429));
#16023=CARTESIAN_POINT('',(2.07601934240537,-0.000924463273316875,-1.58934495415708));
#16024=CARTESIAN_POINT('',(2.07601905042299,1.01189432752408E-15,0.));
#16025=CARTESIAN_POINT('Ctrl Pts',(2.07601930830571,-0.000868805298815955,
-1.6606550458429));
#16026=CARTESIAN_POINT('Ctrl Pts',(2.07605060159967,-0.0535822587060049,
-1.6577761589196));
#16027=CARTESIAN_POINT('Ctrl Pts',(2.07892976381197,-0.106209644322961,
-1.6548972719963));
#16028=CARTESIAN_POINT('Ctrl Pts',(2.08462993641652,-0.158524180948704,
-1.652018385073));
#16029=CARTESIAN_POINT('Ctrl Pts',(2.09058996653434,-0.213223614723923,
-1.64900825644023));
#16030=CARTESIAN_POINT('Ctrl Pts',(2.09965160842919,-0.267701391860388,
-1.64599812780745));
#16031=CARTESIAN_POINT('Ctrl Pts',(2.11178681332887,-0.321578775982193,
-1.64298799917468));
#16032=CARTESIAN_POINT('Ctrl Pts',(2.1239004505508,-0.37536040481447,-1.63998322038848));
#16033=CARTESIAN_POINT('Ctrl Pts',(2.13907669513055,-0.428543247192843,
-1.63697844160228));
#16034=CARTESIAN_POINT('Ctrl Pts',(2.15723593766214,-0.480755287205635,
-1.63397366281607));
#16035=CARTESIAN_POINT('Ctrl Pts',(2.17537721463252,-0.532915672057198,
-1.63097185676054));
#16036=CARTESIAN_POINT('Ctrl Pts',(2.19649547077319,-0.584106660788554,
-1.62797005070501));
#16037=CARTESIAN_POINT('Ctrl Pts',(2.22046086605756,-0.633969838603209,
-1.62496824464948));
#16038=CARTESIAN_POINT('Ctrl Pts',(2.24441201730657,-0.683803379816431,
-1.62196822274276));
#16039=CARTESIAN_POINT('Ctrl Pts',(2.27120672528916,-0.732310199307741,
-1.61896820083604));
#16040=CARTESIAN_POINT('Ctrl Pts',(2.30066733449277,-0.77915253701489,-1.61596817892933));
#16041=CARTESIAN_POINT('Ctrl Pts',(2.33012206907523,-0.825985534080597,
-1.61296875524486));
#16042=CARTESIAN_POINT('Ctrl Pts',(2.36224136814464,-0.871154261717106,
-1.6099693315604));
#16043=CARTESIAN_POINT('Ctrl Pts',(2.39680318556378,-0.91434823902005,-1.60696990787594));
#16044=CARTESIAN_POINT('Ctrl Pts',(2.43139677757535,-0.957581926937968,
-1.60396772665521));
#16045=CARTESIAN_POINT('Ctrl Pts',(2.46843704357936,-0.998836824150021,
-1.60096554543448));
#16046=CARTESIAN_POINT('Ctrl Pts',(2.50766132347454,-1.03783518987206,-1.59796336421375));
#16047=CARTESIAN_POINT('Ctrl Pts',(2.54690345739522,-1.07685130678846,-1.59495981646646));
#16048=CARTESIAN_POINT('Ctrl Pts',(2.58833119117959,-1.11360849360256,-1.59195626871918));
#16049=CARTESIAN_POINT('Ctrl Pts',(2.63164705772915,-1.14786789086641,-1.58895272097189));
#16050=CARTESIAN_POINT('Ctrl Pts',(2.67504467569945,-1.18219194698678,-1.58594350453285));
#16051=CARTESIAN_POINT('Ctrl Pts',(2.72033711193837,-1.21400849197881,-1.58293428809381));
#16052=CARTESIAN_POINT('Ctrl Pts',(2.76719703399693,-1.24312145542726,-1.57992507165477));
#16053=CARTESIAN_POINT('Ctrl Pts',(2.80304679857745,-1.26539406792891,-1.57762289751166));
#16054=CARTESIAN_POINT('Ctrl Pts',(2.83981335928125,-1.28608518774595,-1.57532072336855));
#16055=CARTESIAN_POINT('Ctrl Pts',(2.8773416185596,-1.3051257788929,-1.57301854922543));
#16056=CARTESIAN_POINT('Ctrl Pts',(2.92641040360403,-1.33002164915373,-1.57000842058277));
#16057=CARTESIAN_POINT('Ctrl Pts',(2.97698825375561,-1.35219872375612,-1.5669982919401));
#16058=CARTESIAN_POINT('Ctrl Pts',(3.02874264136784,-1.37147355423017,-1.56398816329744));
#16059=CARTESIAN_POINT('Ctrl Pts',(3.0804050468403,-1.39071412789561,-1.56098338450212));
#16060=CARTESIAN_POINT('Ctrl Pts',(3.13323934918813,-1.40706251090189,-1.55797860570681));
#16061=CARTESIAN_POINT('Ctrl Pts',(3.18689047680632,-1.42038211023269,-1.55497382691149));
#16062=CARTESIAN_POINT('Ctrl Pts',(3.24048852551612,-1.43368853202512,-1.55197202084733));
#16063=CARTESIAN_POINT('Ctrl Pts',(3.29490128862576,-1.44397197940149,-1.54897021478317));
#16064=CARTESIAN_POINT('Ctrl Pts',(3.34975764001591,-1.45114536043786,-1.54596840871901));
#16065=CARTESIAN_POINT('Ctrl Pts',(3.40458138706076,-1.45831447791337,-1.54296838680416));
#16066=CARTESIAN_POINT('Ctrl Pts',(3.4598476772011,-1.46237712454654,-1.5399683648893));
#16067=CARTESIAN_POINT('Ctrl Pts',(3.51517655701911,-1.46329754083538,-1.53696834297445));
#16068=CARTESIAN_POINT('Ctrl Pts',(3.57049440391932,-1.46421777358758,-1.53396891928236));
#16069=CARTESIAN_POINT('Ctrl Pts',(3.62587428796392,-1.46199701157718,-1.53096949559027));
#16070=CARTESIAN_POINT('Ctrl Pts',(3.68093484790044,-1.45665157886978,-1.52797007189817));
#16071=CARTESIAN_POINT('Ctrl Pts',(3.73604602804309,-1.4513012318116,-1.52496789067064));
#16072=CARTESIAN_POINT('Ctrl Pts',(3.79083677078416,-1.44282052595196,-1.5219657094431));
#16073=CARTESIAN_POINT('Ctrl Pts',(3.84493094429205,-1.43127768971759,-1.51896352821556));
#16074=CARTESIAN_POINT('Ctrl Pts',(3.8990497402643,-1.41972959944095,-1.51595998046192));
#16075=CARTESIAN_POINT('Ctrl Pts',(3.9524708246704,-1.40511673990348,-1.51295643270828));
#16076=CARTESIAN_POINT('Ctrl Pts',(4.00483161143695,-1.38755773593845,-1.50995288495463));
#16077=CARTESIAN_POINT('Ctrl Pts',(4.05729122037734,-1.36996559230823,-1.50694366851004));
#16078=CARTESIAN_POINT('Ctrl Pts',(4.1086860425283,-1.34941639313085,-1.50393445206544));
#16079=CARTESIAN_POINT('Ctrl Pts',(4.15867301047219,-1.32607715603406,-1.50092523562084));
#16080=CARTESIAN_POINT('Ctrl Pts',(4.19691509245813,-1.30822168179233,-1.49862306153986));
#16081=CARTESIAN_POINT('Ctrl Pts',(4.23433356560751,-1.28873424481299,-1.49632088745887));
#16082=CARTESIAN_POINT('Ctrl Pts',(4.27078586574333,-1.26770702246664,-1.49401871337788));
#16083=CARTESIAN_POINT('Ctrl Pts',(4.31844782122865,-1.24021359868496,-1.49100858457507));
#16084=CARTESIAN_POINT('Ctrl Pts',(4.36465725919227,-1.20997075273416,-1.48799845577226));
#16085=CARTESIAN_POINT('Ctrl Pts',(4.40907884478412,-1.17715674998304,-1.48498832696945));
#16086=CARTESIAN_POINT('Ctrl Pts',(4.45342148071079,-1.14440106695409,-1.48198354801307));
#16087=CARTESIAN_POINT('Ctrl Pts',(4.49598214871869,-1.1090836069147,-1.47897876905669));
#16088=CARTESIAN_POINT('Ctrl Pts',(4.53645243873407,-1.07142711803957,-1.47597399010031));
#16089=CARTESIAN_POINT('Ctrl Pts',(4.57688269010578,-1.0338078840183,-1.47297218387464));
#16090=CARTESIAN_POINT('Ctrl Pts',(4.61522627552449,-0.993854563228126,
-1.46997037764897));
#16091=CARTESIAN_POINT('Ctrl Pts',(4.65120747129242,-0.95183039713219,-1.4669685714233));
#16092=CARTESIAN_POINT('Ctrl Pts',(4.68716728132948,-0.909831208458134,
-1.46396854934678));
#16093=CARTESIAN_POINT('Ctrl Pts',(4.72076714195681,-0.865764014414497,
-1.46096852727027));
#16094=CARTESIAN_POINT('Ctrl Pts',(4.75176949856182,-0.81992749739669,-1.45796850519376));
#16095=CARTESIAN_POINT('Ctrl Pts',(4.78276567310583,-0.774100120462913,
-1.45496908134014));
#16096=CARTESIAN_POINT('Ctrl Pts',(4.81116507655881,-0.726504558433568,
-1.45196965748652));
#16097=CARTESIAN_POINT('Ctrl Pts',(4.83677300646318,-0.677469131059185,
-1.4489702336329));
#16098=CARTESIAN_POINT('Ctrl Pts',(4.86240447913426,-0.628388622741825,
-1.44596805224533));
#16099=CARTESIAN_POINT('Ctrl Pts',(4.88523910601951,-0.577866073536125,
-1.44296587085776));
#16100=CARTESIAN_POINT('Ctrl Pts',(4.9051285132961,-0.526253783750209,-1.43996368947019));
#16101=CARTESIAN_POINT('Ctrl Pts',(4.92502697378405,-0.474618001209496,
-1.43696014155711));
#16102=CARTESIAN_POINT('Ctrl Pts',(4.94197738035999,-0.421891992946547,
-1.43395659364402));
#16103=CARTESIAN_POINT('Ctrl Pts',(4.95588096889684,-0.368444250731469,
-1.43095304573093));
#16104=CARTESIAN_POINT('Ctrl Pts',(4.96981079810235,-0.31489563495485,-1.42794382912983));
#16105=CARTESIAN_POINT('Ctrl Pts',(4.98068221806394,-0.260623083218473,
-1.42493461252873));
#16106=CARTESIAN_POINT('Ctrl Pts',(4.98844765983903,-0.206005181526372,
-1.42192539592764));
#16107=CARTESIAN_POINT('Ctrl Pts',(4.99438853788055,-0.164220270605003,
-1.41962322312853));
#16108=CARTESIAN_POINT('Ctrl Pts',(4.99851258859486,-0.122233456475762,
-1.41732105032942));
#16109=CARTESIAN_POINT('Ctrl Pts',(5.00081911649501,-0.0802145055330193,
-1.41501887753032));
#16110=CARTESIAN_POINT('Ctrl Pts',(5.00383493929472,-0.0252740427427241,
-1.41200874909616));
#16111=CARTESIAN_POINT('Ctrl Pts',(5.00375439789903,0.0299521711159732,
-1.408998620662));
#16112=CARTESIAN_POINT('Ctrl Pts',(5.00054356866753,0.0850858806637057,
-1.40598849222784));
#16113=CARTESIAN_POINT('Ctrl Pts',(4.99733844598335,0.140121602090493,-1.40298371363921));
#16114=CARTESIAN_POINT('Ctrl Pts',(4.99101410652874,0.195064622512907,-1.39997893505057));
#16115=CARTESIAN_POINT('Ctrl Pts',(4.9815885938022,0.24953493153882,-1.39697415646194));
#16116=CARTESIAN_POINT('Ctrl Pts',(4.97217240605668,0.303951351231319,-1.39397235060318));
#16117=CARTESIAN_POINT('Ctrl Pts',(4.95966121239473,0.357895468133609,-1.39097054474442));
#16118=CARTESIAN_POINT('Ctrl Pts',(4.94412483024175,0.410992522194417,-1.38796873888567));
#16119=CARTESIAN_POINT('Ctrl Pts',(4.9285976822637,0.46405801758988,-1.3849687171746));
#16120=CARTESIAN_POINT('Ctrl Pts',(4.9100490576525,0.516276942180214,-1.38196869546354));
#16121=CARTESIAN_POINT('Ctrl Pts',(4.88859931200724,0.567287138761122,-1.37896867375248));
#16122=CARTESIAN_POINT('Ctrl Pts',(4.86715384355899,0.618287163628853,-1.37596925026221));
#16123=CARTESIAN_POINT('Ctrl Pts',(4.84280860754731,0.668078452602508,-1.37296982677194));
#16124=CARTESIAN_POINT('Ctrl Pts',(4.81573219590353,0.716318544575429,-1.36997040328167));
#16125=CARTESIAN_POINT('Ctrl Pts',(4.78863089137961,0.764602986399556,-1.36696822225136));
#16126=CARTESIAN_POINT('Ctrl Pts',(4.75879365376755,0.811332920532059,-1.36396604122104));
#16127=CARTESIAN_POINT('Ctrl Pts',(4.7264344731455,0.856191584461946,-1.36096386019073));
#16128=CARTESIAN_POINT('Ctrl Pts',(4.69406056331908,0.90107066709267,-1.35796031263206));
#16129=CARTESIAN_POINT('Ctrl Pts',(4.65916275550649,0.944076370791778,-1.35495676507338));
#16130=CARTESIAN_POINT('Ctrl Pts',(4.62199570711233,0.984924635554761,-1.35195321751471));
#16131=CARTESIAN_POINT('Ctrl Pts',(4.58475851208888,1.02584999463136,-1.348944001259));
#16132=CARTESIAN_POINT('Ctrl Pts',(4.54524389884154,1.06460940998231,-1.34593478500329));
#16133=CARTESIAN_POINT('Ctrl Pts',(4.50374295181336,1.1009561835003,-1.34292556874758));
#16134=CARTESIAN_POINT('Ctrl Pts',(4.47199299994219,1.12876297810392,-1.34062339305931));
#16135=CARTESIAN_POINT('Ctrl Pts',(4.43908123842446,1.15515844654347,-1.33832121737103));
#16136=CARTESIAN_POINT('Ctrl Pts',(4.40514947174087,1.18004924629823,-1.33601904168276));
#16137=CARTESIAN_POINT('Ctrl Pts',(4.36078318702258,1.21259433359309,-1.33300891306169));
#16138=CARTESIAN_POINT('Ctrl Pts',(4.3144857366899,1.24270226555692,-1.32999878444062));
#16139=CARTESIAN_POINT('Ctrl Pts',(4.26655538408495,1.27013795295447,-1.32698865581956));
#16140=CARTESIAN_POINT('Ctrl Pts',(4.21871021728604,1.29752487936826,-1.32398387704924));
#16141=CARTESIAN_POINT('Ctrl Pts',(4.16923836214326,1.32224872606814,-1.32097909827893));
#16142=CARTESIAN_POINT('Ctrl Pts',(4.11846794650935,1.3441169687644,-1.31797431950861));
#16143=CARTESIAN_POINT('Ctrl Pts',(4.06774775983131,1.36596357643987,-1.3149725134715));
#16144=CARTESIAN_POINT('Ctrl Pts',(4.01573204026505,1.38495996870533,-1.31197070743439));
#16145=CARTESIAN_POINT('Ctrl Pts',(3.96277280743289,1.4009598520932,-1.30896890139728));
#16146=CARTESIAN_POINT('Ctrl Pts',(3.90984505141247,1.41695022580182,-1.30596887951145));
#16147=CARTESIAN_POINT('Ctrl Pts',(3.85597539817924,1.42994746826775,-1.30296885762563));
#16148=CARTESIAN_POINT('Ctrl Pts',(3.80153292599353,1.43985449924932,-1.29996883573981));
#16149=CARTESIAN_POINT('Ctrl Pts',(3.74710131000526,1.44975955470186,-1.29696941207865));
#16150=CARTESIAN_POINT('Ctrl Pts',(3.69209762120056,1.45657552793798,-1.2939699884175));
#16151=CARTESIAN_POINT('Ctrl Pts',(3.63690079797329,1.46025649981229,-1.29097056475635));
#16152=CARTESIAN_POINT('Ctrl Pts',(3.58165322931397,1.46394085580362,-1.28796838356241));
#16153=CARTESIAN_POINT('Ctrl Pts',(3.52621269957035,1.46448441700204,-1.28496620236847));
#16154=CARTESIAN_POINT('Ctrl Pts',(3.47096142924254,1.46189332804349,-1.28196402117453));
#16155=CARTESIAN_POINT('Ctrl Pts',(3.41568500979353,1.4593010596802,-1.27896047345602));
#16156=CARTESIAN_POINT('Ctrl Pts',(3.36059854768577,1.45357135162118,-1.27595692573751));
#16157=CARTESIAN_POINT('Ctrl Pts',(3.30607909466244,1.44476227700425,-1.272953378019));
#16158=CARTESIAN_POINT('Ctrl Pts',(3.25145674538153,1.43593657674711,-1.26994416161156));
#16159=CARTESIAN_POINT('Ctrl Pts',(3.19740405994049,1.42402001396884,-1.26693494520412));
#16160=CARTESIAN_POINT('Ctrl Pts',(3.14428670208302,1.40912158482711,-1.26392572879668));
#16161=CARTESIAN_POINT('Ctrl Pts',(3.10364973860981,1.39772367376262,-1.26162355447618));
#16162=CARTESIAN_POINT('Ctrl Pts',(3.06355998990276,1.38458157482829,-1.25932138015568));
#16163=CARTESIAN_POINT('Ctrl Pts',(3.02417311397034,1.36976305096237,-1.25701920583518));
#16164=CARTESIAN_POINT('Ctrl Pts',(2.97267414679388,1.35038759515105,-1.25400907626895));
#16165=CARTESIAN_POINT('Ctrl Pts',(2.92216118266346,1.32806308233131,-1.25099894670271));
#16166=CARTESIAN_POINT('Ctrl Pts',(2.87299408520618,1.30291086446569,-1.24798881713648));
#16167=CARTESIAN_POINT('Ctrl Pts',(2.82391437144947,1.27780334913466,-1.24498403741342));
#16168=CARTESIAN_POINT('Ctrl Pts',(2.77617624382463,1.24987834071752,-1.24197925769036));
#16169=CARTESIAN_POINT('Ctrl Pts',(2.73012023449984,1.21930546081866,-1.2389744779673));
#16170=CARTESIAN_POINT('Ctrl Pts',(2.68410978992882,1.18876282769465,-1.23597267097353));
#16171=CARTESIAN_POINT('Ctrl Pts',(2.63977860483815,1.15557780308831,-1.23297086397977));
#16172=CARTESIAN_POINT('Ctrl Pts',(2.59744154618989,1.1199652789341,-1.22996905698601));
#16173=CARTESIAN_POINT('Ctrl Pts',(2.55512965092677,1.08437392138167,-1.22696903414135));
#16174=CARTESIAN_POINT('Ctrl Pts',(2.5148099362524,1.04635826329255,-1.2239690112967));
#16175=CARTESIAN_POINT('Ctrl Pts',(2.47676537248869,1.00617437357405,-1.22096898845204));
#16176=CARTESIAN_POINT('Ctrl Pts',(2.43872839506025,0.965998496786419,-1.2179695638316));
#16177=CARTESIAN_POINT('Ctrl Pts',(2.40296603043599,0.923655630305217,-1.21497013921115));
#16178=CARTESIAN_POINT('Ctrl Pts',(2.36972378767427,0.879438055380055,-1.21197071459071));
#16179=CARTESIAN_POINT('Ctrl Pts',(2.3364509836035,0.835179828956672,-1.20896853244445));
#16180=CARTESIAN_POINT('Ctrl Pts',(2.30570324825082,0.78904387376498,-1.20596635029818));
#16181=CARTESIAN_POINT('Ctrl Pts',(2.27768427918276,0.741353667347177,-1.20296416815191));
#16182=CARTESIAN_POINT('Ctrl Pts',(2.2496525565439,0.69364175347745,-1.19996061948347));
#16183=CARTESIAN_POINT('Ctrl Pts',(2.22435231784351,0.644374648722026,-1.19695707081503));
#16184=CARTESIAN_POINT('Ctrl Pts',(2.20194094494239,0.593899875180095,-1.19395352214659));
#16185=CARTESIAN_POINT('Ctrl Pts',(2.17948727449227,0.543329839325739,-1.19094430480504));
#16186=CARTESIAN_POINT('Ctrl Pts',(2.15993354854111,0.491548076777288,-1.18793508746349));
#16187=CARTESIAN_POINT('Ctrl Pts',(2.14338827719297,0.438920396017478,-1.18492587012193));
#16188=CARTESIAN_POINT('Ctrl Pts',(2.13073050987142,0.398658201236042,-1.1826237034105));
#16189=CARTESIAN_POINT('Ctrl Pts',(2.1198325312392,0.357901299628314,-1.18032153669906));
#16190=CARTESIAN_POINT('Ctrl Pts',(2.11072263870117,0.316817082637371,-1.17801936998763));
#16191=CARTESIAN_POINT('Ctrl Pts',(2.09449554620332,0.243635386307748,-1.17391861116792));
#16192=CARTESIAN_POINT('Ctrl Pts',(2.08388602429248,0.169166356842432,-1.16981785234821));
#16193=CARTESIAN_POINT('Ctrl Pts',(2.07904990501698,0.0941388618851819,
-1.1657170935285));
#16194=CARTESIAN_POINT('Ctrl Pts',(2.07705997522901,0.0632671156302568,
-1.16402974429997));
#16195=CARTESIAN_POINT('Ctrl Pts',(2.07604701387719,0.0323010764233835,
-1.16234239507143));
#16196=CARTESIAN_POINT('Ctrl Pts',(2.07601962146617,0.00129284301226723,
-1.1606550458429));
#16197=CARTESIAN_POINT('Ctrl Pts',(2.07601961090358,0.00128083034372539,
-1.08934495415708));
#16198=CARTESIAN_POINT('Ctrl Pts',(2.076086813979,0.0780682547590463,-1.09352475799718));
#16199=CARTESIAN_POINT('Ctrl Pts',(2.08220099158433,0.154597466853534,-1.09770456183728));
#16200=CARTESIAN_POINT('Ctrl Pts',(2.0942199806277,0.230093130816347,-1.10188436567738));
#16201=CARTESIAN_POINT('Ctrl Pts',(2.09816260126035,0.254858172313705,-1.10325547774021));
#16202=CARTESIAN_POINT('Ctrl Pts',(2.10274024984205,0.279512224846894,-1.10462658980304));
#16203=CARTESIAN_POINT('Ctrl Pts',(2.10794686135528,0.30402848137613,-1.10599770186587));
#16204=CARTESIAN_POINT('Ctrl Pts',(2.11937743601969,0.357851375601575,-1.10900783595551));
#16205=CARTESIAN_POINT('Ctrl Pts',(2.13387162028759,0.411141823683592,-1.11201797004515));
#16206=CARTESIAN_POINT('Ctrl Pts',(2.15136341936914,0.463525828809443,-1.11502810413479));
#16207=CARTESIAN_POINT('Ctrl Pts',(2.16882413118407,0.515816734561915,-1.11803288846935));
#16208=CARTESIAN_POINT('Ctrl Pts',(2.18927171942787,0.567203897473393,-1.12103767280391));
#16209=CARTESIAN_POINT('Ctrl Pts',(2.21258956591817,0.617325192383872,-1.12404245713847));
#16210=CARTESIAN_POINT('Ctrl Pts',(2.23588434370741,0.667396901533078,-1.12704426879407));
#16211=CARTESIAN_POINT('Ctrl Pts',(2.26204353297963,0.71620474703446,-1.13004608044967));
#16212=CARTESIAN_POINT('Ctrl Pts',(2.29090190738579,0.76340518737667,-1.13304789210528));
#16213=CARTESIAN_POINT('Ctrl Pts',(2.3197431300039,0.810577574442678,-1.13604791965355));
#16214=CARTESIAN_POINT('Ctrl Pts',(2.35128008311007,0.856144000245483,-1.13904794720183));
#16215=CARTESIAN_POINT('Ctrl Pts',(2.38530204441923,0.89978628187571,-1.1420479747501));
#16216=CARTESIAN_POINT('Ctrl Pts',(2.41931722191452,0.943419861446911,-1.14504740410745));
#16217=CARTESIAN_POINT('Ctrl Pts',(2.45581609906172,0.985129642514446,-1.1480468334648));
#16218=CARTESIAN_POINT('Ctrl Pts',(2.49454653130814,1.02462904716525,-1.15104626282215));
#16219=CARTESIAN_POINT('Ctrl Pts',(2.53331257055859,1.06416476577846,-1.15404844971891));
#16220=CARTESIAN_POINT('Ctrl Pts',(2.57431389318075,1.10148567016794,-1.15705063661567));
#16221=CARTESIAN_POINT('Ctrl Pts',(2.61726123903304,1.13634184087809,-1.16005282351243));
#16222=CARTESIAN_POINT('Ctrl Pts',(2.66022813368107,1.17121387743859,-1.16305637694622));
#16223=CARTESIAN_POINT('Ctrl Pts',(2.70514238829615,1.20361863435593,-1.16605993038001));
#16224=CARTESIAN_POINT('Ctrl Pts',(2.75168402223468,1.23334837672067,-1.1690634838138));
#16225=CARTESIAN_POINT('Ctrl Pts',(2.79831349468582,1.2631342283392,-1.17207270588541));
#16226=CARTESIAN_POINT('Ctrl Pts',(2.8465760203861,1.29023472087032,-1.17508192795701));
#16227=CARTESIAN_POINT('Ctrl Pts',(2.89612620774829,1.31448769488154,-1.17809115002862));
#16228=CARTESIAN_POINT('Ctrl Pts',(2.93403332522867,1.33304181917519,-1.18039327925689));
#16229=CARTESIAN_POINT('Ctrl Pts',(2.9726935207184,1.34993033683131,-1.18269540848516));
#16230=CARTESIAN_POINT('Ctrl Pts',(3.0119455503449,1.36510016189852,-1.18499753771344));
#16231=CARTESIAN_POINT('Ctrl Pts',(3.0632691966508,1.38493533331972,-1.18800766654975));
#16232=CARTESIAN_POINT('Ctrl Pts',(3.11582084811984,1.40191373474239,-1.19101779538605));
#16233=CARTESIAN_POINT('Ctrl Pts',(3.16925121455922,1.41588628770984,-1.19402792422236));
#16234=CARTESIAN_POINT('Ctrl Pts',(3.22258662075321,1.42983400766291,-1.19703270324373));
#16235=CARTESIAN_POINT('Ctrl Pts',(3.27679713588248,1.440786348274,-1.20003748226509));
#16236=CARTESIAN_POINT('Ctrl Pts',(3.3315157520175,1.44864311610984,-1.20304226128645));
#16237=CARTESIAN_POINT('Ctrl Pts',(3.38618023350355,1.45649211102673,-1.20604406759635));
#16238=CARTESIAN_POINT('Ctrl Pts',(3.44135130002867,1.46125152521475,-1.20904587390625));
#16239=CARTESIAN_POINT('Ctrl Pts',(3.49665094853118,1.46287202989195,-1.21204768021614));
#16240=CARTESIAN_POINT('Ctrl Pts',(3.55191772956816,1.4644915714187,-1.21504770239598));
#16241=CARTESIAN_POINT('Ctrl Pts',(3.60731241427164,1.46297588577288,-1.21804772457581));
#16242=CARTESIAN_POINT('Ctrl Pts',(3.66245337918994,1.4583276040762,-1.22104774675565));
#16243=CARTESIAN_POINT('Ctrl Pts',(3.71758334900887,1.45368024924612,-1.22404717073155));
#16244=CARTESIAN_POINT('Ctrl Pts',(3.77245917356105,1.44590158320879,-1.22704659470745));
#16245=CARTESIAN_POINT('Ctrl Pts',(3.82670306639338,1.43504619820099,-1.23004601868335));
#16246=CARTESIAN_POINT('Ctrl Pts',(3.88099682911028,1.42418083314255,-1.23304820022181));
#16247=CARTESIAN_POINT('Ctrl Pts',(3.93465698043322,1.41023320174446,-1.23605038176026));
#16248=CARTESIAN_POINT('Ctrl Pts',(3.98731615649071,1.39330901159699,-1.23905256329871));
#16249=CARTESIAN_POINT('Ctrl Pts',(4.03999930210369,1.37637711784788,-1.24205611137881));
#16250=CARTESIAN_POINT('Ctrl Pts',(4.09168007052456,1.35646615468641,-1.2450596594589));
#16251=CARTESIAN_POINT('Ctrl Pts',(4.14200964300066,1.33373060842713,-1.248063207539));
#16252=CARTESIAN_POINT('Ctrl Pts',(4.19243420442704,1.31095215249136,-1.25107242433164));
#16253=CARTESIAN_POINT('Ctrl Pts',(4.2415020062414,1.28533870905188,-1.25408164112429));
#16254=CARTESIAN_POINT('Ctrl Pts',(4.2888885159357,1.25709094903957,-1.25709085791694));
#16255=CARTESIAN_POINT('Ctrl Pts',(4.32514110180467,1.23548027646505,-1.25939302979829));
#16256=CARTESIAN_POINT('Ctrl Pts',(4.36041014090153,1.2123287418024,-1.26169520167965));
#16257=CARTESIAN_POINT('Ctrl Pts',(4.39456306180988,1.18774239151064,-1.263997373561));
#16258=CARTESIAN_POINT('Ctrl Pts',(4.43921855961942,1.15559533988526,-1.26700750062103));
#16259=CARTESIAN_POINT('Ctrl Pts',(4.48215241690794,1.12085887548091,-1.27001762768105));
#16260=CARTESIAN_POINT('Ctrl Pts',(4.52304892570035,1.08374408161562,-1.27302775474107));
#16261=CARTESIAN_POINT('Ctrl Pts',(4.56387274924154,1.04669525177016,-1.27603253191065));
#16262=CARTESIAN_POINT('Ctrl Pts',(4.60266602221789,1.00727683301475,-1.27903730908023));
#16263=CARTESIAN_POINT('Ctrl Pts',(4.63914429820567,0.965741458382562,-1.28204208624981));
#16264=CARTESIAN_POINT('Ctrl Pts',(4.675586484654,0.924247176496708,-1.28504389066311));
#16265=CARTESIAN_POINT('Ctrl Pts',(4.70971786435798,0.880640482490543,-1.2880456950764));
#16266=CARTESIAN_POINT('Ctrl Pts',(4.74129058364919,0.835211010420215,-1.29104749948969));
#16267=CARTESIAN_POINT('Ctrl Pts',(4.77284453717947,0.789808540097948,-1.29404751973155));
#16268=CARTESIAN_POINT('Ctrl Pts',(4.80184254379426,0.74258587188108,-1.2970475399734));
#16269=CARTESIAN_POINT('Ctrl Pts',(4.82807828942966,0.693864062746124,-1.30004756021526));
#16270=CARTESIAN_POINT('Ctrl Pts',(4.85430880332614,0.645151969355036,-1.3030469822152));
#16271=CARTESIAN_POINT('Ctrl Pts',(4.87777789992078,0.594941793470117,-1.30604640421515));
#16272=CARTESIAN_POINT('Ctrl Pts',(4.8983248804711,0.543579769884119,-1.30904582621509));
#16273=CARTESIAN_POINT('Ctrl Pts',(4.91889075089191,0.492170526611925,-1.31204800573422));
#16274=CARTESIAN_POINT('Ctrl Pts',(4.93652894151735,0.439607811381876,-1.31505018525336));
#16275=CARTESIAN_POINT('Ctrl Pts',(4.95112725892788,0.386257059070259,-1.31805236477249));
#16276=CARTESIAN_POINT('Ctrl Pts',(4.96573222111481,0.33288202287649,-1.32105591080607));
#16277=CARTESIAN_POINT('Ctrl Pts',(4.97729444138771,0.27871875194974,-1.32405945683964));
#16278=CARTESIAN_POINT('Ctrl Pts',(4.98575271279183,0.224143801679205,-1.32706300287322));
#16279=CARTESIAN_POINT('Ctrl Pts',(4.99422694777541,0.169465850273618,-1.33007221760002));
#16280=CARTESIAN_POINT('Ctrl Pts',(4.99958547999956,0.114375194319197,-1.33308143232681));
#16281=CARTESIAN_POINT('Ctrl Pts',(5.00181905327494,0.0592532839526826,
-1.33609064705361));
#16282=CARTESIAN_POINT('Ctrl Pts',(5.00352783939816,0.0170824912781934,
-1.33839283450526));
#16283=CARTESIAN_POINT('Ctrl Pts',(5.00340868074502,-0.0251064766897208,
-1.34069502195691));
#16284=CARTESIAN_POINT('Ctrl Pts',(5.00147795791863,-0.0671446408445567,
-1.34299720940856));
#16285=CARTESIAN_POINT('Ctrl Pts',(4.99895352151999,-0.122109895449789,
-1.34600733894141));
#16286=CARTESIAN_POINT('Ctrl Pts',(4.99331967897896,-0.177048072556392,
-1.34901746847425));
#16287=CARTESIAN_POINT('Ctrl Pts',(4.98458071728794,-0.231579422569218,
-1.35202759800709));
#16288=CARTESIAN_POINT('Ctrl Pts',(4.97585728714247,-0.286013855330727,
-1.35503237770942));
#16289=CARTESIAN_POINT('Ctrl Pts',(4.9640397725431,-0.340042378639619,-1.35803715741174));
#16290=CARTESIAN_POINT('Ctrl Pts',(4.94918434067214,-0.393288722781086,
-1.36104193711407));
#16291=CARTESIAN_POINT('Ctrl Pts',(4.93434360573965,-0.446482388666503,
-1.36404374409485));
#16292=CARTESIAN_POINT('Ctrl Pts',(4.9164710485214,-0.498894902124361,-1.36704555107562));
#16293=CARTESIAN_POINT('Ctrl Pts',(4.89567381967488,-0.55016042372689,-1.3700473580564));
#16294=CARTESIAN_POINT('Ctrl Pts',(4.8748889517819,-0.601395475369454,-1.3730473808958));
#16295=CARTESIAN_POINT('Ctrl Pts',(4.85118305581007,-0.651484397970665,
-1.3760474037352));
#16296=CARTESIAN_POINT('Ctrl Pts',(4.82471229701215,-0.70007897334631,-1.37904742657459));
#16297=CARTESIAN_POINT('Ctrl Pts',(4.79824681658887,-0.748663858770234,
-1.3820468511975));
#16298=CARTESIAN_POINT('Ctrl Pts',(4.76901782073415,-0.795754525229392,
-1.3850462758204));
#16299=CARTESIAN_POINT('Ctrl Pts',(4.73722748580544,-0.841027201589646,
-1.38804570044331));
#16300=CARTESIAN_POINT('Ctrl Pts',(4.70540792425556,-0.886341499636643,
-1.39104788260391));
#16301=CARTESIAN_POINT('Ctrl Pts',(4.67102262322822,-0.929834035254669,
-1.39405006476452));
#16302=CARTESIAN_POINT('Ctrl Pts',(4.63431634276002,-0.971211171008397,
-1.39705224692513));
#16303=CARTESIAN_POINT('Ctrl Pts',(4.59759335438184,-1.01260714074505,-1.40005579561454));
#16304=CARTESIAN_POINT('Ctrl Pts',(4.55854765355551,-1.05188541597891,-1.40305934430394));
#16305=CARTESIAN_POINT('Ctrl Pts',(4.51746117282878,-1.08878898562782,-1.40606289299335));
#16306=CARTESIAN_POINT('Ctrl Pts',(4.47629714840745,-1.12576220444317,-1.40907211036642));
#16307=CARTESIAN_POINT('Ctrl Pts',(4.43308506318119,-1.16035143364744,-1.41208132773949));
#16308=CARTESIAN_POINT('Ctrl Pts',(4.38813933485548,-1.19234049786532,-1.41509054511257));
#16309=CARTESIAN_POINT('Ctrl Pts',(4.35375412870948,-1.21681335899193,-1.41739271182709));
#16310=CARTESIAN_POINT('Ctrl Pts',(4.31835493766681,-1.23976522522809,-1.41969487854161));
#16311=CARTESIAN_POINT('Ctrl Pts',(4.28209223229497,-1.26111748840642,-1.42199704525612));
#16312=CARTESIAN_POINT('Ctrl Pts',(4.23467802637467,-1.28903599566673,-1.42500717385921));
#16313=CARTESIAN_POINT('Ctrl Pts',(4.18558753179959,-1.31433549866122,-1.4280173024623));
#16314=CARTESIAN_POINT('Ctrl Pts',(4.13514114118776,-1.33681209412281,-1.43102743106538));
#16315=CARTESIAN_POINT('Ctrl Pts',(4.08478440798254,-1.35924874236054,-1.43403220982439));
#16316=CARTESIAN_POINT('Ctrl Pts',(4.03307703951899,-1.37887222633654,-1.4370369885834));
#16317=CARTESIAN_POINT('Ctrl Pts',(3.98036486107862,-1.39552399521734,-1.44004176734241));
#16318=CARTESIAN_POINT('Ctrl Pts',(3.9277048325768,-1.41215928994076,-1.4430435733723));
#16319=CARTESIAN_POINT('Ctrl Pts',(3.87404246445814,-1.42582853530268,-1.44604537940219));
#16320=CARTESIAN_POINT('Ctrl Pts',(3.81974270355202,-1.43642157956048,-1.44904718543208));
#16321=CARTESIAN_POINT('Ctrl Pts',(3.76547521613932,-1.44700832775844,-1.45204720731476));
#16322=CARTESIAN_POINT('Ctrl Pts',(3.71057160413364,-1.45452239787162,-1.45504722919743));
#16323=CARTESIAN_POINT('Ctrl Pts',(3.65540883750058,-1.45890431737352,-1.45804725108011));
#16324=CARTESIAN_POINT('Ctrl Pts',(3.60025707062169,-1.46328536309697,-1.46104667474219));
#16325=CARTESIAN_POINT('Ctrl Pts',(3.54484677790598,-1.46453545677763,-1.46404609840427));
#16326=CARTESIAN_POINT('Ctrl Pts',(3.48955959455852,-1.46264701919832,-1.46704552206635));
#16327=CARTESIAN_POINT('Ctrl Pts',(3.43422158259052,-1.46075684547202,-1.47004770326748));
#16328=CARTESIAN_POINT('Ctrl Pts',(3.37900743505493,-1.4557223938416,-1.47304988446862));
#16329=CARTESIAN_POINT('Ctrl Pts',(3.32429681693925,-1.44758821500255,-1.47605206566975));
#16330=CARTESIAN_POINT('Ctrl Pts',(3.26956129573133,-1.4394503336609,-1.47905561339895));
#16331=CARTESIAN_POINT('Ctrl Pts',(3.21533027885597,-1.42821001989111,-1.48205916112815));
#16332=CARTESIAN_POINT('Ctrl Pts',(3.16197306666285,-1.41396296986399,-1.48506270885735));
#16333=CARTESIAN_POINT('Ctrl Pts',(3.10851515164676,-1.39968903091037,-1.48807192528106));
#16334=CARTESIAN_POINT('Ctrl Pts',(3.05593483868087,-1.38239718497146,-1.49108114170476));
#16335=CARTESIAN_POINT('Ctrl Pts',(3.00458497687674,-1.36223264788333,-1.49409035812846));
#16336=CARTESIAN_POINT('Ctrl Pts',(2.96530022071548,-1.34680594769796,-1.49639253245354));
#16337=CARTESIAN_POINT('Ctrl Pts',(2.92673530585453,-1.32969893096072,-1.49869470677861));
#16338=CARTESIAN_POINT('Ctrl Pts',(2.88903828678348,-1.31099467052119,-1.50099688110369));
#16339=CARTESIAN_POINT('Ctrl Pts',(2.83974885266478,-1.28653856138068,-1.50400700955739));
#16340=CARTESIAN_POINT('Ctrl Pts',(2.79173698722558,-1.25924750199659,-1.50701713801109));
#16341=CARTESIAN_POINT('Ctrl Pts',(2.74534852619855,-1.22927841779358,-1.51002726646479));
#16342=CARTESIAN_POINT('Ctrl Pts',(2.69904251063669,-1.19936259716157,-1.51303204506564));
#16343=CARTESIAN_POINT('Ctrl Pts',(2.65435461369543,-1.16677848145454,-1.51603682366649));
#16344=CARTESIAN_POINT('Ctrl Pts',(2.611606583539,-1.13172907703269,-1.51904160226734));
#16345=CARTESIAN_POINT('Ctrl Pts',(2.56890084552963,-1.09671434823357,-1.52204340813382));
#16346=CARTESIAN_POINT('Ctrl Pts',(2.52813157888946,-1.05923949545577,-1.5250452140003));
#16347=CARTESIAN_POINT('Ctrl Pts',(2.48959044418768,-1.01954998494865,-1.52804701986678));
#16348=CARTESIAN_POINT('Ctrl Pts',(2.4510722167798,-0.979884064283605,-1.53104704158109));
#16349=CARTESIAN_POINT('Ctrl Pts',(2.41477986361633,-0.938006473007482,
-1.5340470632954));
#16350=CARTESIAN_POINT('Ctrl Pts',(2.38096916945945,-0.894200437999985,
-1.5370470850097));
#16351=CARTESIAN_POINT('Ctrl Pts',(2.34716521739095,-0.850403138221584,
-1.54004650849874));
#16352=CARTESIAN_POINT('Ctrl Pts',(2.31584226405684,-0.804678576239946,
-1.54304593198778));
#16353=CARTESIAN_POINT('Ctrl Pts',(2.28721518124924,-0.75734224050455,-1.54604535547683));
#16354=CARTESIAN_POINT('Ctrl Pts',(2.25856178000732,-0.709962385900982,
-1.54904753649903));
#16355=CARTESIAN_POINT('Ctrl Pts',(2.23260947481426,-0.660968249992565,
-1.55204971752123));
#16356=CARTESIAN_POINT('Ctrl Pts',(2.2095284007412,-0.610702154703102,-1.55505189854343));
#16357=CARTESIAN_POINT('Ctrl Pts',(2.18643682068818,-0.560413179430315,
-1.55805544609014));
#16358=CARTESIAN_POINT('Ctrl Pts',(2.16621927013087,-0.508851583173669,
-1.56105899363686));
#16359=CARTESIAN_POINT('Ctrl Pts',(2.14899738523307,-0.456378952886151,
-1.56406254118358));
#16360=CARTESIAN_POINT('Ctrl Pts',(2.13174299692356,-0.403807289332768,
-1.56707175742122));
#16361=CARTESIAN_POINT('Ctrl Pts',(2.11749570491818,-0.350321668506178,
-1.57008097365886));
#16362=CARTESIAN_POINT('Ctrl Pts',(2.10632668243752,-0.296296956360021,
-1.57309018989649));
#16363=CARTESIAN_POINT('Ctrl Pts',(2.09778191531256,-0.254965802708777,
-1.57539236558141));
#16364=CARTESIAN_POINT('Ctrl Pts',(2.0910377791532,-0.213319416672938,-1.57769454126633));
#16365=CARTESIAN_POINT('Ctrl Pts',(2.08610559463042,-0.171527188868424,
-1.57999671695125));
#16366=CARTESIAN_POINT('Ctrl Pts',(2.07942970231923,-0.114959878586476,
-1.58311279601986));
#16367=CARTESIAN_POINT('Ctrl Pts',(2.07605539298674,-0.057995432812559,
-1.58622887508847));
#16368=CARTESIAN_POINT('Ctrl Pts',(2.07601934240537,-0.000924463273316875,
-1.58934495415708));
#16369=CARTESIAN_POINT('Origin',(3.53951905042299,8.32667268468867E-16,
0.));
#16370=CARTESIAN_POINT('',(2.07822263712103,-0.00047059340223754,-2.16065504584291));
#16371=CARTESIAN_POINT('',(2.07826209366837,-0.000404147104298556,-2.08934495415708));
#16372=CARTESIAN_POINT('',(2.07601905042299,1.01189432752408E-15,0.));
#16373=CARTESIAN_POINT('Ctrl Pts',(2.07822263712103,-0.00047059340223754,
-2.16065504584291));
#16374=CARTESIAN_POINT('Ctrl Pts',(2.07760197824254,-0.213557672618783,
-2.14910916394806));
#16375=CARTESIAN_POINT('Ctrl Pts',(2.22069645106389,-0.91184954544291,-2.11123000343738));
#16376=CARTESIAN_POINT('Ctrl Pts',(3.29376990923637,-1.70939328955503,-2.04701756431081));
#16377=CARTESIAN_POINT('Ctrl Pts',(4.8369055691126,-1.139827302423,-1.96801772846324));
#16378=CARTESIAN_POINT('Ctrl Pts',(5.20304199322948,0.46379896208315,-1.88901789261569));
#16379=CARTESIAN_POINT('Ctrl Pts',(4.06001734279725,1.64666316760928,-1.81001805676813));
#16380=CARTESIAN_POINT('Ctrl Pts',(2.50365865871826,1.34699592201261,-1.73389733257609));
#16381=CARTESIAN_POINT('Ctrl Pts',(2.0773938370103,0.429087924422116,-1.6841098869999));
#16382=CARTESIAN_POINT('Ctrl Pts',(2.07435250273762,-0.000857435948038469,
-1.66065572003956));
#16383=CARTESIAN_POINT('Ctrl Pts',(2.07445498749166,-0.000913275611314609,
-1.58934561824827));
#16384=CARTESIAN_POINT('Ctrl Pts',(2.07761216204631,0.424762299842239,-1.61256259643179));
#16385=CARTESIAN_POINT('Ctrl Pts',(2.49649649616959,1.33865665927285,-1.66211285323115));
#16386=CARTESIAN_POINT('Ctrl Pts',(4.04527237248975,1.65125152232427,-1.73799638864638));
#16387=CARTESIAN_POINT('Ctrl Pts',(5.19882826886049,0.478655327125651,-1.81699622449393));
#16388=CARTESIAN_POINT('Ctrl Pts',(4.84704581275503,-1.12818073352081,-1.89599606034151));
#16389=CARTESIAN_POINT('Ctrl Pts',(3.30906481316853,-1.71152237792777,-1.97499589618906));
#16390=CARTESIAN_POINT('Ctrl Pts',(2.22491280319792,-0.920695290287707,
-2.03944552746092));
#16391=CARTESIAN_POINT('Ctrl Pts',(2.07771897242739,-0.217883449584588,
-2.07756188011693));
#16392=CARTESIAN_POINT('Ctrl Pts',(2.07826209366837,-0.000404147104298556,
-2.08934495415708));
#16393=CARTESIAN_POINT('Origin',(3.53951905042299,8.32667268468867E-16,
0.));
#16394=CARTESIAN_POINT('',(2.07601386707336,0.00130271582805805,-2.66065504584291));
#16395=CARTESIAN_POINT('',(2.07601962469904,0.00129649745615735,-2.58934495415708));
#16396=CARTESIAN_POINT('',(2.07601905042299,1.01189432752408E-15,0.));
#16397=CARTESIAN_POINT('Ctrl Pts',(2.07601386707336,0.00130271582805805,
-2.66065504584291));
#16398=CARTESIAN_POINT('Ctrl Pts',(2.07937356612051,-0.37031688775017,-2.64044216897652));
#16399=CARTESIAN_POINT('Ctrl Pts',(2.411408495879,-1.2314244916919,-2.59389601349429));
#16400=CARTESIAN_POINT('Ctrl Pts',(3.85541032199574,-1.69783119393702,-2.52101657939618));
#16401=CARTESIAN_POINT('Ctrl Pts',(5.13410011968933,-0.663120857830193,
-2.44201674354863));
#16402=CARTESIAN_POINT('Ctrl Pts',(4.96617345192722,0.973177926803775,-2.36301690770107));
#16403=CARTESIAN_POINT('Ctrl Pts',(3.50397471012939,1.72660205561732,-2.28401707185351));
#16404=CARTESIAN_POINT('Ctrl Pts',(2.28301066241746,1.03245433367608,-2.21656311790078));
#16405=CARTESIAN_POINT('Ctrl Pts',(2.07901754643573,0.27244083988585,-2.17544244256392));
#16406=CARTESIAN_POINT('Ctrl Pts',(2.07822263712103,-0.00047059340223754,
-2.16065504584291));
#16407=CARTESIAN_POINT('Ctrl Pts',(2.07826209366837,-0.000404147104298556,
-2.08934495415708));
#16408=CARTESIAN_POINT('Ctrl Pts',(2.07893276119865,0.268147873470814,-2.10389515873278));
#16409=CARTESIAN_POINT('Ctrl Pts',(2.27810024031952,1.02365674713459,-2.14477864192436));
#16410=CARTESIAN_POINT('Ctrl Pts',(3.48853717707201,1.72621518156014,-2.21199540373174));
#16411=CARTESIAN_POINT('Ctrl Pts',(4.95741442700981,0.985895889670252,-2.29099523957932));
#16412=CARTESIAN_POINT('Ctrl Pts',(5.13996585904884,-0.648835893708398,
-2.36999507542687));
#16413=CARTESIAN_POINT('Ctrl Pts',(3.8705793808516,-1.69493866021592,-2.44899491127443));
#16414=CARTESIAN_POINT('Ctrl Pts',(2.41775219469909,-1.2399868630121,-2.52211151597577));
#16415=CARTESIAN_POINT('Ctrl Pts',(2.07929642712637,-0.374598926333502,
-2.56889484206127));
#16416=CARTESIAN_POINT('Ctrl Pts',(2.07588373256422,0.00129542995082815,
-2.5893448895309));
#16417=CARTESIAN_POINT('Origin',(3.53951905042299,8.32667268468867E-16,
0.));
#16418=CARTESIAN_POINT('',(2.07601926119859,-0.000785455376519445,-3.16065504584291));
#16419=CARTESIAN_POINT('',(2.07601929469955,-0.000845575214941048,-3.08934495419128));
#16420=CARTESIAN_POINT('',(2.07601905042299,1.01189432752408E-15,0.));
#16421=CARTESIAN_POINT('Ctrl Pts',(2.07421776459465,-0.000786422233640862,
-3.16065504584291));
#16422=CARTESIAN_POINT('Ctrl Pts',(2.07391318880368,-0.0474574829802449,
-3.15810845262083));
#16423=CARTESIAN_POINT('Ctrl Pts',(2.09703130803367,-0.57642940013294,-3.12922858078293));
#16424=CARTESIAN_POINT('Ctrl Pts',(2.73890147350281,-1.53017304710381,-3.07401543032911));
#16425=CARTESIAN_POINT('Ctrl Pts',(4.38362585771088,-1.50661931371105,-2.99501559448158));
#16426=CARTESIAN_POINT('Ctrl Pts',(5.26256991907278,-0.116248710108447,
-2.91601575863399));
#16427=CARTESIAN_POINT('Ctrl Pts',(4.57834870433128,1.37958363599936,-2.83701592278644));
#16428=CARTESIAN_POINT('Ctrl Pts',(2.95169307147619,1.62384687610397,-2.75801608693887));
#16429=CARTESIAN_POINT('Ctrl Pts',(2.13806849098069,0.709370374933544,-2.6992291279577));
#16430=CARTESIAN_POINT('Ctrl Pts',(2.07499655973696,0.113828077107039,-2.66677544759238));
#16431=CARTESIAN_POINT('Ctrl Pts',(2.07601386707336,0.00130271582805805,
-2.66065504584291));
#16432=CARTESIAN_POINT('Ctrl Pts',(2.07601962469904,0.00129649745615735,
-2.58934495415708));
#16433=CARTESIAN_POINT('Ctrl Pts',(2.07608591186512,0.076122120167986,-2.59341615963068));
#16434=CARTESIAN_POINT('Ctrl Pts',(2.08189439960235,0.150699246533157,-2.59748736510427));
#16435=CARTESIAN_POINT('Ctrl Pts',(2.09330987021167,0.224301709918793,-2.60155857057787));
#16436=CARTESIAN_POINT('Ctrl Pts',(2.09839064543428,0.257060549662797,-2.60337057470843));
#16437=CARTESIAN_POINT('Ctrl Pts',(2.1045815205659,0.289626688434001,-2.605182578839));
#16438=CARTESIAN_POINT('Ctrl Pts',(2.11186768165337,0.321937601485487,-2.60699458296956));
#16439=CARTESIAN_POINT('Ctrl Pts',(2.12397156262673,0.375612978823534,-2.61000471163077));
#16440=CARTESIAN_POINT('Ctrl Pts',(2.13913213185262,0.42871758077564,-2.61301484029198));
#16441=CARTESIAN_POINT('Ctrl Pts',(2.15727871612348,0.480878267585018,-2.61602496895319));
#16442=CARTESIAN_POINT('Ctrl Pts',(2.17539304880093,0.532946250156664,-2.6190297477676));
#16443=CARTESIAN_POINT('Ctrl Pts',(2.19648269264047,0.5840731520418,-2.62203452658202));
#16444=CARTESIAN_POINT('Ctrl Pts',(2.22042650369009,0.633898338185006,-2.62503930539644));
#16445=CARTESIAN_POINT('Ctrl Pts',(2.24434662630552,0.683674230561216,-2.62804111148003));
#16446=CARTESIAN_POINT('Ctrl Pts',(2.27111509484355,0.732150484663586,-2.63104291756362));
#16447=CARTESIAN_POINT('Ctrl Pts',(2.30056239373894,0.778985656388025,-2.63404472364721));
#16448=CARTESIAN_POINT('Ctrl Pts',(2.32999219038134,0.825792991229121,-2.63704474558178));
#16449=CARTESIAN_POINT('Ctrl Pts',(2.36209738102242,0.870960730786668,-2.64004476751635));
#16450=CARTESIAN_POINT('Ctrl Pts',(2.39666327533235,0.914173357379207,-2.64304478945092));
#16451=CARTESIAN_POINT('Ctrl Pts',(2.431222276994,0.957377367112778,-2.64604421316299));
#16452=CARTESIAN_POINT('Ctrl Pts',(2.46824067815461,0.998626625951487,-2.64904363687505));
#16453=CARTESIAN_POINT('Ctrl Pts',(2.50746276531876,1.03763773754469,-2.65204306058711));
#16454=CARTESIAN_POINT('Ctrl Pts',(2.54672091151118,1.07668471420467,-2.65504524183484));
#16455=CARTESIAN_POINT('Ctrl Pts',(2.58818641608737,1.11348905947106,-2.65804742308257));
#16456=CARTESIAN_POINT('Ctrl Pts',(2.63156691203819,1.14780449746569,-2.6610496043303));
#16457=CARTESIAN_POINT('Ctrl Pts',(2.67496715382778,1.18213555508594,-2.6640531521043));
#16458=CARTESIAN_POINT('Ctrl Pts',(2.72028369171559,1.21397514294683,-2.66705669987829));
#16459=CARTESIAN_POINT('Ctrl Pts',(2.7671939690093,1.24311955121755,-2.67006024765228));
#16460=CARTESIAN_POINT('Ctrl Pts',(2.81419278155671,1.27231896465408,-2.67306946411722));
#16461=CARTESIAN_POINT('Ctrl Pts',(2.86279087746172,1.29881278362652,-2.67607868058216));
#16462=CARTESIAN_POINT('Ctrl Pts',(2.91264086197523,1.32244318851452,-2.67908789704709));
#16463=CARTESIAN_POINT('Ctrl Pts',(2.95077814314568,1.34052141670617,-2.68139007097044));
#16464=CARTESIAN_POINT('Ctrl Pts',(2.98964760867792,1.35692467056039,-2.68369224489378));
#16465=CARTESIAN_POINT('Ctrl Pts',(3.02908735246642,1.37160188528639,-2.68599441881713));
#16466=CARTESIAN_POINT('Ctrl Pts',(3.08065543859831,1.39079257468908,-2.68900454747836));
#16467=CARTESIAN_POINT('Ctrl Pts',(3.13341564744505,1.40711133598551,-2.6920146761396));
#16468=CARTESIAN_POINT('Ctrl Pts',(3.18701684885484,1.42041347779075,-2.69502480480084));
#16469=CARTESIAN_POINT('Ctrl Pts',(3.24052278582655,1.43369197794187,-2.69802958361528));
#16470=CARTESIAN_POINT('Ctrl Pts',(3.29486624073509,1.44396437212753,-2.70103436242972));
#16471=CARTESIAN_POINT('Ctrl Pts',(3.34967897943601,1.45113507208931,-2.70403914124417));
#16472=CARTESIAN_POINT('Ctrl Pts',(3.40443749001298,1.45829867783148,-2.70704094732778));
#16473=CARTESIAN_POINT('Ctrl Pts',(3.45966384358912,1.46236659995511,-2.7100427534114));
#16474=CARTESIAN_POINT('Ctrl Pts',(3.51497944889858,1.46329424859015,-2.71304455949502));
#16475=CARTESIAN_POINT('Ctrl Pts',(3.57026217690675,1.46422134586933,-2.71604458142962));
#16476=CARTESIAN_POINT('Ctrl Pts',(3.62563352451692,1.46201186024534,-2.71904460336421));
#16477=CARTESIAN_POINT('Ctrl Pts',(3.68071193122592,1.45667320302481,-2.72204462529881));
#16478=CARTESIAN_POINT('Ctrl Pts',(3.73577935496769,1.45133561036481,-2.7250440490109));
#16479=CARTESIAN_POINT('Ctrl Pts',(3.79055342845848,1.44287013621935,-2.72804347272299));
#16480=CARTESIAN_POINT('Ctrl Pts',(3.84465707877754,1.43133610086936,-2.73104289643508));
#16481=CARTESIAN_POINT('Ctrl Pts',(3.89881046956672,1.41979146164445,-2.73404507768283));
#16482=CARTESIAN_POINT('Ctrl Pts',(3.95229168816361,1.40517273537683,-2.73704725893059));
#16483=CARTESIAN_POINT('Ctrl Pts',(4.00473472370613,1.38759022313207,-2.74004944017835));
#16484=CARTESIAN_POINT('Ctrl Pts',(4.05720163015428,1.36999970771804,-2.74305298795237));
#16485=CARTESIAN_POINT('Ctrl Pts',(4.1086289202916,1.34944291345259,-2.74605653572639));
#16486=CARTESIAN_POINT('Ctrl Pts',(4.15866973794188,1.32607868399462,-2.7490600835004));
#16487=CARTESIAN_POINT('Ctrl Pts',(4.20880499921394,1.30267035848558,-2.75206929996537));
#16488=CARTESIAN_POINT('Ctrl Pts',(4.25754809445522,1.27644426392905,-2.75507851643033));
#16489=CARTESIAN_POINT('Ctrl Pts',(4.30457703035911,1.24760512075579,-2.7580877328953));
#16490=CARTESIAN_POINT('Ctrl Pts',(4.34055609372366,1.22554199430677,-2.76038990681843));
#16491=CARTESIAN_POINT('Ctrl Pts',(4.37553238366331,1.20195044434714,-2.76269208074156));
#16492=CARTESIAN_POINT('Ctrl Pts',(4.40937466718105,1.17693816999639,-2.76499425466469));
#16493=CARTESIAN_POINT('Ctrl Pts',(4.45362398585987,1.1442342273665,-2.76800438332594));
#16494=CARTESIAN_POINT('Ctrl Pts',(4.49611935862923,1.10896263963622,-2.77101451198718));
#16495=CARTESIAN_POINT('Ctrl Pts',(4.53654774642365,1.07133842895288,-2.77402464064843));
#16496=CARTESIAN_POINT('Ctrl Pts',(4.57690428158148,1.03378108709327,-2.77702941946288));
#16497=CARTESIAN_POINT('Ctrl Pts',(4.615200738603,0.993879776922777,-2.78003419827733));
#16498=CARTESIAN_POINT('Ctrl Pts',(4.65115585805821,0.951890675398488,-2.78303897709178));
#16499=CARTESIAN_POINT('Ctrl Pts',(4.68707540587953,0.909943115133671,-2.78604078317541));
#16500=CARTESIAN_POINT('Ctrl Pts',(4.72065786293454,0.865912254389309,-2.78904258925904));
#16501=CARTESIAN_POINT('Ctrl Pts',(4.75165902322557,0.820090809809592,-2.79204439534267));
#16502=CARTESIAN_POINT('Ctrl Pts',(4.78264175771287,0.774296599595849,-2.79504441727727));
#16503=CARTESIAN_POINT('Ctrl Pts',(4.81104594100673,0.726714351495139,-2.79804443921188));
#16504=CARTESIAN_POINT('Ctrl Pts',(4.83666929711483,0.677667682206619,-2.80104446114649));
#16505=CARTESIAN_POINT('Ctrl Pts',(4.86228754377085,0.628630793120422,-2.80404388485859));
#16506=CARTESIAN_POINT('Ctrl Pts',(4.88512582007675,0.57813053059954,-2.80704330857069));
#16507=CARTESIAN_POINT('Ctrl Pts',(4.90502777720061,0.526515115731879,-2.81004273228279));
#16508=CARTESIAN_POINT('Ctrl Pts',(4.92494803129146,0.474852247966205,-2.81304491353055));
#16509=CARTESIAN_POINT('Ctrl Pts',(4.94192638250413,0.422072673409251,-2.81604709477832));
#16510=CARTESIAN_POINT('Ctrl Pts',(4.95585522405133,0.368543204077658,-2.81904927602609));
#16511=CARTESIAN_POINT('Ctrl Pts',(4.96979040569801,0.314989369319897,-2.82205282380012));
#16512=CARTESIAN_POINT('Ctrl Pts',(4.98067320670421,0.260685478081652,-2.82505637157414));
#16513=CARTESIAN_POINT('Ctrl Pts',(4.98844714205617,0.206008823297058,-2.82805991934817));
#16514=CARTESIAN_POINT('Ctrl Pts',(4.9962357494028,0.151228975528263,-2.83106913581315));
#16515=CARTESIAN_POINT('Ctrl Pts',(5.00090372528359,0.0960754863314583,
-2.83407835227812));
#16516=CARTESIAN_POINT('Ctrl Pts',(5.0024465926902,0.0409298922064158,-2.8370875687431));
#16517=CARTESIAN_POINT('Ctrl Pts',(5.00362694948791,-0.00125874734258944,
-2.83938974266614));
#16518=CARTESIAN_POINT('Ctrl Pts',(5.00297929899839,-0.0434426617668592,
-2.84169191658919));
#16519=CARTESIAN_POINT('Ctrl Pts',(5.0005221369383,-0.0854530935234426,
-2.84399409051224));
#16520=CARTESIAN_POINT('Ctrl Pts',(4.99730935884699,-0.14038239466579,-2.84700421917348));
#16521=CARTESIAN_POINT('Ctrl Pts',(4.99098775972164,-0.19524567010842,-2.85001434783471));
#16522=CARTESIAN_POINT('Ctrl Pts',(4.98156638308101,-0.249663253951969,
-2.85302447649594));
#16523=CARTESIAN_POINT('Ctrl Pts',(4.97216175088133,-0.303984122415817,
-2.85602925531038));
#16524=CARTESIAN_POINT('Ctrl Pts',(4.95966836353162,-0.357860355081316,
-2.85903403412482));
#16525=CARTESIAN_POINT('Ctrl Pts',(4.94414709707948,-0.410916415522626,
-2.86203881293926));
#16526=CARTESIAN_POINT('Ctrl Pts',(4.92864118634904,-0.463919985782113,
-2.86504061902288));
#16527=CARTESIAN_POINT('Ctrl Pts',(4.91011347817907,-0.516104486830642,
-2.86804242510649));
#16528=CARTESIAN_POINT('Ctrl Pts',(4.88867569743848,-0.56710545034758,-2.87104423119011));
#16529=CARTESIAN_POINT('Ctrl Pts',(4.86725065842551,-0.618076101007325,
-2.87404425312471));
#16530=CARTESIAN_POINT('Ctrl Pts',(4.84291917931119,-0.667864122528489,
-2.8770442750593));
#16531=CARTESIAN_POINT('Ctrl Pts',(4.81584177498237,-0.716123280429649,
-2.88004429699389));
#16532=CARTESIAN_POINT('Ctrl Pts',(4.78876977005164,-0.764372815163025,
-2.88304372070598));
#16533=CARTESIAN_POINT('Ctrl Pts',(4.75895318559949,-0.811093631411098,
-2.88604314441807));
#16534=CARTESIAN_POINT('Ctrl Pts',(4.72659823777069,-0.855964516183891,
-2.88904256813016));
#16535=CARTESIAN_POINT('Ctrl Pts',(4.69421354425364,-0.900876653236148,
-2.89204474937791));
#16536=CARTESIAN_POINT('Ctrl Pts',(4.65928613456119,-0.943935031659692,
-2.89504693062567));
#16537=CARTESIAN_POINT('Ctrl Pts',(4.6220644277031,-0.984849103228237,-2.89804911187342));
#16538=CARTESIAN_POINT('Ctrl Pts',(4.58482577835032,-1.02578179797393,-2.90105265964744));
#16539=CARTESIAN_POINT('Ctrl Pts',(4.54529112770943,-1.06456786970122,-2.90405620742145));
#16540=CARTESIAN_POINT('Ctrl Pts',(4.50374560557704,-1.1009538593128,-2.90705975519547));
#16541=CARTESIAN_POINT('Ctrl Pts',(4.46212167326346,-1.13740852135626,-2.91006897166043));
#16542=CARTESIAN_POINT('Ctrl Pts',(4.41847970541559,-1.17145372677122,-2.91307818812539));
#16543=CARTESIAN_POINT('Ctrl Pts',(4.37313680290049,-1.20287725589703,-2.91608740459035));
#16544=CARTESIAN_POINT('Ctrl Pts',(4.33844762417712,-1.22691754351648,-2.91838957851351));
#16545=CARTESIAN_POINT('Ctrl Pts',(4.30276358686709,-1.24942424404609,-2.92069175243666));
#16546=CARTESIAN_POINT('Ctrl Pts',(4.26623613594139,-1.27032063968733,-2.92299392635982));
#16547=CARTESIAN_POINT('Ctrl Pts',(4.21847591858875,-1.29764300608357,-2.92600405502105));
#16548=CARTESIAN_POINT('Ctrl Pts',(4.16907235192759,-1.32232557501314,-2.92901418368229));
#16549=CARTESIAN_POINT('Ctrl Pts',(4.11834835770971,-1.34416847270942,-2.93202431234353));
#16550=CARTESIAN_POINT('Ctrl Pts',(4.06771451432204,-1.36597254942182,-2.93502909115798));
#16551=CARTESIAN_POINT('Ctrl Pts',(4.01576538169322,-1.38494676331384,-2.93803386997242));
#16552=CARTESIAN_POINT('Ctrl Pts',(3.96284874412012,-1.40093690808483,-2.94103864878686));
#16553=CARTESIAN_POINT('Ctrl Pts',(3.90998445879302,-1.41691123325672,-2.94404045487048));
#16554=CARTESIAN_POINT('Ctrl Pts',(3.85615506771511,-1.42990718554602,-2.9470422609541));
#16555=CARTESIAN_POINT('Ctrl Pts',(3.80172686894361,-1.43981919347766,-2.95004406703772));
#16556=CARTESIAN_POINT('Ctrl Pts',(3.74733102003577,-1.44972531012294,-2.95304408897232));
#16557=CARTESIAN_POINT('Ctrl Pts',(3.6923375873977,-1.45655102104369,-2.95604411090692));
#16558=CARTESIAN_POINT('Ctrl Pts',(3.63712425642985,-1.46024158061615,-2.95904413284152));
#16559=CARTESIAN_POINT('Ctrl Pts',(3.58192193533393,-1.46393140426872,-2.96204355655361));
#16560=CARTESIAN_POINT('Ctrl Pts',(3.52650032963541,-1.46448728292818,-2.9650429802657));
#16561=CARTESIAN_POINT('Ctrl Pts',(3.47124113955017,-1.4619064186489,-2.96804240397779));
#16562=CARTESIAN_POINT('Ctrl Pts',(3.41593114664336,-1.45932318163872,-2.97104458522555));
#16563=CARTESIAN_POINT('Ctrl Pts',(3.36078439634166,-1.45359746496208,-2.97404676647331));
#16564=CARTESIAN_POINT('Ctrl Pts',(3.30617996577585,-1.44477857181508,-2.97704894772107));
#16565=CARTESIAN_POINT('Ctrl Pts',(3.25155068048537,-1.43595566450369,-2.98005249549509));
#16566=CARTESIAN_POINT('Ctrl Pts',(3.19746472365413,-1.42403688793092,-2.98305604326911));
#16567=CARTESIAN_POINT('Ctrl Pts',(3.14429016789902,-1.40912255691932,-2.98605959104313));
#16568=CARTESIAN_POINT('Ctrl Pts',(3.09101525411885,-1.39418007761793,-2.98906880750809));
#16569=CARTESIAN_POINT('Ctrl Pts',(3.0386556784167,-1.37623092160208,-2.99207802397306));
#16570=CARTESIAN_POINT('Ctrl Pts',(2.98756244313878,-1.35542471339256,-2.99508724043803));
#16571=CARTESIAN_POINT('Ctrl Pts',(2.94847402418526,-1.33950711140662,-2.99738941436114));
#16572=CARTESIAN_POINT('Ctrl Pts',(2.91012643886648,-1.32191834261422,-2.99969158828426));
#16573=CARTESIAN_POINT('Ctrl Pts',(2.87266668934103,-1.30274332795045,-3.00199376220737));
#16574=CARTESIAN_POINT('Ctrl Pts',(2.82368747688569,-1.27767169429168,-3.00500389086861));
#16575=CARTESIAN_POINT('Ctrl Pts',(2.77602124624238,-1.24978133638672,-3.00801401952985));
#16576=CARTESIAN_POINT('Ctrl Pts',(2.73001184024735,-1.21923349965199,-3.01102414819109));
#16577=CARTESIAN_POINT('Ctrl Pts',(2.68408420593083,-1.1887399550306,-3.01402892700553));
#16578=CARTESIAN_POINT('Ctrl Pts',(2.63980798900827,-1.15559859433535,-3.01703370581998));
#16579=CARTESIAN_POINT('Ctrl Pts',(2.59750236938113,-1.12001643855743,-3.02003848463442));
#16580=CARTESIAN_POINT('Ctrl Pts',(2.55523860415568,-1.08446948542763,-3.02304029071804));
#16581=CARTESIAN_POINT('Ctrl Pts',(2.51494197638256,-1.04648685900659,-3.02604209680166));
#16582=CARTESIAN_POINT('Ctrl Pts',(2.47690104883388,-1.00631765993585,-3.02904390288528));
#16583=CARTESIAN_POINT('Ctrl Pts',(2.4388827312346,-0.966172335770815,-3.03204392481988));
#16584=CARTESIAN_POINT('Ctrl Pts',(2.40311781892806,-0.923843397553574,
-3.03504394675448));
#16585=CARTESIAN_POINT('Ctrl Pts',(2.3698585286677,-0.879617254177708,-3.03804396868908));
#16586=CARTESIAN_POINT('Ctrl Pts',(2.33660587051082,-0.835399929762124,
-3.04104339240118));
#16587=CARTESIAN_POINT('Ctrl Pts',(2.30585815938332,-0.789286573348689,
-3.04404281611327));
#16588=CARTESIAN_POINT('Ctrl Pts',(2.2778262981395,-0.741595340354364,-3.04704223982537));
#16589=CARTESIAN_POINT('Ctrl Pts',(2.24976866565941,-0.693860262178921,
-3.05004442107313));
#16590=CARTESIAN_POINT('Ctrl Pts',(2.22443213959196,-0.644544865525007,
-3.05304660232089));
#16591=CARTESIAN_POINT('Ctrl Pts',(2.20198255343965,-0.593993576764533,
-3.05604878356865));
#16592=CARTESIAN_POINT('Ctrl Pts',(2.17952274873406,-0.543419278179571,
-3.05905233134267));
#16593=CARTESIAN_POINT('Ctrl Pts',(2.15995269039105,-0.491608460990556,
-3.06205587911669));
#16594=CARTESIAN_POINT('Ctrl Pts',(2.14338947547991,-0.438924207545298,
-3.06505942689071));
#16595=CARTESIAN_POINT('Ctrl Pts',(2.12679500028811,-0.386140521438059,
-3.06806864335568));
#16596=CARTESIAN_POINT('Ctrl Pts',(2.11321883489573,-0.332480619251878,
-3.07107785982064));
#16597=CARTESIAN_POINT('Ctrl Pts',(2.10272745104385,-0.278320229148988,
-3.07408707628561));
#16598=CARTESIAN_POINT('Ctrl Pts',(2.09470111242638,-0.236885311052606,
-3.07638925020872));
#16599=CARTESIAN_POINT('Ctrl Pts',(2.08847920957511,-0.195157742080637,
-3.07869142413183));
#16600=CARTESIAN_POINT('Ctrl Pts',(2.08407094032382,-0.153307040962717,
-3.08099359805493));
#16601=CARTESIAN_POINT('Ctrl Pts',(2.07874046754152,-0.102701233896012,
-3.08377738342232));
#16602=CARTESIAN_POINT('Ctrl Pts',(2.07604874230331,-0.0518126899422588,
-3.0865611687897));
#16603=CARTESIAN_POINT('Ctrl Pts',(2.07601929469992,-0.000845575841055191,
-3.08934495415708));
#16604=CARTESIAN_POINT('Origin',(3.53951905042299,8.32667268468867E-16,
0.));
#16605=CARTESIAN_POINT('',(2.07614743105272,-0.000562648890241308,-3.66065501978387));
#16606=CARTESIAN_POINT('',(2.07617134745593,-0.000497992070551351,-3.58934493090286));
#16607=CARTESIAN_POINT('',(2.07601905042299,1.01189432752408E-15,0.));
#16608=CARTESIAN_POINT('Ctrl Pts',(2.07601915861015,-0.000562728902602422,
-3.66065501812075));
#16609=CARTESIAN_POINT('Ctrl Pts',(2.07604233637565,-0.060841589897486,
-3.65739327834551));
#16610=CARTESIAN_POINT('Ctrl Pts',(2.07979389092341,-0.121006025409188,
-3.65413153857028));
#16611=CARTESIAN_POINT('Ctrl Pts',(2.08720649254477,-0.180611417770944,
-3.65086979879504));
#16612=CARTESIAN_POINT('Ctrl Pts',(2.09464146722324,-0.240396713885171,
-3.64759821428594));
#16613=CARTESIAN_POINT('Ctrl Pts',(2.10575947781169,-0.299619235945275,
-3.64432662977683));
#16614=CARTESIAN_POINT('Ctrl Pts',(2.12044242524502,-0.357846030959535,
-3.64105504526772));
#16615=CARTESIAN_POINT('Ctrl Pts',(2.13518799272812,-0.416321152464037,
-3.63776950805697));
#16616=CARTESIAN_POINT('Ctrl Pts',(2.15352880326591,-0.47379169729044,-3.63448397084622));
#16617=CARTESIAN_POINT('Ctrl Pts',(2.17529705639333,-0.529840165527046,
-3.63119843363546));
#16618=CARTESIAN_POINT('Ctrl Pts',(2.18453772564011,-0.553632858203489,
-3.62980371617767));
#16619=CARTESIAN_POINT('Ctrl Pts',(2.19439545034132,-0.577169577394221,
-3.62840899871987));
#16620=CARTESIAN_POINT('Ctrl Pts',(2.20485490604248,-0.600419746265086,
-3.62701428126207));
#16621=CARTESIAN_POINT('Ctrl Pts',(2.22742887413253,-0.650599084958731,
-3.62400415260083));
#16622=CARTESIAN_POINT('Ctrl Pts',(2.25288409438884,-0.699609016294227,
-3.62099402393959));
#16623=CARTESIAN_POINT('Ctrl Pts',(2.28107683673418,-0.747098015528093,
-3.61798389527836));
#16624=CARTESIAN_POINT('Ctrl Pts',(2.30921947263254,-0.794502613429382,
-3.61497911646391));
#16625=CARTESIAN_POINT('Ctrl Pts',(2.34008970788798,-0.840391193152254,
-3.61197433764947));
#16626=CARTESIAN_POINT('Ctrl Pts',(2.37349685323573,-0.884434557028728,
-3.60896955883502));
#16627=CARTESIAN_POINT('Ctrl Pts',(2.40687094774785,-0.928434347293463,
-3.6059677527514));
#16628=CARTESIAN_POINT('Ctrl Pts',(2.44277666286921,-0.97059211930943,-3.60296594666778));
#16629=CARTESIAN_POINT('Ctrl Pts',(2.48097974161949,-1.01060713520032,-3.59996414058416));
#16630=CARTESIAN_POINT('Ctrl Pts',(2.51916011404443,-1.0505983678256,-3.59696411864956));
#16631=CARTESIAN_POINT('Ctrl Pts',(2.55963477971373,-1.08844898739587,-3.59396409671496));
#16632=CARTESIAN_POINT('Ctrl Pts',(2.60213039085658,-1.12389267766824,-3.59096407478036));
#16633=CARTESIAN_POINT('Ctrl Pts',(2.6446175281177,-1.15932930025452,-3.58796465106826));
#16634=CARTESIAN_POINT('Ctrl Pts',(2.6891244051954,-1.1923596086406,-3.58496522735617));
#16635=CARTESIAN_POINT('Ctrl Pts',(2.73534388809484,-1.22275694980421,-3.58196580364408));
#16636=CARTESIAN_POINT('Ctrl Pts',(2.78160586311438,-1.25318223692027,-3.57896362239632));
#16637=CARTESIAN_POINT('Ctrl Pts',(2.82958314739795,-1.28096942988885,-3.57596144114856));
#16638=CARTESIAN_POINT('Ctrl Pts',(2.87894010028208,-1.30593556526757,-3.5729592599008));
#16639=CARTESIAN_POINT('Ctrl Pts',(2.92831951935554,-1.33091306467692,-3.56995571212678));
#16640=CARTESIAN_POINT('Ctrl Pts',(2.97907937402391,-1.35306673514907,-3.56695216435275));
#16641=CARTESIAN_POINT('Ctrl Pts',(3.03086293765722,-1.3722613486308,-3.56394861657873));
#16642=CARTESIAN_POINT('Ctrl Pts',(3.08274423405206,-1.39149218871514,-3.56093940011377));
#16643=CARTESIAN_POINT('Ctrl Pts',(3.13565259298671,-1.40775265993323,-3.5579301836488));
#16644=CARTESIAN_POINT('Ctrl Pts',(3.18921610930756,-1.42095745870377,-3.55492096718383));
#16645=CARTESIAN_POINT('Ctrl Pts',(3.23019439449889,-1.43105967093853,-3.55261879326072));
#16646=CARTESIAN_POINT('Ctrl Pts',(3.2715558042486,-1.43937446924751,-3.55031661933761));
#16647=CARTESIAN_POINT('Ctrl Pts',(3.31313149786576,-1.44588413299515,-3.5480144454145));
#16648=CARTESIAN_POINT('Ctrl Pts',(3.36749237204281,-1.45439562086543,-3.54500431675327));
#16649=CARTESIAN_POINT('Ctrl Pts',(3.42244814095818,-1.45985502291367,-3.54199418809203));
#16650=CARTESIAN_POINT('Ctrl Pts',(3.47762585962868,-1.46219064520783,-3.53898405943079));
#16651=CARTESIAN_POINT('Ctrl Pts',(3.53270551194573,-1.46452211644308,-3.53597928061635));
#16652=CARTESIAN_POINT('Ctrl Pts',(3.58800580781906,-1.46374080342766,-3.5329745018019));
#16653=CARTESIAN_POINT('Ctrl Pts',(3.64314684347637,-1.45982654123936,-3.52996972298746));
#16654=CARTESIAN_POINT('Ctrl Pts',(3.69823332621429,-1.45591615156501,-3.52696791690384));
#16655=CARTESIAN_POINT('Ctrl Pts',(3.75316033665749,-1.448878989957,-3.52396611082022));
#16656=CARTESIAN_POINT('Ctrl Pts',(3.80754800164634,-1.43874693094585,-3.5209643047366));
#16657=CARTESIAN_POINT('Ctrl Pts',(3.86190334086315,-1.4286208940103,-3.517964282802));
#16658=CARTESIAN_POINT('Ctrl Pts',(3.9157194518584,-1.4154037021664,-3.5149642608674));
#16659=CARTESIAN_POINT('Ctrl Pts',(3.96862393146242,-1.39917877737912,-3.5119642389328));
#16660=CARTESIAN_POINT('Ctrl Pts',(4.0215178615934,-1.38295708793992,-3.50896481522071));
#16661=CARTESIAN_POINT('Ctrl Pts',(4.0735000167278,-1.36372901141447,-3.50596539150862));
#16662=CARTESIAN_POINT('Ctrl Pts',(4.12421275205047,-1.34162793846772,-3.50296596779653));
#16663=CARTESIAN_POINT('Ctrl Pts',(4.17497211038806,-1.31950654678551,-3.49996378654877));
#16664=CARTESIAN_POINT('Ctrl Pts',(4.22445923212649,-1.29450709314462,-3.49696160530101));
#16665=CARTESIAN_POINT('Ctrl Pts',(4.27233748771777,-1.2668107151271,-3.49395942405325));
#16666=CARTESIAN_POINT('Ctrl Pts',(4.32023753642817,-1.23910173033312,-3.49095587627923));
#16667=CARTESIAN_POINT('Ctrl Pts',(4.36652681699616,-1.20869366453081,-3.48795232850521));
#16668=CARTESIAN_POINT('Ctrl Pts',(4.4108971582575,-1.1758113977959,-3.4849487807312));
#16669=CARTESIAN_POINT('Ctrl Pts',(4.45535124107075,-1.14286707131638,-3.48193956426623));
#16670=CARTESIAN_POINT('Ctrl Pts',(4.49787874295706,-1.1074395544305,-3.47893034780126));
#16671=CARTESIAN_POINT('Ctrl Pts',(4.53820501235536,-1.06979371817151,-3.4759211313363));
#16672=CARTESIAN_POINT('Ctrl Pts',(4.56905626114596,-1.04099311058529,-3.47361895741318));
#16673=CARTESIAN_POINT('Ctrl Pts',(4.59861984042386,-1.01089498991805,-3.47131678349006));
#16674=CARTESIAN_POINT('Ctrl Pts',(4.62678865478913,-0.979631082306754,
-3.46901460956694));
#16675=CARTESIAN_POINT('Ctrl Pts',(4.66361982320017,-0.938753030732151,
-3.4660044809057));
#16676=CARTESIAN_POINT('Ctrl Pts',(4.69821983574435,-0.895709091091989,
-3.46299435224446));
#16677=CARTESIAN_POINT('Ctrl Pts',(4.73032487114932,-0.850772441563712,
-3.45998422358323));
#16678=CARTESIAN_POINT('Ctrl Pts',(4.76237284686017,-0.805915657123414,
-3.45697944476878));
#16679=CARTESIAN_POINT('Ctrl Pts',(4.79193434075991,-0.759173264671589,
-3.45397466595434));
#16680=CARTESIAN_POINT('Ctrl Pts',(4.81878488625366,-0.710852425807533,
-3.4509698871399));
#16681=CARTESIAN_POINT('Ctrl Pts',(4.84560886758107,-0.66257939240805,-3.44796808105628));
#16682=CARTESIAN_POINT('Ctrl Pts',(4.86972695822759,-0.61273146543722,-3.44496627497266));
#16683=CARTESIAN_POINT('Ctrl Pts',(4.89095829276723,-0.561644215008064,
-3.44196446888904));
#16684=CARTESIAN_POINT('Ctrl Pts',(4.9121770082823,-0.510587328721452,-3.43896444695444));
#16685=CARTESIAN_POINT('Ctrl Pts',(4.93051216618611,-0.458293065675363,
-3.43596442501984));
#16686=CARTESIAN_POINT('Ctrl Pts',(4.94583015498946,-0.405118904981052,
-3.43296440308524));
#16687=CARTESIAN_POINT('Ctrl Pts',(4.96114508929324,-0.351955347535801,
-3.42996497937315));
#16688=CARTESIAN_POINT('Ctrl Pts',(4.97344390322272,-0.297912748086719,
-3.42696555566106));
#16689=CARTESIAN_POINT('Ctrl Pts',(4.98264289932671,-0.24336352792746,-3.42396613194897));
#16690=CARTESIAN_POINT('Ctrl Pts',(4.99185035257525,-0.188764157661157,
-3.42096395070121));
#16691=CARTESIAN_POINT('Ctrl Pts',(4.99795220639281,-0.133657758030206,
-3.41796176945345));
#16692=CARTESIAN_POINT('Ctrl Pts',(5.00091623531578,-0.0784252382045063,
-3.4149595882057));
#16693=CARTESIAN_POINT('Ctrl Pts',(5.00388161339891,-0.0231675777618596,
-3.41195604043168));
#16694=CARTESIAN_POINT('Ctrl Pts',(5.00370632110761,0.03221578827842,-3.40895249265766));
#16695=CARTESIAN_POINT('Ctrl Pts',(5.00041031804309,0.0873438846819063,
-3.40594894488364));
#16696=CARTESIAN_POINT('Ctrl Pts',(4.99710809432749,0.142576026089676,-3.40293972841868));
#16697=CARTESIAN_POINT('Ctrl Pts',(4.99067345556114,0.19755140961117,-3.39993051195371));
#16698=CARTESIAN_POINT('Ctrl Pts',(4.98117816982806,0.251895282679516,-3.39692129548874));
#16699=CARTESIAN_POINT('Ctrl Pts',(4.97391388709474,0.293470572764479,-3.39461912156562));
#16700=CARTESIAN_POINT('Ctrl Pts',(4.96485932466931,0.334676361031509,-3.3923169476425));
#16701=CARTESIAN_POINT('Ctrl Pts',(4.95406629023054,0.375350977556793,-3.39001477371938));
#16702=CARTESIAN_POINT('Ctrl Pts',(4.93995422772319,0.428533679244945,-3.38700464505814));
#16703=CARTESIAN_POINT('Ctrl Pts',(4.92280908086353,0.481031160584219,-3.3839945163969));
#16704=CARTESIAN_POINT('Ctrl Pts',(4.90271549281963,0.532473200675057,-3.38098438773566));
#16705=CARTESIAN_POINT('Ctrl Pts',(4.88265761674345,0.58382381376586,-3.37797960892122));
#16706=CARTESIAN_POINT('Ctrl Pts',(4.85966188930974,0.634122220236664,-3.37497483010677));
#16707=CARTESIAN_POINT('Ctrl Pts',(4.83386291895825,0.683012591381131,-3.37197005129233));
#16708=CARTESIAN_POINT('Ctrl Pts',(4.80808947241373,0.73185459360319,-3.36896824520871));
#16709=CARTESIAN_POINT('Ctrl Pts',(4.77951852207243,0.779290855221503,-3.36596643912509));
#16710=CARTESIAN_POINT('Ctrl Pts',(4.74833229277643,0.82498654238173,-3.36296463304147));
#16711=CARTESIAN_POINT('Ctrl Pts',(4.71716459928151,0.870655069920977,-3.35996461110687));
#16712=CARTESIAN_POINT('Ctrl Pts',(4.68338500489004,0.914584638159706,-3.35696458917227));
#16713=CARTESIAN_POINT('Ctrl Pts',(4.64721990318528,0.956468018696754,-3.35396456723767));
#16714=CARTESIAN_POINT('Ctrl Pts',(4.61106201302042,0.998343047434538,-3.35096514352558));
#16715=CARTESIAN_POINT('Ctrl Pts',(4.57251990518736,1.03817229928629,-3.34796571981349));
#16716=CARTESIAN_POINT('Ctrl Pts',(4.53185976058371,1.07568218585125,-3.34496629610139));
#16717=CARTESIAN_POINT('Ctrl Pts',(4.4911622348663,1.11322655732398,-3.34196411485363));
#16718=CARTESIAN_POINT('Ctrl Pts',(4.44834317107264,1.14844694454692,-3.33896193360588));
#16719=CARTESIAN_POINT('Ctrl Pts',(4.40370398301709,1.18110823055185,-3.33595975235812));
#16720=CARTESIAN_POINT('Ctrl Pts',(4.35904447619406,1.21378438324915,-3.3329562045841));
#16721=CARTESIAN_POINT('Ctrl Pts',(4.31256363758637,1.24389882502826,-3.32995265681008));
#16722=CARTESIAN_POINT('Ctrl Pts',(4.26459145005377,1.27126010921985,-3.32694910903606));
#16723=CARTESIAN_POINT('Ctrl Pts',(4.21652872309059,1.29867303323064,-3.32393989257109));
#16724=CARTESIAN_POINT('Ctrl Pts',(4.16696949848021,1.32332218383281,-3.32093067610612));
#16725=CARTESIAN_POINT('Ctrl Pts',(4.11626685538243,1.3450629053968,-3.31792145964115));
#16726=CARTESIAN_POINT('Ctrl Pts',(4.07747725545448,1.36169544839827,-3.31561928571804));
#16727=CARTESIAN_POINT('Ctrl Pts',(4.03801892144761,1.37662668963314,-3.31331711179493));
#16728=CARTESIAN_POINT('Ctrl Pts',(3.99805556378633,1.38981168361494,-3.31101493787181));
#16729=CARTESIAN_POINT('Ctrl Pts',(3.94580284426425,1.40705127089563,-3.30800480921057));
#16730=CARTESIAN_POINT('Ctrl Pts',(3.89246674984226,1.42137616669333,-3.30499468054934));
#16731=CARTESIAN_POINT('Ctrl Pts',(3.83840359918223,1.43265497469313,-3.3019845518881));
#16732=CARTESIAN_POINT('Ctrl Pts',(3.78443653397428,1.4439137370731,-3.29897977307365));
#16733=CARTESIAN_POINT('Ctrl Pts',(3.72974548967968,1.45213704830831,-3.29597499425921));
#16734=CARTESIAN_POINT('Ctrl Pts',(3.67470203193942,1.45724322318147,-3.29297021544476));
#16735=CARTESIAN_POINT('Ctrl Pts',(3.61971303058135,1.46234434634056,-3.28996840936114));
#16736=CARTESIAN_POINT('Ctrl Pts',(3.5643728297189,1.46433439363332,-3.28696660327752));
#16737=CARTESIAN_POINT('Ctrl Pts',(3.5090614286548,1.4631830313656,-3.28396479719391));
#16738=CARTESIAN_POINT('Ctrl Pts',(3.45378290239316,1.46203235341986,-3.28096477525931));
#16739=CARTESIAN_POINT('Ctrl Pts',(3.39853366894963,1.457743977644,-3.27796475332471));
#16740=CARTESIAN_POINT('Ctrl Pts',(3.3436947409438,1.4503396463646,-3.27496473139011));
#16741=CARTESIAN_POINT('Ctrl Pts',(3.28886674815168,1.44293679155362,-3.27196530767802));
#16742=CARTESIAN_POINT('Ctrl Pts',(3.23444942138508,1.43241928581962,-3.26896588396592));
#16743=CARTESIAN_POINT('Ctrl Pts',(3.18081733849026,1.41886057519988,-3.26596646025383));
#16744=CARTESIAN_POINT('Ctrl Pts',(3.12713594866328,1.40528939930957,-3.26296427900607));
#16745=CARTESIAN_POINT('Ctrl Pts',(3.07424175811424,1.38867156231255,-3.25996209775831));
#16746=CARTESIAN_POINT('Ctrl Pts',(3.02249637495661,1.36913103940185,-3.25695991651055));
#16747=CARTESIAN_POINT('Ctrl Pts',(2.97072743844921,1.34958162207888,-3.25395636873653));
#16748=CARTESIAN_POINT('Ctrl Pts',(2.92010883524168,1.32710708157945,-3.25095282096251));
#16749=CARTESIAN_POINT('Ctrl Pts',(2.87098120841114,1.30187918172084,-3.24794927318849));
#16750=CARTESIAN_POINT('Ctrl Pts',(2.82176086145281,1.27660366844695,-3.24494005672353));
#16751=CARTESIAN_POINT('Ctrl Pts',(2.7740375686657,1.2485646831774,-3.24193084025856));
#16752=CARTESIAN_POINT('Ctrl Pts',(2.72812540409954,1.21797889994283,-3.23892162379359));
#16753=CARTESIAN_POINT('Ctrl Pts',(2.69300071657754,1.19457952226413,-3.23661944987048));
#16754=CARTESIAN_POINT('Ctrl Pts',(2.65893552139658,1.16969047719012,-3.23431727594736));
#16755=CARTESIAN_POINT('Ctrl Pts',(2.62605691234446,1.14342431856989,-3.23201510202425));
#16756=CARTESIAN_POINT('Ctrl Pts',(2.5835930740428,1.1095006841884,-3.22904176635002));
#16757=CARTESIAN_POINT('Ctrl Pts',(2.54292174979811,1.07312835563625,-3.2260684306758));
#16758=CARTESIAN_POINT('Ctrl Pts',(2.50434371988584,1.0345261161746,-3.22309509500158));
#16759=CARTESIAN_POINT('Ctrl Pts',(2.46583075694527,0.995988984517273,-3.22012677425292));
#16760=CARTESIAN_POINT('Ctrl Pts',(2.42940446987904,0.955229777174039,-3.21715845350425));
#16761=CARTESIAN_POINT('Ctrl Pts',(2.39533283488617,0.912507618694519,-3.21419013275559));
#16762=CARTESIAN_POINT('Ctrl Pts',(2.36129435586734,0.869827034233313,-3.21122470055529));
#16763=CARTESIAN_POINT('Ctrl Pts',(2.32960632975867,0.825187701629692,-3.20825926835499));
#16764=CARTESIAN_POINT('Ctrl Pts',(2.30049855645537,0.778884115596297,-3.2052938361547));
#16765=CARTESIAN_POINT('Ctrl Pts',(2.27140692485811,0.732606207201201,-3.20233004843385));
#16766=CARTESIAN_POINT('Ctrl Pts',(2.24489299935041,0.684666332099463,-3.199366260713));
#16767=CARTESIAN_POINT('Ctrl Pts',(2.22114359965401,0.635388401538536,-3.19640247299214));
#16768=CARTESIAN_POINT('Ctrl Pts',(2.19727268357613,0.58585833509691,-3.19342352072971));
#16769=CARTESIAN_POINT('Ctrl Pts',(2.17619494012542,0.534976960907847,-3.19044456846727));
#16770=CARTESIAN_POINT('Ctrl Pts',(2.1580524439776,0.483096538257368,-3.18746561620484));
#16771=CARTESIAN_POINT('Ctrl Pts',(2.13998954434235,0.431443730411376,-3.18449973348968));
#16772=CARTESIAN_POINT('Ctrl Pts',(2.12483631177765,0.378801157227782,-3.18153385077452));
#16773=CARTESIAN_POINT('Ctrl Pts',(2.11268295892437,0.325531900121845,-3.17856796805937));
#16774=CARTESIAN_POINT('Ctrl Pts',(2.10044927308004,0.27191053616886,-3.17558248102329));
#16775=CARTESIAN_POINT('Ctrl Pts',(2.0912553792392,0.217654718773236,-3.17259699398722));
#16776=CARTESIAN_POINT('Ctrl Pts',(2.08514055124846,0.16314236463543,-3.16961150695114));
#16777=CARTESIAN_POINT('Ctrl Pts',(2.07902572325772,0.108630010497624,-3.16662601991506));
#16778=CARTESIAN_POINT('Ctrl Pts',(2.07598993226836,0.0538616760797857,
-3.16364053287899));
#16779=CARTESIAN_POINT('Ctrl Pts',(2.07601926119859,-0.000785455376519445,
-3.16065504584291));
#16780=CARTESIAN_POINT('Ctrl Pts',(2.07601929469955,-0.000845575214942023,
-3.08934495419128));
#16781=CARTESIAN_POINT('Ctrl Pts',(2.07598788830133,0.0535118081616528,
-3.09231391351179));
#16782=CARTESIAN_POINT('Ctrl Pts',(2.07898914341997,0.107988214496755,-3.09528287283231));
#16783=CARTESIAN_POINT('Ctrl Pts',(2.08503651530545,0.162212222221544,-3.09825183215282));
#16784=CARTESIAN_POINT('Ctrl Pts',(2.09107644060574,0.216369459835164,-3.10121713556976));
#16785=CARTESIAN_POINT('Ctrl Pts',(2.10015500184333,0.270274378399644,-3.10418243898669));
#16786=CARTESIAN_POINT('Ctrl Pts',(2.11223365853967,0.323556270402055,-3.10714774240363));
#16787=CARTESIAN_POINT('Ctrl Pts',(2.12430251114413,0.376794914170989,-3.11011063892153));
#16788=CARTESIAN_POINT('Ctrl Pts',(2.13936651916553,0.429411004753964,-3.11307353543942));
#16789=CARTESIAN_POINT('Ctrl Pts',(2.15733575241434,0.481042181836397,-3.11603643195732));
#16790=CARTESIAN_POINT('Ctrl Pts',(2.1752979395256,0.532653113181575,-3.11899816665735));
#16791=CARTESIAN_POINT('Ctrl Pts',(2.19616291584931,0.583279384128728,-3.12195990135737));
#16792=CARTESIAN_POINT('Ctrl Pts',(2.21979111334346,0.632574439960861,-3.1249216360574));
#16793=CARTESIAN_POINT('Ctrl Pts',(2.24343713421129,0.681906680356117,-3.12788560487216));
#16794=CARTESIAN_POINT('Ctrl Pts',(2.26985031141326,0.729905205751302,-3.13084957368693));
#16795=CARTESIAN_POINT('Ctrl Pts',(2.29884387362766,0.776245679977589,-3.13381354250169));
#16796=CARTESIAN_POINT('Ctrl Pts',(2.32784691981308,0.822601312455631,-3.13677848084874));
#16797=CARTESIAN_POINT('Ctrl Pts',(2.3594317215764,0.867297366745525,-3.13974341919578));
#16798=CARTESIAN_POINT('Ctrl Pts',(2.39336858699972,0.910039210800623,-3.14270835754282));
#16799=CARTESIAN_POINT('Ctrl Pts',(2.42737043916069,0.952862902515246,-3.14567897354064));
#16800=CARTESIAN_POINT('Ctrl Pts',(2.46373299244548,0.993724499544306,-3.14864958953847));
#16801=CARTESIAN_POINT('Ctrl Pts',(2.50218756820692,1.03236410534434,-3.15162020553629));
#16802=CARTESIAN_POINT('Ctrl Pts',(2.53831800319773,1.06866838741702,-3.15441128165836));
#16803=CARTESIAN_POINT('Ctrl Pts',(2.57629459257143,1.10301125847451,-3.15720235778043));
#16804=CARTESIAN_POINT('Ctrl Pts',(2.61586914384278,1.13521059723488,-3.1599934339025));
#16805=CARTESIAN_POINT('Ctrl Pts',(2.65854963187952,1.16993704260453,-3.16300356256374));
#16806=CARTESIAN_POINT('Ctrl Pts',(2.70328093322167,1.20232611928244,-3.16601369122498));
#16807=CARTESIAN_POINT('Ctrl Pts',(2.7497769339639,1.23212809378357,-3.16902381988622));
#16808=CARTESIAN_POINT('Ctrl Pts',(2.79619029821165,1.2618771017787,-3.17202859870067));
#16809=CARTESIAN_POINT('Ctrl Pts',(2.84436169668854,1.28904784969789,-3.17503337751511));
#16810=CARTESIAN_POINT('Ctrl Pts',(2.89397305648445,1.31343161973127,-3.17803815632955));
#16811=CARTESIAN_POINT('Ctrl Pts',(2.94353533405915,1.33779126606395,-3.18103996241318));
#16812=CARTESIAN_POINT('Ctrl Pts',(2.99453427924996,1.35936916469082,-3.1840417684968));
#16813=CARTESIAN_POINT('Ctrl Pts',(3.04662564177115,1.37800157391331,-3.18704357458042));
#16814=CARTESIAN_POINT('Ctrl Pts',(3.09868604334722,1.39662290880464,-3.19004359651502));
#16815=CARTESIAN_POINT('Ctrl Pts',(3.15183707905261,1.4123020467382,-3.19304361844962));
#16816=CARTESIAN_POINT('Ctrl Pts',(3.20571499639883,1.42492354304259,-3.19604364038422));
#16817=CARTESIAN_POINT('Ctrl Pts',(3.25958217016266,1.43754252254432,-3.19904306409631));
#16818=CARTESIAN_POINT('Ctrl Pts',(3.31417542380638,1.44710495089077,-3.2020424878084));
#16819=CARTESIAN_POINT('Ctrl Pts',(3.36911859454331,1.45354598641942,-3.2050419115205));
#16820=CARTESIAN_POINT('Ctrl Pts',(3.42411227756775,1.45999294354731,-3.20804409276826));
#16821=CARTESIAN_POINT('Ctrl Pts',(3.47945599474517,1.4633127130099,-3.21104627401601));
#16822=CARTESIAN_POINT('Ctrl Pts',(3.53476769754728,1.46349228718359,-3.21404845526377));
#16823=CARTESIAN_POINT('Ctrl Pts',(3.59010457700865,1.46367194309545,-3.21705200303779));
#16824=CARTESIAN_POINT('Ctrl Pts',(3.64540888476693,1.46070858272001,-3.22005555081181));
#16825=CARTESIAN_POINT('Ctrl Pts',(3.70030113358416,1.45464132064724,-3.22305909858583));
#16826=CARTESIAN_POINT('Ctrl Pts',(3.75529698228306,1.4485626076384,-3.22606831505079));
#16827=CARTESIAN_POINT('Ctrl Pts',(3.80987869642373,1.43936837842353,-3.22907753151576));
#16828=CARTESIAN_POINT('Ctrl Pts',(3.86367561185656,1.42714917709382,-3.23208674798073));
#16829=CARTESIAN_POINT('Ctrl Pts',(3.90483245693408,1.41780098729424,-3.23438892190384));
#16830=CARTESIAN_POINT('Ctrl Pts',(3.94553013665897,1.40668339077255,-3.23669109582695));
#16831=CARTESIAN_POINT('Ctrl Pts',(3.98560979439686,1.39385626882432,-3.23899326975006));
#16832=CARTESIAN_POINT('Ctrl Pts',(4.03801457810078,1.37708460486359,-3.2420033984113));
#16833=CARTESIAN_POINT('Ctrl Pts',(4.08958230895929,1.3573182004886,-3.24501352707254));
#16834=CARTESIAN_POINT('Ctrl Pts',(4.1399474969429,1.33466023039937,-3.24802365573378));
#16835=CARTESIAN_POINT('Ctrl Pts',(4.19022317179605,1.31204252990732,-3.25102843454823));
#16836=CARTESIAN_POINT('Ctrl Pts',(4.23930006744847,1.28654367725026,-3.25403321336267));
#16837=CARTESIAN_POINT('Ctrl Pts',(4.28682958332776,1.25831602445872,-3.25703799217712));
#16838=CARTESIAN_POINT('Ctrl Pts',(4.3343120766255,1.23011629825302,-3.26003979826074));
#16839=CARTESIAN_POINT('Ctrl Pts',(4.38024977090027,1.19919338822748,-3.26304160434436));
#16840=CARTESIAN_POINT('Ctrl Pts',(4.42431743106801,1.16574614543989,-3.26604341042798));
#16841=CARTESIAN_POINT('Ctrl Pts',(4.46835889924644,1.13231878230604,-3.26904343236258));
#16842=CARTESIAN_POINT('Ctrl Pts',(4.51053211649643,1.09637037886893,-3.27204345429718));
#16843=CARTESIAN_POINT('Ctrl Pts',(4.55054164186696,1.05814250911204,-3.27504347623178));
#16844=CARTESIAN_POINT('Ctrl Pts',(4.59054318909628,1.01992226222347,-3.27804289994387));
#16845=CARTESIAN_POINT('Ctrl Pts',(4.62838151966835,0.979423816342135,-3.28104232365596));
#16846=CARTESIAN_POINT('Ctrl Pts',(4.66379679307575,0.936926788695683,-3.28404174736805));
#16847=CARTESIAN_POINT('Ctrl Pts',(4.69924462569751,0.894390691187572,-3.28704392861581));
#16848=CARTESIAN_POINT('Ctrl Pts',(4.73226461177485,0.84985274759171,-3.29004610986357));
#16849=CARTESIAN_POINT('Ctrl Pts',(4.76263710725688,0.803625826518099,-3.29304829111132));
#16850=CARTESIAN_POINT('Ctrl Pts',(4.79302342762465,0.757377863976139,-3.29605183888535));
#16851=CARTESIAN_POINT('Ctrl Pts',(4.82075959021328,0.709439849350995,-3.29905538665937));
#16852=CARTESIAN_POINT('Ctrl Pts',(4.84567100420749,0.660150985476005,-3.30205893443339));
#16853=CARTESIAN_POINT('Ctrl Pts',(4.87062943430318,0.610769097165448,-3.30506815089835));
#16854=CARTESIAN_POINT('Ctrl Pts',(4.89275225423175,0.560031751868331,-3.30807736736332));
#16855=CARTESIAN_POINT('Ctrl Pts',(4.9119127676701,0.5082988637216,-3.31108658382829));
#16856=CARTESIAN_POINT('Ctrl Pts',(4.92657134571018,0.468721084108464,-3.3133887577514));
#16857=CARTESIAN_POINT('Ctrl Pts',(4.93949711185437,0.428561070948688,-3.31569093167451));
#16858=CARTESIAN_POINT('Ctrl Pts',(4.95065341965792,0.38798458985369,-3.31799310559762));
#16859=CARTESIAN_POINT('Ctrl Pts',(4.96524046781094,0.33493020178591,-3.32100323425886));
#16860=CARTESIAN_POINT('Ctrl Pts',(4.97686197788097,0.280940553597557,-3.3240133629201));
#16861=CARTESIAN_POINT('Ctrl Pts',(4.98540465913867,0.226378127275795,-3.32702349158134));
#16862=CARTESIAN_POINT('Ctrl Pts',(4.99393215764469,0.171912673759671,-3.33002827039579));
#16863=CARTESIAN_POINT('Ctrl Pts',(4.99939160542292,0.116876979854145,-3.33303304921023));
#16864=CARTESIAN_POINT('Ctrl Pts',(5.00172012741486,0.061646252471897,-3.33603782802467));
#16865=CARTESIAN_POINT('Ctrl Pts',(5.00404634572006,0.0064701667441437,
-3.33903963410829));
#16866=CARTESIAN_POINT('Ctrl Pts',(5.00324775216541,-0.0489000451757802,
-3.34204144019191));
#16867=CARTESIAN_POINT('Ctrl Pts',(4.99931318269029,-0.104083338714585,
-3.34504324627553));
#16868=CARTESIAN_POINT('Ctrl Pts',(4.99538095176005,-0.159233833592706,
-3.34804326821013));
#16869=CARTESIAN_POINT('Ctrl Pts',(4.98831647675397,-0.214197104563205,
-3.35104329014472));
#16870=CARTESIAN_POINT('Ctrl Pts',(4.97816065460882,-0.268593716802175,
-3.35404331207932));
#16871=CARTESIAN_POINT('Ctrl Pts',(4.96800685759601,-0.322979482027846,
-3.35704273579141));
#16872=CARTESIAN_POINT('Ctrl Pts',(4.95476303452417,-0.376798294070876,
-3.3600421595035));
#16873=CARTESIAN_POINT('Ctrl Pts',(4.93852139651355,-0.429679747757702,
-3.36304158321559));
#16874=CARTESIAN_POINT('Ctrl Pts',(4.92226482666919,-0.482609818281916,
-3.36604376446335));
#16875=CARTESIAN_POINT('Ctrl Pts',(4.9030050910297,-0.53460030282857,-3.36904594571111));
#16876=CARTESIAN_POINT('Ctrl Pts',(4.88088421282898,-0.585296293413464,
-3.37204812695887));
#16877=CARTESIAN_POINT('Ctrl Pts',(4.85875326569557,-0.636015359687887,
-3.37505167473289));
#16878=CARTESIAN_POINT('Ctrl Pts',(4.8337588186512,-0.685438285322511,-3.3780552225069));
#16879=CARTESIAN_POINT('Ctrl Pts',(4.80608956746164,-0.733233506714226,
-3.38105877028092));
#16880=CARTESIAN_POINT('Ctrl Pts',(4.77836809521701,-0.781118933542707,
-3.38406798674589));
#16881=CARTESIAN_POINT('Ctrl Pts',(4.747962025003,-0.82737007691808,-3.38707720321085));
#16882=CARTESIAN_POINT('Ctrl Pts',(4.71510356822208,-0.871684169588439,
-3.39008641967582));
#16883=CARTESIAN_POINT('Ctrl Pts',(4.68996550213884,-0.905586266616097,
-3.39238859359894));
#16884=CARTESIAN_POINT('Ctrl Pts',(4.66339299817311,-0.938355217170147,
-3.39469076752206));
#16885=CARTESIAN_POINT('Ctrl Pts',(4.63550486601212,-0.969869755187481,
-3.39699294144519));
#16886=CARTESIAN_POINT('Ctrl Pts',(4.59904069400365,-1.0110755099651,-3.40000307010642));
#16887=CARTESIAN_POINT('Ctrl Pts',(4.56017285810662,-1.05030856924529,-3.40301319876766));
#16888=CARTESIAN_POINT('Ctrl Pts',(4.51914304513095,-1.08727599025842,-3.40602332742889));
#16889=CARTESIAN_POINT('Ctrl Pts',(4.47818615369389,-1.12417770974811,-3.40902810624334));
#16890=CARTESIAN_POINT('Ctrl Pts',(4.43507529971017,-1.15882143129324,-3.41203288505778));
#16891=CARTESIAN_POINT('Ctrl Pts',(4.39009037438196,-1.190949483756,-3.41503766387222));
#16892=CARTESIAN_POINT('Ctrl Pts',(4.3451499541845,-1.22304575083365,-3.41803946995584));
#16893=CARTESIAN_POINT('Ctrl Pts',(4.29833956314318,-1.25263097367015,-3.42104127603946));
#16894=CARTESIAN_POINT('Ctrl Pts',(4.24997223634424,-1.27948760080524,-3.42404308212308));
#16895=CARTESIAN_POINT('Ctrl Pts',(4.20163365707812,-1.30632826547515,-3.42704310405768));
#16896=CARTESIAN_POINT('Ctrl Pts',(4.15174043700631,-1.33044329302549,-3.43004312599228));
#16897=CARTESIAN_POINT('Ctrl Pts',(4.10063270893127,-1.35165961404322,-3.43304314792688));
#16898=CARTESIAN_POINT('Ctrl Pts',(4.04953517204602,-1.37287170439833,-3.43604257163897));
#16899=CARTESIAN_POINT('Ctrl Pts',(3.9972240956012,-1.39118603377396,-3.43904199535107));
#16900=CARTESIAN_POINT('Ctrl Pts',(3.94406008769248,-1.40647744353222,-3.44204141906316));
#16901=CARTESIAN_POINT('Ctrl Pts',(3.89084720317884,-1.42178291152692,-3.44504360031092));
#16902=CARTESIAN_POINT('Ctrl Pts',(3.83678032920723,-1.4340597612545,-3.44804578155868));
#16903=CARTESIAN_POINT('Ctrl Pts',(3.78223431170352,-1.44323302066628,-3.45104796280644));
#16904=CARTESIAN_POINT('Ctrl Pts',(3.72766346606344,-1.45241045554212,-3.45405151058046));
#16905=CARTESIAN_POINT('Ctrl Pts',(3.67261356798181,-1.45848142601991,-3.45705505835448));
#16906=CARTESIAN_POINT('Ctrl Pts',(3.61746541352522,-1.46142280483067,-3.4600586061285));
#16907=CARTESIAN_POINT('Ctrl Pts',(3.56221317620818,-1.46436973499892,-3.46306782259346));
#16908=CARTESIAN_POINT('Ctrl Pts',(3.5068628414747,-1.46417527605418,-3.46607703905843));
#16909=CARTESIAN_POINT('Ctrl Pts',(3.45179486444536,-1.46086848045762,-3.46908625552339));
#16910=CARTESIAN_POINT('Ctrl Pts',(3.40966560515415,-1.45833864630307,-3.47138842944651));
#16911=CARTESIAN_POINT('Ctrl Pts',(3.36770161530294,-1.45398828503212,-3.47369060336963));
#16912=CARTESIAN_POINT('Ctrl Pts',(3.32606937562991,-1.44785064365449,-3.47599277729275));
#16913=CARTESIAN_POINT('Ctrl Pts',(3.27163456659456,-1.43982558089202,-3.47900290595399));
#16914=CARTESIAN_POINT('Ctrl Pts',(3.21753859061648,-1.42870951185746,-3.48201303461522));
#16915=CARTESIAN_POINT('Ctrl Pts',(3.16415885187338,-1.41454479297928,-3.48502316327646));
#16916=CARTESIAN_POINT('Ctrl Pts',(3.11087398396675,-1.40040524879772,-3.48802794209091));
#16917=CARTESIAN_POINT('Ctrl Pts',(3.05830333342818,-1.38322794180099,-3.49103272090535));
#16918=CARTESIAN_POINT('Ctrl Pts',(3.00681563822438,-1.36310649790541,-3.4940374997198));
#16919=CARTESIAN_POINT('Ctrl Pts',(2.95537888156484,-1.34300496084498,-3.49703930580342));
#16920=CARTESIAN_POINT('Ctrl Pts',(2.90502344730855,-1.31996524816041,-3.50004111188704));
#16921=CARTESIAN_POINT('Ctrl Pts',(2.85610258180067,-1.2941306658973,-3.50304291797066));
#16922=CARTESIAN_POINT('Ctrl Pts',(2.80721079282602,-1.26831143863827,-3.50604293990526));
#16923=CARTESIAN_POINT('Ctrl Pts',(2.75975234866062,-1.2397008804422,-3.50904296183986));
#16924=CARTESIAN_POINT('Ctrl Pts',(2.71405804682371,-1.20848929723721,-3.51204298377445));
#16925=CARTESIAN_POINT('Ctrl Pts',(2.66837285670687,-1.17728393781061,-3.51504240748654));
#16926=CARTESIAN_POINT('Ctrl Pts',(2.62445154614612,-1.14347888111928,-3.51804183119863));
#16927=CARTESIAN_POINT('Ctrl Pts',(2.58259597371697,-1.10730775995993,-3.52104125491072));
#16928=CARTESIAN_POINT('Ctrl Pts',(2.54070192115126,-1.07110338469365,-3.52404343615847));
#16929=CARTESIAN_POINT('Ctrl Pts',(2.50087780140589,-1.03252894514098,-3.52704561740623));
#16930=CARTESIAN_POINT('Ctrl Pts',(2.46339121993172,-0.991857420419962,
-3.53004779865399));
#16931=CARTESIAN_POINT('Ctrl Pts',(2.42588757539782,-0.95116738292376,-3.53305134642801));
#16932=CARTESIAN_POINT('Ctrl Pts',(2.39072392602788,-0.908378766162718,
-3.53605489420202));
#16933=CARTESIAN_POINT('Ctrl Pts',(2.35812770700803,-0.863797860442005,
-3.53905844197604));
#16934=CARTESIAN_POINT('Ctrl Pts',(2.32546996811047,-0.819132815764377,
-3.54206765844101));
#16935=CARTESIAN_POINT('Ctrl Pts',(2.2953896270958,-0.772669169180946,-3.54507687490597));
#16936=CARTESIAN_POINT('Ctrl Pts',(2.26807023093027,-0.724741436245074,
-3.54808609137094));
#16937=CARTESIAN_POINT('Ctrl Pts',(2.24716977322639,-0.688074756315559,
-3.55038826529406));
#16938=CARTESIAN_POINT('Ctrl Pts',(2.22788435855148,-0.650551765120204,
-3.55269043921719));
#16939=CARTESIAN_POINT('Ctrl Pts',(2.21027710606191,-0.612330060793335,
-3.55499261314031));
#16940=CARTESIAN_POINT('Ctrl Pts',(2.18529599781639,-0.558101240386331,
-3.5582589294499));
#16941=CARTESIAN_POINT('Ctrl Pts',(2.16360293385677,-0.50226721692865,-3.56152524575948));
#16942=CARTESIAN_POINT('Ctrl Pts',(2.14538703089759,-0.445228213542251,
-3.56479156206906));
#16943=CARTESIAN_POINT('Ctrl Pts',(2.1272219106246,-0.388348224716697,-3.56804877247176));
#16944=CARTESIAN_POINT('Ctrl Pts',(2.11251478421498,-0.330270296838304,
-3.57130598287446));
#16945=CARTESIAN_POINT('Ctrl Pts',(2.10140693884337,-0.271414451582842,
-3.57456319327716));
#16946=CARTESIAN_POINT('Ctrl Pts',(2.09034632600109,-0.21280887182384,-3.57780655344332));
#16947=CARTESIAN_POINT('Ctrl Pts',(2.08285459652992,-0.153432331059518,
-3.58104991360948));
#16948=CARTESIAN_POINT('Ctrl Pts',(2.07902279640965,-0.093717351717778,
-3.58429327377564));
#16949=CARTESIAN_POINT('Ctrl Pts',(2.07703340549742,-0.0627145766519451,
-3.58597715890459));
#16950=CARTESIAN_POINT('Ctrl Pts',(2.07602972725318,-0.0316208373297955,
-3.58766104403353));
#16951=CARTESIAN_POINT('Ctrl Pts',(2.07601913517861,-0.000498075992148151,
-3.58934492916248));
#16952=CARTESIAN_POINT('Origin',(3.53951905042299,8.32667268468867E-16,
0.));
#16953=CARTESIAN_POINT('',(2.076195135922,0.00130430976331031,-4.16065504584291));
#16954=CARTESIAN_POINT('',(2.07606592154595,0.00130399798662343,-4.08934495415709));
#16955=CARTESIAN_POINT('',(2.07601905042299,1.01189432752408E-15,0.));
#16956=CARTESIAN_POINT('Ctrl Pts',(2.076195135922,0.00130430976331031,-4.16065504584291));
#16957=CARTESIAN_POINT('Ctrl Pts',(2.07946608474589,-0.364321824825649,
-4.14077446267775));
#16958=CARTESIAN_POINT('Ctrl Pts',(2.40262791122405,-1.21940508752796,-4.09456060089675));
#16959=CARTESIAN_POINT('Ctrl Pts',(3.83411705959719,-1.70165509770555,-4.02201346049987));
#16960=CARTESIAN_POINT('Ctrl Pts',(5.12566818702416,-0.683043904164373,
-3.94301362465232));
#16961=CARTESIAN_POINT('Ctrl Pts',(4.97825236450885,0.955230081967798,-3.86401378880474));
#16962=CARTESIAN_POINT('Ctrl Pts',(3.52560638363233,1.72691183801013,-3.78501395295721));
#16963=CARTESIAN_POINT('Ctrl Pts',(2.2899855395789,1.0447694976777,-3.71722770530323));
#16964=CARTESIAN_POINT('Ctrl Pts',(2.07912945035243,0.278451525816697,-3.67577473626515));
#16965=CARTESIAN_POINT('Ctrl Pts',(2.07815730775203,-0.000561395191652214,
-3.66065504584291));
#16966=CARTESIAN_POINT('Ctrl Pts',(2.07820514495938,-0.000496870744879993,
-3.58934495415708));
#16967=CARTESIAN_POINT('Ctrl Pts',(2.07905042986027,0.274161491287648,-3.60422745243401));
#16968=CARTESIAN_POINT('Ctrl Pts',(2.28499543959671,1.0359800857574,-3.64544322932679));
#16969=CARTESIAN_POINT('Ctrl Pts',(3.51016521557272,1.7267183779139,-3.71299228483544));
#16970=CARTESIAN_POINT('Ctrl Pts',(4.96965334285999,0.968056769947792,-3.79199212068301));
#16971=CARTESIAN_POINT('Ctrl Pts',(5.13171241173874,-0.668833540148877,
-3.87099195653056));
#16972=CARTESIAN_POINT('Ctrl Pts',(3.84932116255957,-1.6989528114582,-3.94999179237812));
#16973=CARTESIAN_POINT('Ctrl Pts',(2.40888291571603,-1.22798739644682,-4.0227761249203));
#16974=CARTESIAN_POINT('Ctrl Pts',(2.07940194346651,-0.368600809769743,
-4.06922717884662));
#16975=CARTESIAN_POINT('Ctrl Pts',(2.07606592154595,0.00130399798662343,
-4.08934495415709));
#16976=CARTESIAN_POINT('Origin',(3.53951905042299,8.32667268468867E-16,
0.));
#16977=CARTESIAN_POINT('',(2.07409469887417,-0.000697191783334949,-4.66065504584291));
#16978=CARTESIAN_POINT('',(2.07601924802061,-0.000760505223226088,-4.58934495415708));
#16979=CARTESIAN_POINT('',(2.07601905042299,1.01189432752408E-15,0.));
#16980=CARTESIAN_POINT('Ctrl Pts',(2.07409469887417,-0.000697191783334949,
-4.66065504584291));
#16981=CARTESIAN_POINT('Ctrl Pts',(2.07385459663328,-0.0412693483006937,
-4.65844074632206));
#16982=CARTESIAN_POINT('Ctrl Pts',(2.09371445821182,-0.564102276336072,
-4.62989316818539));
#16983=CARTESIAN_POINT('Ctrl Pts',(2.71979604533931,-1.52002376741039,-4.57501231143279));
#16984=CARTESIAN_POINT('Ctrl Pts',(4.36468643187272,-1.51707509739907,-4.49601247558526));
#16985=CARTESIAN_POINT('Ctrl Pts',(5.26097849137829,-0.13782398812516,-4.41701263973768));
#16986=CARTESIAN_POINT('Ctrl Pts',(4.59554903047943,1.36646212526309,-4.33801280389013));
#16987=CARTESIAN_POINT('Ctrl Pts',(2.97208088054184,1.63108307020786,-4.25901296804256));
#16988=CARTESIAN_POINT('Ctrl Pts',(2.1424012204092,0.721759407375466,-4.19989371536015));
#16989=CARTESIAN_POINT('Ctrl Pts',(2.07513347508338,0.119976587921299,-4.1671077412936));
#16990=CARTESIAN_POINT('Ctrl Pts',(2.076195135922,0.00130430976331031,-4.16065504584291));
#16991=CARTESIAN_POINT('Ctrl Pts',(2.07606592154595,0.00130399798662343,
-4.08934495415709));
#16992=CARTESIAN_POINT('Ctrl Pts',(2.0750352382346,0.11558823268988,-4.09556045746248));
#16993=CARTESIAN_POINT('Ctrl Pts',(2.13929924925922,0.712915691466917,-4.12810923938368));
#16994=CARTESIAN_POINT('Ctrl Pts',(2.95751872983224,1.62594392002861,-4.18699129992084));
#16995=CARTESIAN_POINT('Ctrl Pts',(4.5832881519124,1.37585030690918,-4.26599113576836));
#16996=CARTESIAN_POINT('Ctrl Pts',(5.26214205025278,-0.122425506752148,
-4.34499097161594));
#16997=CARTESIAN_POINT('Ctrl Pts',(4.37821883844248,-1.50963593949734,-4.4239908074635));
#16998=CARTESIAN_POINT('Ctrl Pts',(2.73342059411813,-1.52729279543541,-4.50299064331106));
#16999=CARTESIAN_POINT('Ctrl Pts',(2.09607364483251,-0.572900753676928,
-4.55810869220892));
#17000=CARTESIAN_POINT('Ctrl Pts',(2.07389563130326,-0.0456866571895436,
-4.58689346249093));
#17001=CARTESIAN_POINT('Ctrl Pts',(2.07418131521338,-0.00076146030193382,
-4.58934495415708));
#17002=CARTESIAN_POINT('Origin',(3.53951905042299,8.32667268468867E-16,
0.));
#17003=CARTESIAN_POINT('',(2.07610901343792,-0.000650317076287153,-5.16065502546599));
#17004=CARTESIAN_POINT('',(2.07601916841636,-0.000587678975572513,-5.08934495412951));
#17005=CARTESIAN_POINT('',(2.07601905042299,1.01189432752408E-15,0.));
#17006=CARTESIAN_POINT('Ctrl Pts',(2.07808044699004,-0.000657693853875153,
-5.16065457821226));
#17007=CARTESIAN_POINT('Ctrl Pts',(2.0772701732856,-0.201427577003968,-5.14977343959675));
#17008=CARTESIAN_POINT('Ctrl Pts',(2.20916534632738,-0.887056648995822,
-5.11255902236538));
#17009=CARTESIAN_POINT('Ctrl Pts',(3.25102377061198,-1.70270036473932,-5.0490113265182));
#17010=CARTESIAN_POINT('Ctrl Pts',(4.80794374219368,-1.17197135624689,-4.97001149067062));
#17011=CARTESIAN_POINT('Ctrl Pts',(5.21413887471018,0.421979268046491,-4.89101165482307));
#17012=CARTESIAN_POINT('Ctrl Pts',(4.10110575481217,1.63310698731284,-4.81201181897551));
#17013=CARTESIAN_POINT('Ctrl Pts',(2.52407434145005,1.37024742679016,-4.73522628264877));
#17014=CARTESIAN_POINT('Ctrl Pts',(2.0767099823415,0.441229921360335,-4.68477402493792));
#17015=CARTESIAN_POINT('Ctrl Pts',(2.07409469887417,-0.000697191783334949,
-4.66065504584291));
#17016=CARTESIAN_POINT('Ctrl Pts',(2.07601924802061,-0.000760505223226088,
-4.58934495415708));
#17017=CARTESIAN_POINT('Ctrl Pts',(2.07599085580295,0.0538768643349187,
-4.59233017752579));
#17018=CARTESIAN_POINT('Ctrl Pts',(2.07902648452409,0.108635686348704,-4.59531540089451));
#17019=CARTESIAN_POINT('Ctrl Pts',(2.08514018297494,0.163139081524142,-4.59830062426322));
#17020=CARTESIAN_POINT('Ctrl Pts',(2.09121901100316,0.217331608173781,-4.60126882094975));
#17021=CARTESIAN_POINT('Ctrl Pts',(2.10034087561815,0.271271068644694,-4.60423701763627));
#17022=CARTESIAN_POINT('Ctrl Pts',(2.11246753287747,0.324586223168858,-4.6072052143228));
#17023=CARTESIAN_POINT('Ctrl Pts',(2.12458396202739,0.377856409552088,-4.61017090751312));
#17024=CARTESIAN_POINT('Ctrl Pts',(2.13970004715109,0.430502805880079,-4.61313660070344));
#17025=CARTESIAN_POINT('Ctrl Pts',(2.15772614502274,0.482162437966234,-4.61610229389376));
#17026=CARTESIAN_POINT('Ctrl Pts',(2.17574457529192,0.533800096049706,-4.6190667255933));
#17027=CARTESIAN_POINT('Ctrl Pts',(2.19667038709155,0.584451310505765,-4.62203115729283));
#17028=CARTESIAN_POINT('Ctrl Pts',(2.22036427111649,0.633768820811523,-4.62499558899236));
#17029=CARTESIAN_POINT('Ctrl Pts',(2.24433892995291,0.683670748372119,-4.62799514949351));
#17030=CARTESIAN_POINT('Ctrl Pts',(2.27114750041236,0.732206621938655,-4.63099470999467));
#17031=CARTESIAN_POINT('Ctrl Pts',(2.3005968689088,0.77904048556677,-4.63399427049582));
#17032=CARTESIAN_POINT('Ctrl Pts',(2.32973135258981,0.825373582174859,-4.63696175845678));
#17033=CARTESIAN_POINT('Ctrl Pts',(2.36145006211764,0.870040477621746,-4.63992924641774));
#17034=CARTESIAN_POINT('Ctrl Pts',(2.39552297687357,0.912745985312182,-4.6428967343787));
#17035=CARTESIAN_POINT('Ctrl Pts',(2.43014828052323,0.956143833188909,-4.64591233114995));
#17036=CARTESIAN_POINT('Ctrl Pts',(2.46720443639282,0.997515679329537,-4.6489279279212));
#17037=CARTESIAN_POINT('Ctrl Pts',(2.506410426729,1.0365899968884,-4.65194352469245));
#17038=CARTESIAN_POINT('Ctrl Pts',(2.54561641706517,1.07566431444727,-4.65495912146369));
#17039=CARTESIAN_POINT('Ctrl Pts',(2.58697176139739,1.11244077224011,-4.65797471823494));
#17040=CARTESIAN_POINT('Ctrl Pts',(2.63016222976418,1.14669194761336,-4.66099031500619));
#17041=CARTESIAN_POINT('Ctrl Pts',(2.67327438188038,1.1808810161437,-4.66400044366743));
#17042=CARTESIAN_POINT('Ctrl Pts',(2.71840790652042,1.21270720915157,-4.66701057232867));
#17043=CARTESIAN_POINT('Ctrl Pts',(2.76527358385478,1.24192439685295,-4.67002070098991));
#17044=CARTESIAN_POINT('Ctrl Pts',(2.81205596767518,1.27108965737926,-4.67302547980435));
#17045=CARTESIAN_POINT('Ctrl Pts',(2.8605639503056,1.29765483749972,-4.6760302586188));
#17046=CARTESIAN_POINT('Ctrl Pts',(2.91047686921657,1.32141522023286,-4.67903503743324));
#17047=CARTESIAN_POINT('Ctrl Pts',(2.96034040756352,1.34515209600376,-4.68203684351686));
#17048=CARTESIAN_POINT('Ctrl Pts',(3.01160565426423,1.36608944541669,-4.68503864960048));
#17049=CARTESIAN_POINT('Ctrl Pts',(3.06392633487658,1.38406785199252,-4.6880404556841));
#17050=CARTESIAN_POINT('Ctrl Pts',(3.11621591824668,1.40203557294925,-4.6910404776187));
#17051=CARTESIAN_POINT('Ctrl Pts',(3.16955919371126,1.41704766559505,-4.6940404995533));
#17052=CARTESIAN_POINT('Ctrl Pts',(3.22359099116527,1.42899325098954,-4.6970405214879));
#17053=CARTESIAN_POINT('Ctrl Pts',(3.27761201435219,1.44093645436208,-4.70003994519999));
#17054=CARTESIAN_POINT('Ctrl Pts',(3.33232077149073,1.4498142509152,-4.70303936891208));
#17055=CARTESIAN_POINT('Ctrl Pts',(3.38734031704768,1.45556651620882,-4.70603879262417));
#17056=CARTESIAN_POINT('Ctrl Pts',(3.44241044510778,1.46132406987723,-4.70904097387193));
#17057=CARTESIAN_POINT('Ctrl Pts',(3.4977914060457,1.46395029642692,-4.71204315511969));
#17058=CARTESIAN_POINT('Ctrl Pts',(3.55310101836569,1.46343697511946,-4.71504533636744));
#17059=CARTESIAN_POINT('Ctrl Pts',(3.60843580639342,1.46292342015954,-4.71804888414146));
#17060=CARTESIAN_POINT('Ctrl Pts',(3.66369865318093,1.45926750354695,-4.72105243191548));
#17061=CARTESIAN_POINT('Ctrl Pts',(3.71851059124897,1.45251309058223,-4.7240559796895));
#17062=CARTESIAN_POINT('Ctrl Pts',(3.77342597762567,1.44574592979976,-4.72706519615447));
#17063=CARTESIAN_POINT('Ctrl Pts',(3.82788823433538,1.4358686850687,-4.73007441261943));
#17064=CARTESIAN_POINT('Ctrl Pts',(3.88152786054452,1.42297653662991,-4.7330836290844));
#17065=CARTESIAN_POINT('Ctrl Pts',(3.92256437291978,1.41311351471232,-4.73538580300752));
#17066=CARTESIAN_POINT('Ctrl Pts',(3.96311959087821,1.40148697680282,-4.73768797693064));
#17067=CARTESIAN_POINT('Ctrl Pts',(4.00303542037397,1.38815878947168,-4.73999015085375));
#17068=CARTESIAN_POINT('Ctrl Pts',(4.05522599607103,1.37073197463159,-4.74300027951499));
#17069=CARTESIAN_POINT('Ctrl Pts',(4.10654206993801,1.35032113999199,-4.74601040817623));
#17070=CARTESIAN_POINT('Ctrl Pts',(4.15661947307721,1.32703403059604,-4.74902053683747));
#17071=CARTESIAN_POINT('Ctrl Pts',(4.20660787456074,1.3037883089551,-4.75202531565191));
#17072=CARTESIAN_POINT('Ctrl Pts',(4.25536149914432,1.27767667814298,-4.75503009446636));
#17073=CARTESIAN_POINT('Ctrl Pts',(4.30253368209914,1.24885584510307,-4.7580348732808));
#17074=CARTESIAN_POINT('Ctrl Pts',(4.3496591959941,1.22006352550261,-4.76103667936442));
#17075=CARTESIAN_POINT('Ctrl Pts',(4.39520591916271,1.18856758721965,-4.76403848544803));
#17076=CARTESIAN_POINT('Ctrl Pts',(4.43885113301751,1.15457093988035,-4.76704029153165));
#17077=CARTESIAN_POINT('Ctrl Pts',(4.48247040596762,1.12059449873803,-4.77004031346625));
#17078=CARTESIAN_POINT('Ctrl Pts',(4.52418999388672,1.0841206184022,-4.77304033540085));
#17079=CARTESIAN_POINT('Ctrl Pts',(4.56371750516629,1.04539455484589,-4.77604035733545));
#17080=CARTESIAN_POINT('Ctrl Pts',(4.60323713442113,1.00667621350079,-4.77903978104754));
#17081=CARTESIAN_POINT('Ctrl Pts',(4.64056517809698,0.965706950209743,-4.78203920475962));
#17082=CARTESIAN_POINT('Ctrl Pts',(4.67544531879757,0.922769615243488,-4.78503862847171));
#17083=CARTESIAN_POINT('Ctrl Pts',(4.71035752673553,0.879792805616716,-4.78804080971947));
#17084=CARTESIAN_POINT('Ctrl Pts',(4.74281700180259,0.834844720244073,-4.79104299096723));
#17085=CARTESIAN_POINT('Ctrl Pts',(4.77260803644009,0.788240954634642,-4.79404517221498));
#17086=CARTESIAN_POINT('Ctrl Pts',(4.80241263129523,0.741615976025646,-4.797048719989));
#17087=CARTESIAN_POINT('Ctrl Pts',(4.82954610528484,0.69333427607016,-4.80005226776302));
#17088=CARTESIAN_POINT('Ctrl Pts',(4.85383813043568,0.643737218059205,-4.80305581553704));
#17089=CARTESIAN_POINT('Ctrl Pts',(4.87817600269582,0.594046553948078,-4.806065032002));
#17090=CARTESIAN_POINT('Ctrl Pts',(4.89966150767629,0.543036060467595,-4.80907424846697));
#17091=CARTESIAN_POINT('Ctrl Pts',(4.91817246758545,0.491067210620182,-4.81208346493193));
#17092=CARTESIAN_POINT('Ctrl Pts',(4.93233411055499,0.451308910635268,-4.81438563885506));
#17093=CARTESIAN_POINT('Ctrl Pts',(4.94475578403992,0.410990129462399,-4.81668781277819));
#17094=CARTESIAN_POINT('Ctrl Pts',(4.9554029209918,0.37027707877086,-4.81898998670131));
#17095=CARTESIAN_POINT('Ctrl Pts',(4.96932422023727,0.317044123805193,-4.82200011536255));
#17096=CARTESIAN_POINT('Ctrl Pts',(4.9802684982249,0.26291313095329,-4.82501024402378));
#17097=CARTESIAN_POINT('Ctrl Pts',(4.98812701387199,0.208247972936449,-4.82802037268502));
#17098=CARTESIAN_POINT('Ctrl Pts',(4.99597156272249,0.15367997030835,-4.83102515149947));
#17099=CARTESIAN_POINT('Ctrl Pts',(5.00074115826121,0.0985802050447489,
-4.83402993031391));
#17100=CARTESIAN_POINT('Ctrl Pts',(5.00237763052374,0.0433246422444861,
-4.83703470912836));
#17101=CARTESIAN_POINT('Ctrl Pts',(5.00401248376809,-0.0118762543307643,
-4.84003651521198));
#17102=CARTESIAN_POINT('Ctrl Pts',(5.00252033854837,-0.0672321178175497,
-4.8430383212956));
#17103=CARTESIAN_POINT('Ctrl Pts',(4.99789480496805,-0.122361793690387,
-4.84604012737922));
#17104=CARTESIAN_POINT('Ctrl Pts',(4.99327202061302,-0.177458702770685,
-4.84904014931382));
#17105=CARTESIAN_POINT('Ctrl Pts',(4.98551958327649,-0.232329165482758,
-4.85204017124842));
#17106=CARTESIAN_POINT('Ctrl Pts',(4.97468313980935,-0.286594289084472,
-4.85504019318302));
#17107=CARTESIAN_POINT('Ctrl Pts',(4.96384885719453,-0.340848591892532,
-4.85803961689511));
#17108=CARTESIAN_POINT('Ctrl Pts',(4.94993189311401,-0.394497277711197,
-4.8610390406072));
#17109=CARTESIAN_POINT('Ctrl Pts',(4.93302909146274,-0.447171125545251,
-4.86403846431929));
#17110=CARTESIAN_POINT('Ctrl Pts',(4.91611075013354,-0.499893399353124,
-4.86704064556705));
#17111=CARTESIAN_POINT('Ctrl Pts',(4.89620124870217,-0.551638540700445,
-4.87004282681481));
#17112=CARTESIAN_POINT('Ctrl Pts',(4.87344704513782,-0.602053448554247,
-4.87304500806257));
#17113=CARTESIAN_POINT('Ctrl Pts',(4.85068248436513,-0.652491304154955,
-4.87604855583659));
#17114=CARTESIAN_POINT('Ctrl Pts',(4.82507088492237,-0.701597250183144,
-4.87905210361061));
#17115=CARTESIAN_POINT('Ctrl Pts',(4.79680508121693,-0.749042112815041,
-4.88205565138463));
#17116=CARTESIAN_POINT('Ctrl Pts',(4.76848593056393,-0.796576519640517,
-4.88506486784959));
#17117=CARTESIAN_POINT('Ctrl Pts',(4.7375028650093,-0.84244314168997,-4.88807408431456));
#17118=CARTESIAN_POINT('Ctrl Pts',(4.70409187045511,-0.88634214434519,-4.89108330077953));
#17119=CARTESIAN_POINT('Ctrl Pts',(4.67853109033062,-0.919926680499441,
-4.89338547470264));
#17120=CARTESIAN_POINT('Ctrl Pts',(4.6515501796311,-0.952360190103516,-4.89568764862576));
#17121=CARTESIAN_POINT('Ctrl Pts',(4.62326945780324,-0.983522904920442,
-4.89798982254888));
#17122=CARTESIAN_POINT('Ctrl Pts',(4.58629196862232,-1.02426864532286,-4.90099995121011));
#17123=CARTESIAN_POINT('Ctrl Pts',(4.54693571581419,-1.06301173467712,-4.90401007987136));
#17124=CARTESIAN_POINT('Ctrl Pts',(4.5054460368751,-1.09946228077344,-4.90702020853259));
#17125=CARTESIAN_POINT('Ctrl Pts',(4.46403009678604,-1.13584804397867,-4.91002498734704));
#17126=CARTESIAN_POINT('Ctrl Pts',(4.42048864875999,-1.16994900404581,-4.91302976616148));
#17127=CARTESIAN_POINT('Ctrl Pts',(4.37510478984533,-1.20151101621001,-4.91603454497593));
#17128=CARTESIAN_POINT('Ctrl Pts',(4.32976583074014,-1.23304180299219,-4.91903635105955));
#17129=CARTESIAN_POINT('Ctrl Pts',(4.28258850299054,-1.26203831771611,-4.92203815714317));
#17130=CARTESIAN_POINT('Ctrl Pts',(4.23388854235524,-1.288286947335,-4.92503996322679));
#17131=CARTESIAN_POINT('Ctrl Pts',(4.18521752695648,-1.31451997585724,-4.92803998516139));
#17132=CARTESIAN_POINT('Ctrl Pts',(4.13502613638216,-1.33800810637266,-4.93104000709599));
#17133=CARTESIAN_POINT('Ctrl Pts',(4.08365664476106,-1.35858254384045,-4.93404002903059));
#17134=CARTESIAN_POINT('Ctrl Pts',(4.03229739652721,-1.37915287864099,-4.93703945274267));
#17135=CARTESIAN_POINT('Ctrl Pts',(3.97976100376948,-1.39681047800443,-4.94003887645476));
#17136=CARTESIAN_POINT('Ctrl Pts',(3.9264096141322,-1.41143471039675,-4.94303830016684));
#17137=CARTESIAN_POINT('Ctrl Pts',(3.87300917561944,-1.42607238765262,-4.9460404814146));
#17138=CARTESIAN_POINT('Ctrl Pts',(3.81879275370222,-1.43767098648142,-4.94904266266236));
#17139=CARTESIAN_POINT('Ctrl Pts',(3.76413610405804,-1.44616023635568,-4.95204484391012));
#17140=CARTESIAN_POINT('Ctrl Pts',(3.70945457592029,-1.45465335034802,-4.95504839168414));
#17141=CARTESIAN_POINT('Ctrl Pts',(3.65433294714216,-1.46003424267016,-4.95805193945816));
#17142=CARTESIAN_POINT('Ctrl Pts',(3.59915227362332,-1.46228455804291,-4.96105548723217));
#17143=CARTESIAN_POINT('Ctrl Pts',(3.54386745586965,-1.46453912050721,-4.96406470369714));
#17144=CARTESIAN_POINT('Ctrl Pts',(3.48852390010615,-1.46365131149307,-4.96707392016211));
#17145=CARTESIAN_POINT('Ctrl Pts',(3.43350166766549,-1.45965494708621,-4.97008313662708));
#17146=CARTESIAN_POINT('Ctrl Pts',(3.39140740485943,-1.45659756453103,-4.9723853105502));
#17147=CARTESIAN_POINT('Ctrl Pts',(3.34950120399534,-1.45172186801083,-4.97468748447332));
#17148=CARTESIAN_POINT('Ctrl Pts',(3.30794911626834,-1.44506318740587,-4.97698965839643));
#17149=CARTESIAN_POINT('Ctrl Pts',(3.25361910716469,-1.43635685764783,-4.97999978705767));
#17150=CARTESIAN_POINT('Ctrl Pts',(3.19966662510328,-1.42456400866142,-4.98300991571891));
#17151=CARTESIAN_POINT('Ctrl Pts',(3.14646851405652,-1.40973172123707,-4.98602004438014));
#17152=CARTESIAN_POINT('Ctrl Pts',(3.0933649510427,-1.39492579496676,-4.98902482319459));
#17153=CARTESIAN_POINT('Ctrl Pts',(3.04101360295494,-1.37709129113015,-4.99202960200903));
#17154=CARTESIAN_POINT('Ctrl Pts',(2.9897820059895,-1.35632644742242,-4.99503438082347));
#17155=CARTESIAN_POINT('Ctrl Pts',(2.93860109420154,-1.33558214708735,-4.99803618690709));
#17156=CARTESIAN_POINT('Ctrl Pts',(2.88853822605648,-1.31191344723265,-5.00103799299071));
#17157=CARTESIAN_POINT('Ctrl Pts',(2.83994482500906,-1.28546806772339,-5.00403979907433));
#17158=CARTESIAN_POINT('Ctrl Pts',(2.7913803058636,-1.25903840625077,-5.00703982100892));
#17159=CARTESIAN_POINT('Ctrl Pts',(2.7442839856446,-1.22983558815535,-5.01003984294352));
#17160=CARTESIAN_POINT('Ctrl Pts',(2.69898425198183,-1.19805404828392,-5.01303986487811));
#17161=CARTESIAN_POINT('Ctrl Pts',(2.65369355135973,-1.1662788458436,-5.0160392885902));
#17162=CARTESIAN_POINT('Ctrl Pts',(2.61019915790964,-1.13192624597554,-5.0190387123023));
#17163=CARTESIAN_POINT('Ctrl Pts',(2.56879997983906,-1.0952336444817,-5.02203813601439));
#17164=CARTESIAN_POINT('Ctrl Pts',(2.5273627412205,-1.05850730945534,-5.02504031726215));
#17165=CARTESIAN_POINT('Ctrl Pts',(2.48802496244617,-1.01943702584492,-5.0280424985099));
#17166=CARTESIAN_POINT('Ctrl Pts',(2.45105080840114,-0.978299103602709,
-5.03104467975766));
#17167=CARTESIAN_POINT('Ctrl Pts',(2.41405982454195,-0.937142456291482,
-5.03404822753168));
#17168=CARTESIAN_POINT('Ctrl Pts',(2.37943494082837,-0.893916707146323,
-5.0370517753057));
#17169=CARTESIAN_POINT('Ctrl Pts',(2.34739973774838,-0.848930971486027,
-5.04005532307972));
#17170=CARTESIAN_POINT('Ctrl Pts',(2.31530407361389,-0.803860332820476,
-5.04306453954468));
#17171=CARTESIAN_POINT('Ctrl Pts',(2.28580813594504,-0.757023520050787,
-5.04607375600965));
#17172=CARTESIAN_POINT('Ctrl Pts',(2.25909126688016,-0.708757321748141,
-5.04908297247461));
#17173=CARTESIAN_POINT('Ctrl Pts',(2.23865176710177,-0.671831701941607,
-5.05138514639774));
#17174=CARTESIAN_POINT('Ctrl Pts',(2.21983791051209,-0.634070069460272,
-5.05368732032087));
#17175=CARTESIAN_POINT('Ctrl Pts',(2.20271083710676,-0.595630800756864,
-5.055989494244));
#17176=CARTESIAN_POINT('Ctrl Pts',(2.17822463627681,-0.540675022209486,
-5.05928086175864));
#17177=CARTESIAN_POINT('Ctrl Pts',(2.15709871382792,-0.484134691290982,
-5.06257222927328));
#17178=CARTESIAN_POINT('Ctrl Pts',(2.13951937131544,-0.42641898233868,-5.06586359678792));
#17179=CARTESIAN_POINT('Ctrl Pts',(2.12199297534358,-0.368877105094038,
-5.06914505116027));
#17180=CARTESIAN_POINT('Ctrl Pts',(2.10799201218925,-0.310167235961898,
-5.07242650553261));
#17181=CARTESIAN_POINT('Ctrl Pts',(2.09765464740422,-0.250717556839019,
-5.07570795990495));
#17182=CARTESIAN_POINT('Ctrl Pts',(2.08736539805606,-0.191544587239539,
-5.07897414069317));
#17183=CARTESIAN_POINT('Ctrl Pts',(2.08070586389208,-0.131639017030512,
-5.08224032148139));
#17184=CARTESIAN_POINT('Ctrl Pts',(2.0777637777177,-0.071440693713586,-5.0855065022696));
#17185=CARTESIAN_POINT('Ctrl Pts',(2.07661125362505,-0.047858781476013,
-5.08678598622291));
#17186=CARTESIAN_POINT('Ctrl Pts',(2.07602866300798,-0.0242321078209353,
-5.08806547017621));
#17187=CARTESIAN_POINT('Ctrl Pts',(2.07601916841636,-0.000587678975561644,
-5.08934495412951));
#17188=CARTESIAN_POINT('Origin',(3.53951905042299,8.32667268468867E-16,
0.));
#17189=CARTESIAN_POINT('',(2.07601962619751,0.00129818785261296,-5.66065504584291));
#17190=CARTESIAN_POINT('',(2.07601963090622,0.00130348536077232,-5.58934495415709));
#17191=CARTESIAN_POINT('',(2.07601905042299,1.01189432752408E-15,0.));
#17192=CARTESIAN_POINT('Ctrl Pts',(2.07601962619751,0.00129818785261296,
-5.66065504584291));
#17193=CARTESIAN_POINT('Ctrl Pts',(2.07597114765928,-0.0533536197810684,
-5.65768502711364));
#17194=CARTESIAN_POINT('Ctrl Pts',(2.07898825837672,-0.108079334828836,
-5.65471500838437));
#17195=CARTESIAN_POINT('Ctrl Pts',(2.08506915307526,-0.162504603335374,
-5.65174498965511));
#17196=CARTESIAN_POINT('Ctrl Pts',(2.09114622993757,-0.216895701415943,
-5.64877683562597));
#17197=CARTESIAN_POINT('Ctrl Pts',(2.10028322128251,-0.270986190441087,
-5.64580868159683));
#17198=CARTESIAN_POINT('Ctrl Pts',(2.11242635184785,-0.324405116595802,
-5.64284052756769));
#17199=CARTESIAN_POINT('Ctrl Pts',(2.12456691007413,-0.377812726756688,
-5.63987300229721));
#17200=CARTESIAN_POINT('Ctrl Pts',(2.1397122236165,-0.430548529546075,-5.63690547702674));
#17201=CARTESIAN_POINT('Ctrl Pts',(2.15775758481954,-0.482252529462938,
-5.63393795175626));
#17202=CARTESIAN_POINT('Ctrl Pts',(2.1758191975795,-0.534003093728829,-5.63096775394821));
#17203=CARTESIAN_POINT('Ctrl Pts',(2.19678589465581,-0.584719488164479,
-5.62799755614017));
#17204=CARTESIAN_POINT('Ctrl Pts',(2.22050385984984,-0.634059285112427,
-5.62502735833212));
#17205=CARTESIAN_POINT('Ctrl Pts',(2.24423325748627,-0.683422864639618,
-5.62205572884074));
#17206=CARTESIAN_POINT('Ctrl Pts',(2.27071630107471,-0.731408052320245,
-5.61908409934937));
#17207=CARTESIAN_POINT('Ctrl Pts',(2.29975359853863,-0.77769780397914,-5.61611246985799));
#17208=CARTESIAN_POINT('Ctrl Pts',(2.32884376638286,-0.824071838852668,
-5.61313542969844));
#17209=CARTESIAN_POINT('Ctrl Pts',(2.36049715663055,-0.868743835850679,
-5.61015838953888));
#17210=CARTESIAN_POINT('Ctrl Pts',(2.39447240308624,-0.911427685240511,
-5.60718134937933));
#17211=CARTESIAN_POINT('Ctrl Pts',(2.41414427305429,-0.936141888153728,
-5.60545762540326));
#17212=CARTESIAN_POINT('Ctrl Pts',(2.43459380573541,-0.960190211352025,
-5.6037339014272));
#17213=CARTESIAN_POINT('Ctrl Pts',(2.45576864304273,-0.983522904920427,
-5.60201017745113));
#17214=CARTESIAN_POINT('Ctrl Pts',(2.49274613222366,-1.02426864532286,-5.59900004878989));
#17215=CARTESIAN_POINT('Ctrl Pts',(2.53210238503181,-1.06301173467714,-5.59598992012865));
#17216=CARTESIAN_POINT('Ctrl Pts',(2.57359206397092,-1.09946228077348,-5.59297979146741));
#17217=CARTESIAN_POINT('Ctrl Pts',(2.61500800405997,-1.1358480439787,-5.58997501265296));
#17218=CARTESIAN_POINT('Ctrl Pts',(2.65854945208602,-1.16994900404583,-5.58697023383852));
#17219=CARTESIAN_POINT('Ctrl Pts',(2.70393331100067,-1.20151101621002,-5.58396545502407));
#17220=CARTESIAN_POINT('Ctrl Pts',(2.74927227010583,-1.23304180299218,-5.58096364894045));
#17221=CARTESIAN_POINT('Ctrl Pts',(2.79644959785539,-1.26203831771608,-5.57796184285684));
#17222=CARTESIAN_POINT('Ctrl Pts',(2.84514955849066,-1.28828694733496,-5.57496003677322));
#17223=CARTESIAN_POINT('Ctrl Pts',(2.8938205738894,-1.31451997585719,-5.57196001483862));
#17224=CARTESIAN_POINT('Ctrl Pts',(2.9440119644637,-1.3380081063726,-5.56895999290402));
#17225=CARTESIAN_POINT('Ctrl Pts',(2.99538145608477,-1.35858254384039,-5.56595997096942));
#17226=CARTESIAN_POINT('Ctrl Pts',(3.04674070431875,-1.37915287864099,-5.56296054725732));
#17227=CARTESIAN_POINT('Ctrl Pts',(3.09927709707663,-1.39681047800447,-5.55996112354523));
#17228=CARTESIAN_POINT('Ctrl Pts',(3.15262848671406,-1.41143471039683,-5.55696169983314));
#17229=CARTESIAN_POINT('Ctrl Pts',(3.20602892522683,-1.42607238765269,-5.55395951858537));
#17230=CARTESIAN_POINT('Ctrl Pts',(3.26024534714408,-1.43767098648148,-5.55095733733761));
#17231=CARTESIAN_POINT('Ctrl Pts',(3.31490199678827,-1.44616023635573,-5.54795515608985));
#17232=CARTESIAN_POINT('Ctrl Pts',(3.36958352492605,-1.45465335034806,-5.54495160831583));
#17233=CARTESIAN_POINT('Ctrl Pts',(3.4247051537042,-1.46003424267019,-5.54194806054181));
#17234=CARTESIAN_POINT('Ctrl Pts',(3.47988582722307,-1.46228455804292,-5.5389445127678));
#17235=CARTESIAN_POINT('Ctrl Pts',(3.53517064497669,-1.46453912050721,-5.53593529630283));
#17236=CARTESIAN_POINT('Ctrl Pts',(3.59051420074016,-1.46365131149306,-5.53292607983786));
#17237=CARTESIAN_POINT('Ctrl Pts',(3.64553643318078,-1.45965494708619,-5.5299168633729));
#17238=CARTESIAN_POINT('Ctrl Pts',(3.68763069598673,-1.45659756453101,-5.52761468944978));
#17239=CARTESIAN_POINT('Ctrl Pts',(3.72953689685072,-1.45172186801082,-5.52531251552667));
#17240=CARTESIAN_POINT('Ctrl Pts',(3.77108898457761,-1.44506318740587,-5.52301034160356));
#17241=CARTESIAN_POINT('Ctrl Pts',(3.82541899368129,-1.43635685764783,-5.52000021294232));
#17242=CARTESIAN_POINT('Ctrl Pts',(3.87937147574273,-1.42456400866141,-5.51699008428108));
#17243=CARTESIAN_POINT('Ctrl Pts',(3.93256958678952,-1.40973172123705,-5.51397995561984));
#17244=CARTESIAN_POINT('Ctrl Pts',(3.98567314980338,-1.39492579496673,-5.5109751768054));
#17245=CARTESIAN_POINT('Ctrl Pts',(4.03802449789117,-1.37709129113011,-5.50797039799095));
#17246=CARTESIAN_POINT('Ctrl Pts',(4.08925609485665,-1.35632644742235,-5.50496561917651));
#17247=CARTESIAN_POINT('Ctrl Pts',(4.14043700664466,-1.33558214708726,-5.50196381309289));
#17248=CARTESIAN_POINT('Ctrl Pts',(4.19049987478974,-1.31191344723253,-5.49896200700927));
#17249=CARTESIAN_POINT('Ctrl Pts',(4.23909327583719,-1.28546806772324,-5.49596020092565));
#17250=CARTESIAN_POINT('Ctrl Pts',(4.2876577949827,-1.25903840625058,-5.49296017899105));
#17251=CARTESIAN_POINT('Ctrl Pts',(4.33475411520175,-1.22983558815512,-5.48996015705645));
#17252=CARTESIAN_POINT('Ctrl Pts',(4.38005384886455,-1.19805404828363,-5.48696013512185));
#17253=CARTESIAN_POINT('Ctrl Pts',(4.42534454948663,-1.16627884584332,-5.48396071140976));
#17254=CARTESIAN_POINT('Ctrl Pts',(4.46883894293668,-1.13192624597526,-5.48096128769767));
#17255=CARTESIAN_POINT('Ctrl Pts',(4.51023812100723,-1.09523364448143,-5.47796186398559));
#17256=CARTESIAN_POINT('Ctrl Pts',(4.55167535962579,-1.05850730945505,-5.47495968273783));
#17257=CARTESIAN_POINT('Ctrl Pts',(4.59101313840011,-1.01943702584461,-5.47195750149007));
#17258=CARTESIAN_POINT('Ctrl Pts',(4.62798729244513,-0.978299103602381,
-5.46895532024231));
#17259=CARTESIAN_POINT('Ctrl Pts',(4.66497827630434,-0.937142456291102,
-5.46595177246829));
#17260=CARTESIAN_POINT('Ctrl Pts',(4.69960316001795,-0.89391670714589,-5.46294822469427));
#17261=CARTESIAN_POINT('Ctrl Pts',(4.73163836309795,-0.848930971485537,
-5.45994467692025));
#17262=CARTESIAN_POINT('Ctrl Pts',(4.76373402723243,-0.803860332819957,
-5.45693546045528));
#17263=CARTESIAN_POINT('Ctrl Pts',(4.79322996490127,-0.757023520050236,
-5.45392624399032));
#17264=CARTESIAN_POINT('Ctrl Pts',(4.81994683396614,-0.708757321747561,
-5.45091702752535));
#17265=CARTESIAN_POINT('Ctrl Pts',(4.84038633374441,-0.671831701941208,
-5.44861485360224));
#17266=CARTESIAN_POINT('Ctrl Pts',(4.85920019033398,-0.634070069460065,
-5.44631267967912));
#17267=CARTESIAN_POINT('Ctrl Pts',(4.87632726373923,-0.595630800756855,
-5.44401050575601));
#17268=CARTESIAN_POINT('Ctrl Pts',(4.89872118194956,-0.545370851550297,
-5.44100037709477));
#17269=CARTESIAN_POINT('Ctrl Pts',(4.91832377794496,-0.493740629412078,
-5.43799024843354));
#17270=CARTESIAN_POINT('Ctrl Pts',(4.93496857708735,-0.441081476070143,
-5.4349801197723));
#17271=CARTESIAN_POINT('Ctrl Pts',(4.95158379373167,-0.388515912881416,
-5.43197534095786));
#17272=CARTESIAN_POINT('Ctrl Pts',(4.9652514878736,-0.33492554704438,-5.42897056214341));
#17273=CARTESIAN_POINT('Ctrl Pts',(4.97585311589188,-0.280671876705873,
-5.42596578332897));
#17274=CARTESIAN_POINT('Ctrl Pts',(4.98644425535566,-0.226471881385757,
-5.42296397724535));
#17275=CARTESIAN_POINT('Ctrl Pts',(4.99397523686006,-0.171610397288949,
-5.41996217116173));
#17276=CARTESIAN_POINT('Ctrl Pts',(4.99837776337159,-0.116462464571016,
-5.41696036507811));
#17277=CARTESIAN_POINT('Ctrl Pts',(5.00277767320397,-0.0613473094967593,
-5.41396034314351));
#17278=CARTESIAN_POINT('Ctrl Pts',(5.00405277160113,-0.00594656864460139,
-5.41096032120891));
#17279=CARTESIAN_POINT('Ctrl Pts',(5.00218647326826,0.0493584860706374,
-5.40796029927431));
#17280=CARTESIAN_POINT('Ctrl Pts',(5.00032054708656,0.104652512623676,-5.40496087556222));
#17281=CARTESIAN_POINT('Ctrl Pts',(4.9953144860066,0.159850363412901,-5.40196145185013));
#17282=CARTESIAN_POINT('Ctrl Pts',(4.98720379313038,0.214571982635766,-5.39896202813804));
#17283=CARTESIAN_POINT('Ctrl Pts',(4.97908564364681,0.269343910461643,-5.39595984689028));
#17284=CARTESIAN_POINT('Ctrl Pts',(4.96785723752433,0.323638208470234,-5.39295766564252));
#17285=CARTESIAN_POINT('Ctrl Pts',(4.95360565312807,0.377082656787611,-5.38995548439476));
#17286=CARTESIAN_POINT('Ctrl Pts',(4.93934758172696,0.430551431831492,-5.38695193662074));
#17287=CARTESIAN_POINT('Ctrl Pts',(4.92206375402316,0.483169083444289,-5.38394838884672));
#17288=CARTESIAN_POINT('Ctrl Pts',(4.90189089891441,0.534579457553378,-5.3809448410727));
#17289=CARTESIAN_POINT('Ctrl Pts',(4.8816799709366,0.586086860091577,-5.37793562460774));
#17290=CARTESIAN_POINT('Ctrl Pts',(4.85856934427834,0.636381952345708,-5.37492640814277));
#17291=CARTESIAN_POINT('Ctrl Pts',(4.8327430965916,0.685130510495105,-5.3719171916778));
#17292=CARTESIAN_POINT('Ctrl Pts',(4.81298495866809,0.722425155352967,-5.36961501775468));
#17293=CARTESIAN_POINT('Ctrl Pts',(4.79163839257322,0.758815074333101,-5.36731284383156));
#17294=CARTESIAN_POINT('Ctrl Pts',(4.76880263619492,0.794162524771662,-5.36501066990844));
#17295=CARTESIAN_POINT('Ctrl Pts',(4.73894452509179,0.840379872904255,-5.3620005412472));
#17296=CARTESIAN_POINT('Ctrl Pts',(4.70641360602975,0.885008125309868,-5.35899041258596));
#17297=CARTESIAN_POINT('Ctrl Pts',(4.67140480080371,0.927721347218594,-5.35598028392473));
#17298=CARTESIAN_POINT('Ctrl Pts',(4.63645821608895,0.970358655696731,-5.35297550511028));
#17299=CARTESIAN_POINT('Ctrl Pts',(4.5990428168513,1.01108728289669,-5.34997072629584));
#17300=CARTESIAN_POINT('Ctrl Pts',(4.55939659574844,1.04961042417696,-5.3469659474814));
#17301=CARTESIAN_POINT('Ctrl Pts',(4.519789598013,1.08809545319123,-5.34396414139778));
#17302=CARTESIAN_POINT('Ctrl Pts',(4.47795652732849,1.12437895242752,-5.34096233531416));
#17303=CARTESIAN_POINT('Ctrl Pts',(4.4341741726876,1.15819880081345,-5.33796052923054));
#17304=CARTESIAN_POINT('Ctrl Pts',(4.39041784046222,1.19199854808434,-5.33496050729594));
#17305=CARTESIAN_POINT('Ctrl Pts',(4.34471493776048,1.22333722462832,-5.33196048536134));
#17306=CARTESIAN_POINT('Ctrl Pts',(4.29737572793224,1.2519926143371,-5.32896046342674));
#17307=CARTESIAN_POINT('Ctrl Pts',(4.25004595782853,1.28064228998799,-5.32596103971465));
#17308=CARTESIAN_POINT('Ctrl Pts',(4.20108098013394,1.30660946809153,-5.32296161600255));
#17309=CARTESIAN_POINT('Ctrl Pts',(4.15081850056707,1.32971622245258,-5.31996219229046));
#17310=CARTESIAN_POINT('Ctrl Pts',(4.10050981193029,1.35284422012746,-5.3169600110427));
#17311=CARTESIAN_POINT('Ctrl Pts',(4.04890171910207,1.37310631910392,-5.31395782979494));
#17312=CARTESIAN_POINT('Ctrl Pts',(3.99635354552124,1.3903720703784,-5.31095564854718));
#17313=CARTESIAN_POINT('Ctrl Pts',(3.94378145317827,1.40764568063959,-5.30795210077316));
#17314=CARTESIAN_POINT('Ctrl Pts',(3.89026893824923,1.42192008806373,-5.30494855299914));
#17315=CARTESIAN_POINT('Ctrl Pts',(3.83618899748807,1.43311520559528,-5.30194500522513));
#17316=CARTESIAN_POINT('Ctrl Pts',(3.78200698994002,1.44433145202711,-5.29893578876016));
#17317=CARTESIAN_POINT('Ctrl Pts',(3.7272559409058,1.4524567211945,-5.29592657229519));
#17318=CARTESIAN_POINT('Ctrl Pts',(3.6723163511366,1.45746256450146,-5.29291735583023));
#17319=CARTESIAN_POINT('Ctrl Pts',(3.63028531336119,1.46129223978693,-5.29061518190711));
#17320=CARTESIAN_POINT('Ctrl Pts',(3.58814409693993,1.46329722506164,-5.28831300798399));
#17321=CARTESIAN_POINT('Ctrl Pts',(3.54606228825325,1.46348537267671,-5.28601083406088));
#17322=CARTESIAN_POINT('Ctrl Pts',(3.4910396606522,1.46373137864654,-5.28300070539964));
#17323=CARTESIAN_POINT('Ctrl Pts',(3.43588753171339,1.46087056035062,-5.2799905767384));
#17324=CARTESIAN_POINT('Ctrl Pts',(3.38098538508204,1.45488808055931,-5.27698044807717));
#17325=CARTESIAN_POINT('Ctrl Pts',(3.32618081503499,1.44891623332028,-5.27397566926272));
#17326=CARTESIAN_POINT('Ctrl Pts',(3.27162586636294,1.43983379151762,-5.27097089044828));
#17327=CARTESIAN_POINT('Ctrl Pts',(3.21769915919492,1.42767790751624,-5.26796611163383));
#17328=CARTESIAN_POINT('Ctrl Pts',(3.16382580356946,1.41553404974818,-5.26496430555021));
#17329=CARTESIAN_POINT('Ctrl Pts',(3.110579970862,1.40032288874678,-5.26196249946659));
#17330=CARTESIAN_POINT('Ctrl Pts',(3.05833243094417,1.38213302081766,-5.25896069338298));
#17331=CARTESIAN_POINT('Ctrl Pts',(3.00611594479678,1.3639539641915,-5.25596067144838));
#17332=CARTESIAN_POINT('Ctrl Pts',(2.95489707315103,1.34279988301949,-5.25296064951378));
#17333=CARTESIAN_POINT('Ctrl Pts',(2.90503145465448,1.31880921319799,-5.24996062757917));
#17334=CARTESIAN_POINT('Ctrl Pts',(2.85517577966366,1.29482332726106,-5.24696120386708));
#17335=CARTESIAN_POINT('Ctrl Pts',(2.80667329755418,1.2680022048291,-5.24396178015499));
#17336=CARTESIAN_POINT('Ctrl Pts',(2.75985754738192,1.23853146535554,-5.24096235644289));
#17337=CARTESIAN_POINT('Ctrl Pts',(2.71299875690819,1.20903363180559,-5.23796017519514));
#17338=CARTESIAN_POINT('Ctrl Pts',(2.66783024437489,1.17688159647613,-5.23495799394737));
#17339=CARTESIAN_POINT('Ctrl Pts',(2.62465759724969,1.14230502559415,-5.23195581269962));
#17340=CARTESIAN_POINT('Ctrl Pts',(2.58146529889392,1.10771271622468,-5.2289522649256));
#17341=CARTESIAN_POINT('Ctrl Pts',(2.54027107042225,1.07069402497338,-5.22594871715158));
#17342=CARTESIAN_POINT('Ctrl Pts',(2.50134579086117,1.0315175874074,-5.22294516937757));
#17343=CARTESIAN_POINT('Ctrl Pts',(2.46234704638573,0.992267210908591,-5.2199359529126));
#17344=CARTESIAN_POINT('Ctrl Pts',(2.42562615652234,0.950851349007231,-5.21692673644763));
#17345=CARTESIAN_POINT('Ctrl Pts',(2.39141485185252,0.90757313712166,-5.21391751998266));
#17346=CARTESIAN_POINT('Ctrl Pts',(2.36524180169027,0.874463531348206,-5.21161534605955));
#17347=CARTESIAN_POINT('Ctrl Pts',(2.34053677734022,0.840264644534776,-5.20931317213643));
#17348=CARTESIAN_POINT('Ctrl Pts',(2.31738586357953,0.805122800332869,-5.20701099821332));
#17349=CARTESIAN_POINT('Ctrl Pts',(2.28656148700224,0.758333051535187,-5.20394575954991));
#17350=CARTESIAN_POINT('Ctrl Pts',(2.25836766374379,0.709679539907307,-5.2008805208865));
#17351=CARTESIAN_POINT('Ctrl Pts',(2.23302982051775,0.659483238711648,-5.19781528222309));
#17352=CARTESIAN_POINT('Ctrl Pts',(2.20743202463528,0.608771950438284,-5.19471859585807));
#17353=CARTESIAN_POINT('Ctrl Pts',(2.18474950720201,0.55648641724976,-5.19162190949306));
#17354=CARTESIAN_POINT('Ctrl Pts',(2.16517011740709,0.502988330200676,-5.18852522312805));
#17355=CARTESIAN_POINT('Ctrl Pts',(2.14585640794371,0.450216179437288,-5.18547055690098));
#17356=CARTESIAN_POINT('Ctrl Pts',(2.12956232042806,0.396264660733128,-5.18241589067391));
#17357=CARTESIAN_POINT('Ctrl Pts',(2.11642128931065,0.341504044364121,-5.17936122444685));
#17358=CARTESIAN_POINT('Ctrl Pts',(2.10300910519356,0.285613493421454,-5.17624352801286));
#17359=CARTESIAN_POINT('Ctrl Pts',(2.09288180219176,0.228880562508218,-5.17312583157887));
#17360=CARTESIAN_POINT('Ctrl Pts',(2.08612790286529,0.171716109322651,-5.17000813514488));
#17361=CARTESIAN_POINT('Ctrl Pts',(2.07937400353882,0.114551656137083,-5.16689043871089));
#17362=CARTESIAN_POINT('Ctrl Pts',(2.07599361023914,0.0569562315344585,
-5.1637727422769));
#17363=CARTESIAN_POINT('Ctrl Pts',(2.0760191947603,-0.000649980989682889,
-5.16065504584291));
#17364=CARTESIAN_POINT('Ctrl Pts',(2.07601916841615,-0.000587678466146558,
-5.08934495415708));
#17365=CARTESIAN_POINT('Ctrl Pts',(2.07599647908465,0.0559157258477616,
-5.09240255388168));
#17366=CARTESIAN_POINT('Ctrl Pts',(2.0792503896227,0.112403252583727,-5.09546015360627));
#17367=CARTESIAN_POINT('Ctrl Pts',(2.08574917914879,0.168479706123322,-5.09851775333087));
#17368=CARTESIAN_POINT('Ctrl Pts',(2.09225826286632,0.224644985704336,-5.10158019634463));
#17369=CARTESIAN_POINT('Ctrl Pts',(2.10202243211027,0.280397394683112,-5.1046426393584));
#17370=CARTESIAN_POINT('Ctrl Pts',(2.11495823197472,0.335348661160296,-5.10770508237216));
#17371=CARTESIAN_POINT('Ctrl Pts',(2.12790393526328,0.390341997374393,-5.1107698699392));
#17372=CARTESIAN_POINT('Ctrl Pts',(2.1440259636609,0.444532490215689,-5.11383465750624));
#17373=CARTESIAN_POINT('Ctrl Pts',(2.16319090346734,0.49754706500755,-5.11689944507328));
#17374=CARTESIAN_POINT('Ctrl Pts',(2.18240188203802,0.550688993474133,-5.11997159499228));
#17375=CARTESIAN_POINT('Ctrl Pts',(2.20467018624253,0.602648896761848,-5.12304374491128));
#17376=CARTESIAN_POINT('Ctrl Pts',(2.22981434073402,0.653074133172129,-5.12611589483029));
#17377=CARTESIAN_POINT('Ctrl Pts',(2.25402268917208,0.701622661360063,-5.12907370658405));
#17378=CARTESIAN_POINT('Ctrl Pts',(2.28089629616199,0.748748447528253,-5.1320315183378));
#17379=CARTESIAN_POINT('Ctrl Pts',(2.31023546465109,0.794162524771709,-5.13498933009156));
#17380=CARTESIAN_POINT('Ctrl Pts',(2.34009357575423,0.840379872904314,-5.1379994587528));
#17381=CARTESIAN_POINT('Ctrl Pts',(2.37262449481628,0.885008125309938,-5.14100958741403));
#17382=CARTESIAN_POINT('Ctrl Pts',(2.40763330004234,0.927721347218673,-5.14401971607527));
#17383=CARTESIAN_POINT('Ctrl Pts',(2.4425798847571,0.970358655696808,-5.14702449488971));
#17384=CARTESIAN_POINT('Ctrl Pts',(2.47999528399475,1.01108728289676,-5.15002927370416));
#17385=CARTESIAN_POINT('Ctrl Pts',(2.51964150509762,1.04961042417703,-5.1530340525186));
#17386=CARTESIAN_POINT('Ctrl Pts',(2.55924850283305,1.08809545319129,-5.15603585860222));
#17387=CARTESIAN_POINT('Ctrl Pts',(2.60108157351756,1.12437895242757,-5.15903766468584));
#17388=CARTESIAN_POINT('Ctrl Pts',(2.64486392815845,1.1581988008135,-5.16203947076946));
#17389=CARTESIAN_POINT('Ctrl Pts',(2.68862026038384,1.1919985480844,-5.16503949270406));
#17390=CARTESIAN_POINT('Ctrl Pts',(2.73432316308559,1.22333722462838,-5.16803951463866));
#17391=CARTESIAN_POINT('Ctrl Pts',(2.78166237291385,1.25199261433716,-5.17103953657326));
#17392=CARTESIAN_POINT('Ctrl Pts',(2.82899214301756,1.28064228998806,-5.17403896028535));
#17393=CARTESIAN_POINT('Ctrl Pts',(2.87795712071217,1.3066094680916,-5.17703838399745));
#17394=CARTESIAN_POINT('Ctrl Pts',(2.92821960027905,1.32971622245264,-5.18003780770955));
#17395=CARTESIAN_POINT('Ctrl Pts',(2.97852828891583,1.35284422012751,-5.1830399889573));
#17396=CARTESIAN_POINT('Ctrl Pts',(3.03013638174404,1.37310631910397,-5.18604217020506));
#17397=CARTESIAN_POINT('Ctrl Pts',(3.08268455532486,1.39037207037844,-5.18904435145282));
#17398=CARTESIAN_POINT('Ctrl Pts',(3.13525664766784,1.40764568063963,-5.19204789922684));
#17399=CARTESIAN_POINT('Ctrl Pts',(3.18876916259689,1.42192008806376,-5.19505144700086));
#17400=CARTESIAN_POINT('Ctrl Pts',(3.24284910335806,1.43311520559531,-5.19805499477488));
#17401=CARTESIAN_POINT('Ctrl Pts',(3.29703111090612,1.44433145202714,-5.20106421123985));
#17402=CARTESIAN_POINT('Ctrl Pts',(3.35178215994035,1.45245672119452,-5.20407342770481));
#17403=CARTESIAN_POINT('Ctrl Pts',(3.40672174970956,1.45746256450148,-5.20708264416978));
#17404=CARTESIAN_POINT('Ctrl Pts',(3.44875278748493,1.46129223978694,-5.2093848180929));
#17405=CARTESIAN_POINT('Ctrl Pts',(3.49089400390613,1.46329722506164,-5.21168699201601));
#17406=CARTESIAN_POINT('Ctrl Pts',(3.53297581259277,1.46348537267671,-5.21398916593912));
#17407=CARTESIAN_POINT('Ctrl Pts',(3.58799844019384,1.46373137864654,-5.21699929460036));
#17408=CARTESIAN_POINT('Ctrl Pts',(3.64315056913268,1.46087056035061,-5.2200094232616));
#17409=CARTESIAN_POINT('Ctrl Pts',(3.69805271576405,1.4548880805593,-5.22301955192284));
#17410=CARTESIAN_POINT('Ctrl Pts',(3.75285728581109,1.44891623332026,-5.22602433073728));
#17411=CARTESIAN_POINT('Ctrl Pts',(3.8074122344831,1.43983379151761,-5.22902910955173));
#17412=CARTESIAN_POINT('Ctrl Pts',(3.86133894165111,1.42767790751623,-5.23203388836617));
#17413=CARTESIAN_POINT('Ctrl Pts',(3.91521229727657,1.41553404974817,-5.23503569444979));
#17414=CARTESIAN_POINT('Ctrl Pts',(3.96845812998403,1.40032288874676,-5.23803750053341));
#17415=CARTESIAN_POINT('Ctrl Pts',(4.02070566990185,1.38213302081764,-5.24103930661702));
#17416=CARTESIAN_POINT('Ctrl Pts',(4.07292215604919,1.3639539641915,-5.24403932855162));
#17417=CARTESIAN_POINT('Ctrl Pts',(4.12414102769489,1.34279988301951,-5.24703935048622));
#17418=CARTESIAN_POINT('Ctrl Pts',(4.17400664619139,1.31880921319804,-5.25003937242082));
#17419=CARTESIAN_POINT('Ctrl Pts',(4.22386232118207,1.29482332726118,-5.2530387961329));
#17420=CARTESIAN_POINT('Ctrl Pts',(4.27236480329143,1.2680022048293,-5.25603821984499));
#17421=CARTESIAN_POINT('Ctrl Pts',(4.31918055346358,1.23853146535584,-5.25903764355707));
#17422=CARTESIAN_POINT('Ctrl Pts',(4.36603934393731,1.20903363180591,-5.26203982480483));
#17423=CARTESIAN_POINT('Ctrl Pts',(4.41120785647062,1.17688159647647,-5.26504200605259));
#17424=CARTESIAN_POINT('Ctrl Pts',(4.45438050359583,1.14230502559452,-5.26804418730035));
#17425=CARTESIAN_POINT('Ctrl Pts',(4.49757280195163,1.10771271622504,-5.27104773507437));
#17426=CARTESIAN_POINT('Ctrl Pts',(4.53876703042334,1.07069402497375,-5.27405128284839));
#17427=CARTESIAN_POINT('Ctrl Pts',(4.57769230998446,1.03151758740776,-5.27705483062241));
#17428=CARTESIAN_POINT('Ctrl Pts',(4.61669105445989,0.992267210908983,-5.28006404708737));
#17429=CARTESIAN_POINT('Ctrl Pts',(4.65341194432327,0.950851349007655,-5.28307326355234));
#17430=CARTESIAN_POINT('Ctrl Pts',(4.6876232489931,0.907573137122119,-5.2860824800173));
#17431=CARTESIAN_POINT('Ctrl Pts',(4.71379629915549,0.874463531348512,-5.28838465394043));
#17432=CARTESIAN_POINT('Ctrl Pts',(4.73850132350566,0.840264644534916,-5.29068682786356));
#17433=CARTESIAN_POINT('Ctrl Pts',(4.76165223726647,0.805122800332836,-5.29298900178668));
#17434=CARTESIAN_POINT('Ctrl Pts',(4.79192242161058,0.759174285592591,-5.29599913044792));
#17435=CARTESIAN_POINT('Ctrl Pts',(4.81966131604092,0.711419753414092,-5.29900925910916));
#17436=CARTESIAN_POINT('Ctrl Pts',(4.84464914560435,0.662168924559209,-5.3020193877704));
#17437=CARTESIAN_POINT('Ctrl Pts',(4.86959256475384,0.613005628304572,-5.30502416658484));
#17438=CARTESIAN_POINT('Ctrl Pts',(4.89179438510166,0.562351780010985,-5.30802894539928));
#17439=CARTESIAN_POINT('Ctrl Pts',(4.91107884620114,0.510544784132602,-5.31103372421373));
#17440=CARTESIAN_POINT('Ctrl Pts',(4.93034422852127,0.458789042693621,-5.31403553029735));
#17441=CARTESIAN_POINT('Ctrl Pts',(4.94669778577434,0.405882906141302,-5.31703733638096));
#17442=CARTESIAN_POINT('Ctrl Pts',(4.96001113254836,0.352185312895246,-5.32003914246458));
#17443=CARTESIAN_POINT('Ctrl Pts',(4.97331656642131,0.29851963527119,-5.32303916439918));
#17444=CARTESIAN_POINT('Ctrl Pts',(4.983585244523,0.24406394490794,-5.32603918633378));
#17445=CARTESIAN_POINT('Ctrl Pts',(4.99073879108145,0.189191739574429,-5.32903920826838));
#17446=CARTESIAN_POINT('Ctrl Pts',(4.99789091117947,0.134330476090335,-5.33203863198048));
#17447=CARTESIAN_POINT('Ctrl Pts',(5.00192906513011,0.0790533859719109,
-5.33503805569257));
#17448=CARTESIAN_POINT('Ctrl Pts',(5.0028264697904,0.0237412388956652,-5.33803747940466));
#17449=CARTESIAN_POINT('Ctrl Pts',(5.00372469948429,-0.0316217596883739,
-5.34103966065242));
#17450=CARTESIAN_POINT('Ctrl Pts',(5.0014764025242,-0.0870193504399114,
-5.34404184190018));
#17451=CARTESIAN_POINT('Ctrl Pts',(4.99610695876351,-0.142070106905666,
-5.34704402314794));
#17452=CARTESIAN_POINT('Ctrl Pts',(4.99073507095122,-0.197145921253763,
-5.35004757092196));
#17453=CARTESIAN_POINT('Ctrl Pts',(4.98223928547081,-0.251874063835189,
-5.35305111869598));
#17454=CARTESIAN_POINT('Ctrl Pts',(4.97069658460281,-0.305880884755777,
-5.35605466647));
#17455=CARTESIAN_POINT('Ctrl Pts',(4.95913209882948,-0.359989634461847,
-5.35906388293496));
#17456=CARTESIAN_POINT('Ctrl Pts',(4.94450934993391,-0.413373832349662,
-5.36207309939993));
#17457=CARTESIAN_POINT('Ctrl Pts',(4.92695560530715,-0.465673765818067,
-5.36508231586489));
#17458=CARTESIAN_POINT('Ctrl Pts',(4.91352627125848,-0.505685358341731,
-5.36738448978801));
#17459=CARTESIAN_POINT('Ctrl Pts',(4.89838251148219,-0.54506261862293,-5.36968666371113));
#17460=CARTESIAN_POINT('Ctrl Pts',(4.88159983959011,-0.583653497675247,
-5.37198883763425));
#17461=CARTESIAN_POINT('Ctrl Pts',(4.85965623178218,-0.634111679801032,
-5.37499896629549));
#17462=CARTESIAN_POINT('Ctrl Pts',(4.83481694889245,-0.683436639338129,
-5.37800909495673));
#17463=CARTESIAN_POINT('Ctrl Pts',(4.80722130622284,-0.731275078640029,
-5.38101922361797));
#17464=CARTESIAN_POINT('Ctrl Pts',(4.77967470878589,-0.779028495555822,
-5.38402400243241));
#17465=CARTESIAN_POINT('Ctrl Pts',(4.74938173507842,-0.825300181473497,
-5.38702878124686));
#17466=CARTESIAN_POINT('Ctrl Pts',(4.71652893559323,-0.869758575819491,
-5.3900335600613));
#17467=CARTESIAN_POINT('Ctrl Pts',(4.68370863851028,-0.91417298594985,-5.39303536614492));
#17468=CARTESIAN_POINT('Ctrl Pts',(4.64833384477347,-0.956777235594704,
-5.39603717222854));
#17469=CARTESIAN_POINT('Ctrl Pts',(4.61063502568417,-0.997267675972856,
-5.39903897831216));
#17470=CARTESIAN_POINT('Ctrl Pts',(4.57295861320917,-1.0377340505128,-5.40203900024676));
#17471=CARTESIAN_POINT('Ctrl Pts',(4.53296127237125,-1.07608872022572,-5.40503902218136));
#17472=CARTESIAN_POINT('Ctrl Pts',(4.49091299338967,-1.11206196557849,-5.40803904411596));
#17473=CARTESIAN_POINT('Ctrl Pts',(4.44887309908909,-1.1480280376487,-5.41103846782805));
#17474=CARTESIAN_POINT('Ctrl Pts',(4.40478347991244,-1.18161328530514,-5.41403789154014));
#17475=CARTESIAN_POINT('Ctrl Pts',(4.35894840650725,-1.21258722588824,-5.41703731525223));
#17476=CARTESIAN_POINT('Ctrl Pts',(4.3130711943908,-1.24358964252345,-5.42003949649999));
#17477=CARTESIAN_POINT('Ctrl Pts',(4.26544576059141,-1.2719756594282,-5.42304167774775));
#17478=CARTESIAN_POINT('Ctrl Pts',(4.21640542748126,-1.29755812299601,-5.42604385899551));
#17479=CARTESIAN_POINT('Ctrl Pts',(4.16734277230008,-1.32315223113336,-5.42904740676953));
#17480=CARTESIAN_POINT('Ctrl Pts',(4.1168644161577,-1.34594002441191,-5.43205095454355));
#17481=CARTESIAN_POINT('Ctrl Pts',(4.0653253637124,-1.36578181672806,-5.43505450231757));
#17482=CARTESIAN_POINT('Ctrl Pts',(4.01368903997931,-1.38566105708796,-5.43806371878253));
#17483=CARTESIAN_POINT('Ctrl Pts',(3.96098852492938,-1.40258302750694,-5.4410729352475));
#17484=CARTESIAN_POINT('Ctrl Pts',(3.90759462594989,-1.41645777229699,-5.44408215171247));
#17485=CARTESIAN_POINT('Ctrl Pts',(3.86674610497601,-1.42707252069326,-5.44638432563558));
#17486=CARTESIAN_POINT('Ctrl Pts',(3.82549209883954,-1.43590479475528,-5.4486864995587));
#17487=CARTESIAN_POINT('Ctrl Pts',(3.78400121299976,-1.44293476019596,-5.45098867348181));
#17488=CARTESIAN_POINT('Ctrl Pts',(3.72975122632739,-1.45212655072405,-5.45399880214305));
#17489=CARTESIAN_POINT('Ctrl Pts',(3.67486815857402,-1.45827394706616,-5.45700893080429));
#17490=CARTESIAN_POINT('Ctrl Pts',(3.61972402736092,-1.46130058908986,-5.46001905946553));
#17491=CARTESIAN_POINT('Ctrl Pts',(3.56467790280697,-1.46432185191788,-5.46302383827997));
#17492=CARTESIAN_POINT('Ctrl Pts',(3.50937215862868,-1.46423333870561,-5.46602861709442));
#17493=CARTESIAN_POINT('Ctrl Pts',(3.45418641618661,-1.46101012711558,-5.46903339590886));
#17494=CARTESIAN_POINT('Ctrl Pts',(3.39905527089387,-1.45779010435941,-5.47203520199248));
#17495=CARTESIAN_POINT('Ctrl Pts',(3.34404441678076,-1.45144155732333,-5.4750370080761));
#17496=CARTESIAN_POINT('Ctrl Pts',(3.28953409648797,-1.44199159942286,-5.47803881415972));
#17497=CARTESIAN_POINT('Ctrl Pts',(3.2350561748684,-1.43254725818537,-5.48103883609432));
#17498=CARTESIAN_POINT('Ctrl Pts',(3.18107871672722,-1.42000524975318,-5.48403885802892));
#17499=CARTESIAN_POINT('Ctrl Pts',(3.12797514102828,-1.40444432450707,-5.48703887996352));
#17500=CARTESIAN_POINT('Ctrl Pts',(3.07488215450339,-1.38888650220353,-5.49003830367561));
#17501=CARTESIAN_POINT('Ctrl Pts',(3.02266321087416,-1.37031110703868,-5.4930377273877));
#17502=CARTESIAN_POINT('Ctrl Pts',(2.97167759785829,-1.34884703904824,-5.49603715109979));
#17503=CARTESIAN_POINT('Ctrl Pts',(2.92064511095596,-1.32736323795612,-5.49903933234755));
#17504=CARTESIAN_POINT('Ctrl Pts',(2.87084870777818,-1.30298566361301,-5.5020415135953));
#17505=CARTESIAN_POINT('Ctrl Pts',(2.8226272605429,-1.27589122248039,-5.50504369484306));
#17506=CARTESIAN_POINT('Ctrl Pts',(2.77438386397531,-1.24878444855966,-5.50804724261708));
#17507=CARTESIAN_POINT('Ctrl Pts',(2.72771729818045,-1.21895862756092,-5.5110507903911));
#17508=CARTESIAN_POINT('Ctrl Pts',(2.68293852718109,-1.18663476150104,-5.51405433816511));
#17509=CARTESIAN_POINT('Ctrl Pts',(2.6380752437874,-1.15424988958383,-5.51706355463008));
#17510=CARTESIAN_POINT('Ctrl Pts',(2.59510728360013,-1.11935788811164,-5.52007277109505));
#17511=CARTESIAN_POINT('Ctrl Pts',(2.55431259462973,-1.08222016681602,-5.52308198756001));
#17512=CARTESIAN_POINT('Ctrl Pts',(2.52310298566911,-1.05380828800096,-5.52538416148313));
#17513=CARTESIAN_POINT('Ctrl Pts',(2.493164691434,-1.0240828674705,-5.52768633540625));
#17514=CARTESIAN_POINT('Ctrl Pts',(2.46460644903469,-0.993174279457856,
-5.52998850932937));
#17515=CARTESIAN_POINT('Ctrl Pts',(2.42770723493981,-0.95323825711789,-5.53296307643631));
#17516=CARTESIAN_POINT('Ctrl Pts',(2.39295012736766,-0.911149160200317,
-5.53593764354324));
#17517=CARTESIAN_POINT('Ctrl Pts',(2.36059970343556,-0.867168624489341,
-5.53891221065018));
#17518=CARTESIAN_POINT('Ctrl Pts',(2.32829617987034,-0.823251850021937,
-5.54188246534721));
#17519=CARTESIAN_POINT('Ctrl Pts',(2.2983927516882,-0.77744949631226,-5.54485272004424));
#17520=CARTESIAN_POINT('Ctrl Pts',(2.27111569915588,-0.730058345952124,
-5.54782297474127));
#17521=CARTESIAN_POINT('Ctrl Pts',(2.24386679721609,-0.682716104430726,
-5.55079016406202));
#17522=CARTESIAN_POINT('Ctrl Pts',(2.21923917147809,-0.633788780753086,
-5.55375735338278));
#17523=CARTESIAN_POINT('Ctrl Pts',(2.19741602064055,-0.583602353875314,
-5.55672454270353));
#17524=CARTESIAN_POINT('Ctrl Pts',(2.17559980709139,-0.533431880592808,
-5.55969078879441));
#17525=CARTESIAN_POINT('Ctrl Pts',(2.15658653224062,-0.482003586647679,
-5.56265703488528));
#17526=CARTESIAN_POINT('Ctrl Pts',(2.14051259108434,-0.429666355127702,
-5.56562328097615));
#17527=CARTESIAN_POINT('Ctrl Pts',(2.1244421866726,-0.377340639353387,-5.56858887440477));
#17528=CARTESIAN_POINT('Ctrl Pts',(2.11130998532965,-0.324106902664438,
-5.57155446783338));
#17529=CARTESIAN_POINT('Ctrl Pts',(2.10120260055936,-0.270329502740076,
-5.574520061262));
#17530=CARTESIAN_POINT('Ctrl Pts',(2.09108705510497,-0.2165086830407,-5.57748804910537));
#17531=CARTESIAN_POINT('Ctrl Pts',(2.08400129502276,-0.162143858228026,
-5.58045603694873));
#17532=CARTESIAN_POINT('Ctrl Pts',(2.07998051047228,-0.107608087049964,
-5.5834240247921));
#17533=CARTESIAN_POINT('Ctrl Pts',(2.07730678194287,-0.0713430632861772,
-5.58539766791376));
#17534=CARTESIAN_POINT('Ctrl Pts',(2.07598729440754,-0.0350025971489008,
-5.58737131103543));
#17535=CARTESIAN_POINT('Ctrl Pts',(2.07601963090622,0.00130348536077232,
-5.58934495415709));
#17536=CARTESIAN_POINT('Origin',(3.53951905042299,8.32667268468867E-16,
0.));
#17537=CARTESIAN_POINT('',(2.07398455785054,-0.000602649354525531,-6.16065504584291));
#17538=CARTESIAN_POINT('',(2.07406181082671,-0.00067065111815213,-6.08934495415709));
#17539=CARTESIAN_POINT('',(2.07601905042299,1.01189432752408E-15,0.));
#17540=CARTESIAN_POINT('Ctrl Pts',(2.07398455785054,-0.000602649354525531,
-6.16065504584291));
#17541=CARTESIAN_POINT('Ctrl Pts',(2.07380392810973,-0.0350793873735884,
-6.15877304002329));
#17542=CARTESIAN_POINT('Ctrl Pts',(2.09047948666901,-0.551781602873419,
-6.1305577555879));
#17543=CARTESIAN_POINT('Ctrl Pts',(2.700819254767,-1.50963595324291,-6.07600919253644));
#17544=CARTESIAN_POINT('Ctrl Pts',(4.34561751406752,-1.52729280934158,-5.99700935668896));
#17545=CARTESIAN_POINT('Ctrl Pts',(5.25911691828729,-0.159377637682488,
-5.91800952084136));
#17546=CARTESIAN_POINT('Ctrl Pts',(4.61258363582657,1.35312617819235,-5.83900968499382));
#17547=CARTESIAN_POINT('Ctrl Pts',(2.9925577366135,1.6380633015096,-5.76000984914625));
#17548=CARTESIAN_POINT('Ctrl Pts',(2.1468259724859,0.734152894754073,-5.70055836087874));
#17549=CARTESIAN_POINT('Ctrl Pts',(2.07527553244525,0.126122538347039,-5.66744015122709));
#17550=CARTESIAN_POINT('Ctrl Pts',(2.07637422736057,0.00130108074448911,
-5.66065522019129));
#17551=CARTESIAN_POINT('Ctrl Pts',(2.0762466562035,0.00130536003002751,
-5.58934506707585));
#17552=CARTESIAN_POINT('Ctrl Pts',(2.07517374542601,0.121736799127538,-5.59589282644287));
#17553=CARTESIAN_POINT('Ctrl Pts',(2.14365852969769,0.725306357571781,-5.62877386442578));
#17554=CARTESIAN_POINT('Ctrl Pts',(2.97793235114716,1.6331069724431,-5.68798818102447));
#17555=CARTESIAN_POINT('Ctrl Pts',(4.60044132363883,1.36266721338727,-5.76698801687208));
#17556=CARTESIAN_POINT('Ctrl Pts',(5.26047328032698,-0.143994940263915,
-5.84598785271962));
#17557=CARTESIAN_POINT('Ctrl Pts',(4.35924204804306,-1.52002375357057,-5.92498768856719));
#17558=CARTESIAN_POINT('Ctrl Pts',(2.71435167648648,-1.51707508358577,-6.00398752441476));
#17559=CARTESIAN_POINT('Ctrl Pts',(2.09278029747244,-0.560575463951796,
-6.05877327961139));
#17560=CARTESIAN_POINT('Ctrl Pts',(2.0738392940555,-0.0394979728212691,
-6.08722575619216));
#17561=CARTESIAN_POINT('Ctrl Pts',(2.07406181082671,-0.00067065111815213,
-6.08934495415709));
#17562=CARTESIAN_POINT('Origin',(3.53951905042299,8.32667268468867E-16,
0.));
#17563=CARTESIAN_POINT('',(2.0779924908381,-0.000733103778174787,-6.66065504584291));
#17564=CARTESIAN_POINT('',(2.07609699915992,-0.000674750808749472,-6.58934493582576));
#17565=CARTESIAN_POINT('',(2.07601905042299,1.01189432752408E-15,0.));
#17566=CARTESIAN_POINT('Ctrl Pts',(2.0779924908381,-0.000733103778174787,
-6.66065504584291));
#17567=CARTESIAN_POINT('Ctrl Pts',(2.07710078135123,-0.195345291847198,
-6.65010604505175));
#17568=CARTESIAN_POINT('Ctrl Pts',(2.2035492442434,-0.874652820981799,-6.61322376564476));
#17569=CARTESIAN_POINT('Ctrl Pts',(3.22971693546565,-1.69895282692743,-6.55000820762186));
#17570=CARTESIAN_POINT('Ctrl Pts',(4.79316310733731,-1.18776876416246,-6.47100837177433));
#17571=CARTESIAN_POINT('Ctrl Pts',(5.21929354813173,0.400968446893448,-6.39200853592674));
#17572=CARTESIAN_POINT('Ctrl Pts',(4.12151937631297,1.62594393483315,-6.31300870007919));
#17573=CARTESIAN_POINT('Ctrl Pts',(2.53448049511705,1.38180827662175,-6.23589087005124));
#17574=CARTESIAN_POINT('Ctrl Pts',(2.07633132374345,0.447323769173315,-6.18510631863914));
#17575=CARTESIAN_POINT('Ctrl Pts',(2.07398455785054,-0.000602649354525531,
-6.16065504584291));
#17576=CARTESIAN_POINT('Ctrl Pts',(2.07406181082671,-0.00067065111815213,
-6.08934495415709));
#17577=CARTESIAN_POINT('Ctrl Pts',(2.07660430054847,0.442972611446132,-6.11355903480801));
#17578=CARTESIAN_POINT('Ctrl Pts',(2.52703917513374,1.37356066127882,-6.16410639407482));
#17579=CARTESIAN_POINT('Ctrl Pts',(4.10695721513758,1.63108305535657,-6.24098703195743));
#17580=CARTESIAN_POINT('Ctrl Pts',(5.21564099217811,0.415972644068219,-6.31998686780501));
#17581=CARTESIAN_POINT('Ctrl Pts',(4.80373378404372,-1.1765114158147,-6.39898670365256));
#17582=CARTESIAN_POINT('Ctrl Pts',(3.24492104393115,-1.70165508221173,-6.47798653950012));
#17583=CARTESIAN_POINT('Ctrl Pts',(2.20754846303831,-0.883507584733025,
-6.54143912965251));
#17584=CARTESIAN_POINT('Ctrl Pts',(2.07722212510776,-0.199689226725607,
-6.57855844118906));
#17585=CARTESIAN_POINT('Ctrl Pts',(2.0780563998582,-0.000682366665369591,
-6.58934447410974));
#17586=CARTESIAN_POINT('Origin',(3.53951905042299,8.32667268468867E-16,
0.));
#17587=CARTESIAN_POINT('',(2.0760196139518,0.00128430857734538,-7.16065506268004));
#17588=CARTESIAN_POINT('',(2.07601962331082,0.00129492948150966,-7.08934495420698));
#17589=CARTESIAN_POINT('',(2.07601905042299,1.01189432752408E-15,0.));
#17590=CARTESIAN_POINT('Ctrl Pts',(2.07655027563832,0.00128353304686551,
-7.16065504584291));
#17591=CARTESIAN_POINT('Ctrl Pts',(2.07959752967489,-0.352338916278862,
-7.14143905008021));
#17592=CARTESIAN_POINT('Ctrl Pts',(2.38543525504794,-1.19528620059351,-7.09588977570168));
#17593=CARTESIAN_POINT('Ctrl Pts',(3.79139519143046,-1.70850123445903,-7.02400722270725));
#17594=CARTESIAN_POINT('Ctrl Pts',(5.10805894974804,-0.72256532077177,-6.94500738685969));
#17595=CARTESIAN_POINT('Ctrl Pts',(5.00173099643442,0.918887524944285,-6.86600755101213));
#17596=CARTESIAN_POINT('Ctrl Pts',(3.56887288554054,1.72671839363593,-6.78700771516457));
#17597=CARTESIAN_POINT('Ctrl Pts',(2.30427301763542,1.06936233072511,-6.71855688010815));
#17598=CARTESIAN_POINT('Ctrl Pts',(2.0793267395085,0.29046157004619,-6.67643932366761));
#17599=CARTESIAN_POINT('Ctrl Pts',(2.0779924908381,-0.000733103778174787,
-6.66065504584291));
#17600=CARTESIAN_POINT('Ctrl Pts',(2.0760192058315,-0.000674448439338396,
-6.58934495415709));
#17601=CARTESIAN_POINT('Ctrl Pts',(2.07599326113436,0.0556234952179208,
-6.59239202230984));
#17602=CARTESIAN_POINT('Ctrl Pts',(2.07922016311911,0.111913354676178,-6.59543909046259));
#17603=CARTESIAN_POINT('Ctrl Pts',(2.08567083734158,0.167802334071928,-6.59848615861535));
#17604=CARTESIAN_POINT('Ctrl Pts',(2.09228650335208,0.225120810962692,-6.601611162997));
#17605=CARTESIAN_POINT('Ctrl Pts',(2.10229309861054,0.282017059273543,-6.60473616737866));
#17606=CARTESIAN_POINT('Ctrl Pts',(2.11560311694291,0.338076417961319,-6.60786117176032));
#17607=CARTESIAN_POINT('Ctrl Pts',(2.1286086080415,0.392853163732831,-6.61091467744707));
#17608=CARTESIAN_POINT('Ctrl Pts',(2.14476771993851,0.44683044349619,-6.61396818313383));
#17609=CARTESIAN_POINT('Ctrl Pts',(2.16394835432136,0.499637378532147,-6.61702168882059));
#17610=CARTESIAN_POINT('Ctrl Pts',(2.18380266863138,0.55429904743349,-6.6201824425497));
#17611=CARTESIAN_POINT('Ctrl Pts',(2.2068945099148,0.607706069216808,-6.62334319627881));
#17612=CARTESIAN_POINT('Ctrl Pts',(2.23302458651292,0.659472869625687,-6.62650395000792));
#17613=CARTESIAN_POINT('Ctrl Pts',(2.25915466311103,0.71123967003456,-6.62966470373703));
#17614=CARTESIAN_POINT('Ctrl Pts',(2.28832261198184,0.761365777376941,-6.63282545746614));
#17615=CARTESIAN_POINT('Ctrl Pts',(2.32028027386689,0.809499262348018,-6.63598621119525));
#17616=CARTESIAN_POINT('Ctrl Pts',(2.35071499995783,0.855338956007899,-6.63899633985649));
#17617=CARTESIAN_POINT('Ctrl Pts',(2.38380241792489,0.899556196763958,-6.64200646851773));
#17618=CARTESIAN_POINT('Ctrl Pts',(2.41934353833162,0.941827517176493,-6.64501659717896));
#17619=CARTESIAN_POINT('Ctrl Pts',(2.45482149215298,0.984023709541885,-6.64802137599341));
#17620=CARTESIAN_POINT('Ctrl Pts',(2.4927441570204,1.02428044392336,-6.65102615480785));
#17621=CARTESIAN_POINT('Ctrl Pts',(2.53286984092293,1.06230392026618,-6.6540309336223));
#17622=CARTESIAN_POINT('Ctrl Pts',(2.572955827109,1.10028977867865,-6.65703273970592));
#17623=CARTESIAN_POINT('Ctrl Pts',(2.61524013334466,1.13604639437272,-6.66003454578954));
#17624=CARTESIAN_POINT('Ctrl Pts',(2.65944270880389,1.16931513413722,-6.66303635187316));
#17625=CARTESIAN_POINT('Ctrl Pts',(2.7036190120858,1.2025641003428,-6.66603637380776));
#17626=CARTESIAN_POINT('Ctrl Pts',(2.74971090364499,1.23332780453115,-6.66903639574236));
#17627=CARTESIAN_POINT('Ctrl Pts',(2.79740536080833,1.26138793465235,-6.67203641767696));
#17628=CARTESIAN_POINT('Ctrl Pts',(2.84509030740863,1.28944246941399,-6.67503584138905));
#17629=CARTESIAN_POINT('Ctrl Pts',(2.89437673005101,1.31479423310812,-6.67803526510114));
#17630=CARTESIAN_POINT('Ctrl Pts',(2.94492472065994,1.3372695438892,-6.68103468881323));
#17631=CARTESIAN_POINT('Ctrl Pts',(2.99551918282488,1.35976551746323,-6.68403687006099));
#17632=CARTESIAN_POINT('Ctrl Pts',(3.04737704654229,1.37937953976781,-6.68703905130875));
#17633=CARTESIAN_POINT('Ctrl Pts',(3.10013738245228,1.39598567322565,-6.69004123255651));
#17634=CARTESIAN_POINT('Ctrl Pts',(3.15292173369599,1.41259936542682,-6.69304478033053));
#17635=CARTESIAN_POINT('Ctrl Pts',(3.20660886317306,1.42620230958812,-6.69604832810455));
#17636=CARTESIAN_POINT('Ctrl Pts',(3.26082480015785,1.43671909741228,-6.69905187587857));
#17637=CARTESIAN_POINT('Ctrl Pts',(3.31514306059952,1.44725573390355,-6.70206109234354));
#17638=CARTESIAN_POINT('Ctrl Pts',(3.36999159767024,1.45469450736379,-6.7050703088085));
#17639=CARTESIAN_POINT('Ctrl Pts',(3.42498958410318,1.45901173790498,-6.70807952527347));
#17640=CARTESIAN_POINT('Ctrl Pts',(3.4670652977196,1.46231459620304,-6.71038169919659));
#17641=CARTESIAN_POINT('Ctrl Pts',(3.50922832371918,1.46379152747159,-6.7126838731197));
#17642=CARTESIAN_POINT('Ctrl Pts',(3.55130918739314,1.46345250782874,-6.71498604704281));
#17643=CARTESIAN_POINT('Ctrl Pts',(3.60633057937528,1.46300923430651,-6.71799617570406));
#17644=CARTESIAN_POINT('Ctrl Pts',(3.66144254381316,1.45945775804877,-6.72100630436529));
#17645=CARTESIAN_POINT('Ctrl Pts',(3.71626544097366,1.45278799672468,-6.72401643302654));
#17646=CARTESIAN_POINT('Ctrl Pts',(3.77099090239841,1.44613008944581,-6.72702121184098));
#17647=CARTESIAN_POINT('Ctrl Pts',(3.82542779608369,1.43636495864267,-6.73002599065542));
#17648=CARTESIAN_POINT('Ctrl Pts',(3.87919799701067,1.4235344966825,-6.73303076946987));
#17649=CARTESIAN_POINT('Ctrl Pts',(3.93291500123211,1.41071672833877,-6.73603257555349));
#17650=CARTESIAN_POINT('Ctrl Pts',(3.98596610812677,1.39483975832007,-6.73903438163711));
#17651=CARTESIAN_POINT('Ctrl Pts',(4.03798168674773,1.3759968205589,-6.74203618772072));
#17652=CARTESIAN_POINT('Ctrl Pts',(4.08996634946638,1.35716508225832,-6.74503620965532));
#17653=CARTESIAN_POINT('Ctrl Pts',(4.14091620827475,1.33537104981138,-6.74803623158992));
#17654=CARTESIAN_POINT('Ctrl Pts',(4.19047738659582,1.31075760328411,-6.75103625352452));
#17655=CARTESIAN_POINT('Ctrl Pts',(4.24002868211836,1.28614906482685,-6.75403567723661));
#17656=CARTESIAN_POINT('Ctrl Pts',(4.28819137435497,1.25872246358266,-6.7570351009487));
#17657=CARTESIAN_POINT('Ctrl Pts',(4.33463427564759,1.22866758263415,-6.76003452466079));
#17658=CARTESIAN_POINT('Ctrl Pts',(4.38111987446117,1.19858507057574,-6.76303670590855));
#17659=CARTESIAN_POINT('Ctrl Pts',(4.42588207917347,1.16586973885509,-6.76603888715631));
#17660=CARTESIAN_POINT('Ctrl Pts',(4.46861820328876,1.13075506372694,-6.76904106840407));
#17661=CARTESIAN_POINT('Ctrl Pts',(4.51137377993907,1.09562440517816,-6.77204461617809));
#17662=CARTESIAN_POINT('Ctrl Pts',(4.55210104856066,1.05809258465259,-6.77504816395211));
#17663=CARTESIAN_POINT('Ctrl Pts',(4.5905325165387,1.01843160989997,-6.77805171172613));
#17664=CARTESIAN_POINT('Ctrl Pts',(4.62903651744478,0.978695781732188,-6.78106092819109));
#17665=CARTESIAN_POINT('Ctrl Pts',(4.66523571575824,0.936823172417134,-6.78407014465606));
#17666=CARTESIAN_POINT('Ctrl Pts',(4.69890219641194,0.893119796442098,-6.78707936112102));
#17667=CARTESIAN_POINT('Ctrl Pts',(4.72465843387322,0.859684922715576,-6.78938153504414));
#17668=CARTESIAN_POINT('Ctrl Pts',(4.74893311544962,0.825179243157287,-6.79168370896726));
#17669=CARTESIAN_POINT('Ctrl Pts',(4.77164199609297,0.789750148308652,-6.79398588289037));
#17670=CARTESIAN_POINT('Ctrl Pts',(4.80133421517459,0.74342604882393,-6.79699601155161));
#17671=CARTESIAN_POINT('Ctrl Pts',(4.82847271924862,0.695327782696866,-6.80000614021285));
#17672=CARTESIAN_POINT('Ctrl Pts',(4.85284163043178,0.645767799475205,-6.80301626887409));
#17673=CARTESIAN_POINT('Ctrl Pts',(4.87716723119335,0.596295898308248,-6.80602104768853));
#17674=CARTESIAN_POINT('Ctrl Pts',(4.89873277634878,0.545367905653401,-6.80902582650297));
#17675=CARTESIAN_POINT('Ctrl Pts',(4.91736674585716,0.493323401215406,-6.81203060531742));
#17676=CARTESIAN_POINT('Ctrl Pts',(4.93598228013988,0.441330386192138,-6.81503241140104));
#17677=CARTESIAN_POINT('Ctrl Pts',(4.95167180700242,0.388223542315351,-6.81803421748465));
#17678=CARTESIAN_POINT('Ctrl Pts',(4.96431144747405,0.334363388105644,-6.82103602356827));
#17679=CARTESIAN_POINT('Ctrl Pts',(4.97694357546769,0.280535246137471,-6.82403604550287));
#17680=CARTESIAN_POINT('Ctrl Pts',(4.98652928959537,0.225955194401018,-6.82703606743747));
#17681=CARTESIAN_POINT('Ctrl Pts',(4.99299489898523,0.170997683160591,-6.83003608937207));
#17682=CARTESIAN_POINT('Ctrl Pts',(4.99945921909348,0.116051130780102,-6.83303551308416));
#17683=CARTESIAN_POINT('Ctrl Pts',(5.00280460839102,0.0607277925788181,
-6.83603493679625));
#17684=CARTESIAN_POINT('Ctrl Pts',(5.0030090556809,0.00540874386492178,
-6.83903436050834));
#17685=CARTESIAN_POINT('Ctrl Pts',(5.00321369093046,-0.0499611627018728,
-6.8420365417561));
#17686=CARTESIAN_POINT('Ctrl Pts',(5.0002716130844,-0.105326242655259,-6.84503872300386));
#17687=CARTESIAN_POINT('Ctrl Pts',(4.99421297807659,-0.160305417399837,
-6.84804090425162));
#17688=CARTESIAN_POINT('Ctrl Pts',(4.98815158531262,-0.215309617444318,
-6.85104445202564));
#17689=CARTESIAN_POINT('Ctrl Pts',(4.97897089522622,-0.269927040405111,
-6.85404799979966));
#17690=CARTESIAN_POINT('Ctrl Pts',(4.96675256471366,-0.323785030051597,
-6.85705154757368));
#17691=CARTESIAN_POINT('Ctrl Pts',(4.95451117415852,-0.377744667589602,
-6.86006076403864));
#17692=CARTESIAN_POINT('Ctrl Pts',(4.93922083679664,-0.430941499757968,
-6.86306998050361));
#17693=CARTESIAN_POINT('Ctrl Pts',(4.92101331609888,-0.483017436439539,
-6.86607919696858));
#17694=CARTESIAN_POINT('Ctrl Pts',(4.90708381656203,-0.522857662241221,
-6.8683813708917));
#17695=CARTESIAN_POINT('Ctrl Pts',(4.89144797200305,-0.562042129219201,
-6.87068354481482));
#17696=CARTESIAN_POINT('Ctrl Pts',(4.87418319480349,-0.600419746265117,
-6.87298571873794));
#17697=CARTESIAN_POINT('Ctrl Pts',(4.85160922671344,-0.650599084958741,
-6.87599584739917));
#17698=CARTESIAN_POINT('Ctrl Pts',(4.82615400645715,-0.699609016294218,
-6.87900597606041));
#17699=CARTESIAN_POINT('Ctrl Pts',(4.79796126411181,-0.747098015528067,
-6.88201610472165));
#17700=CARTESIAN_POINT('Ctrl Pts',(4.76981862821346,-0.794502613429359,
-6.8850208835361));
#17701=CARTESIAN_POINT('Ctrl Pts',(4.73894839295802,-0.840391193152233,
-6.88802566235054));
#17702=CARTESIAN_POINT('Ctrl Pts',(4.70554124761026,-0.884434557028712,
-6.89103044116499));
#17703=CARTESIAN_POINT('Ctrl Pts',(4.67216715309817,-0.92843434729342,-6.89403224724861));
#17704=CARTESIAN_POINT('Ctrl Pts',(4.63626143797683,-0.970592119309363,
-6.89703405333222));
#17705=CARTESIAN_POINT('Ctrl Pts',(4.59805835922658,-1.01060713520023,-6.90003585941584));
#17706=CARTESIAN_POINT('Ctrl Pts',(4.55987798680168,-1.05059836782546,-6.90303588135044));
#17707=CARTESIAN_POINT('Ctrl Pts',(4.51940332113245,-1.08844898739569,-6.90603590328504));
#17708=CARTESIAN_POINT('Ctrl Pts',(4.47690770998966,-1.12389267766802,-6.90903592521963));
#17709=CARTESIAN_POINT('Ctrl Pts',(4.43442057272858,-1.15932930025429,-6.91203534893173));
#17710=CARTESIAN_POINT('Ctrl Pts',(4.38991369565091,-1.19235960864036,-6.91503477264382));
#17711=CARTESIAN_POINT('Ctrl Pts',(4.34369421275151,-1.22275694980397,-6.91803419635591));
#17712=CARTESIAN_POINT('Ctrl Pts',(4.297432237732,-1.25318223692003,-6.92103637760367));
#17713=CARTESIAN_POINT('Ctrl Pts',(4.24945495344846,-1.28096942988862,-6.92403855885143));
#17714=CARTESIAN_POINT('Ctrl Pts',(4.20009800056435,-1.30593556526734,-6.92704074009919));
#17715=CARTESIAN_POINT('Ctrl Pts',(4.15071858149094,-1.33091306467668,-6.9300442878732));
#17716=CARTESIAN_POINT('Ctrl Pts',(4.09995872682262,-1.35306673514884,-6.93304783564722));
#17717=CARTESIAN_POINT('Ctrl Pts',(4.04817516318935,-1.37226134863058,-6.93605138342124));
#17718=CARTESIAN_POINT('Ctrl Pts',(3.99629386679455,-1.39149218871494,-6.93906059988621));
#17719=CARTESIAN_POINT('Ctrl Pts',(3.94338550785993,-1.40775265993304,-6.94206981635118));
#17720=CARTESIAN_POINT('Ctrl Pts',(3.88982199153912,-1.4209574587036,-6.94507903281614));
#17721=CARTESIAN_POINT('Ctrl Pts',(3.84884370634756,-1.43105967093844,-6.94738120673926));
#17722=CARTESIAN_POINT('Ctrl Pts',(3.8074822965976,-1.43937446924747,-6.94968338066238));
#17723=CARTESIAN_POINT('Ctrl Pts',(3.76590660298021,-1.44588413299516,-6.95198555458551));
#17724=CARTESIAN_POINT('Ctrl Pts',(3.71154572880312,-1.45439562086544,-6.95499568324674));
#17725=CARTESIAN_POINT('Ctrl Pts',(3.65658995988772,-1.45985502291367,-6.95800581190798));
#17726=CARTESIAN_POINT('Ctrl Pts',(3.60141224121718,-1.46219064520784,-6.96101594056922));
#17727=CARTESIAN_POINT('Ctrl Pts',(3.54633258890015,-1.46452211644307,-6.96402071938366));
#17728=CARTESIAN_POINT('Ctrl Pts',(3.49103229302684,-1.46374080342766,-6.96702549819811));
#17729=CARTESIAN_POINT('Ctrl Pts',(3.43589125736956,-1.45982654123936,-6.97003027701255));
#17730=CARTESIAN_POINT('Ctrl Pts',(3.38080477463164,-1.45591615156501,-6.97303208309617));
#17731=CARTESIAN_POINT('Ctrl Pts',(3.32587776418845,-1.44887898995699,-6.97603388917979));
#17732=CARTESIAN_POINT('Ctrl Pts',(3.2714900991996,-1.43874693094585,-6.97903569526341));
#17733=CARTESIAN_POINT('Ctrl Pts',(3.2171347599828,-1.42862089401029,-6.98203571719801));
#17734=CARTESIAN_POINT('Ctrl Pts',(3.16331864898754,-1.41540370216639,-6.9850357391326));
#17735=CARTESIAN_POINT('Ctrl Pts',(3.11041416938353,-1.39917877737911,-6.9880357610672));
#17736=CARTESIAN_POINT('Ctrl Pts',(3.05752023925256,-1.38295708793992,-6.99103518477929));
#17737=CARTESIAN_POINT('Ctrl Pts',(3.00553808411818,-1.36372901141447,-6.99403460849138));
#17738=CARTESIAN_POINT('Ctrl Pts',(2.95482534879553,-1.34162793846773,-6.99703403220347));
#17739=CARTESIAN_POINT('Ctrl Pts',(2.90406599045795,-1.31950654678553,-7.00003621345123));
#17740=CARTESIAN_POINT('Ctrl Pts',(2.85457886871953,-1.29450709314464,-7.00303839469899));
#17741=CARTESIAN_POINT('Ctrl Pts',(2.80670061312826,-1.26681071512713,-7.00604057594674));
#17742=CARTESIAN_POINT('Ctrl Pts',(2.7588005644179,-1.23910173033318,-7.00904412372076));
#17743=CARTESIAN_POINT('Ctrl Pts',(2.71251128384996,-1.20869366453091,-7.01204767149478));
#17744=CARTESIAN_POINT('Ctrl Pts',(2.66814094258865,-1.17581139779603,-7.01505121926879));
#17745=CARTESIAN_POINT('Ctrl Pts',(2.6236868597754,-1.14286707131651,-7.01806043573376));
#17746=CARTESIAN_POINT('Ctrl Pts',(2.58115935788908,-1.10743955443064,-7.02106965219873));
#17747=CARTESIAN_POINT('Ctrl Pts',(2.54083308849079,-1.06979371817166,-7.02407886866369));
#17748=CARTESIAN_POINT('Ctrl Pts',(2.50998183970012,-1.04099311058539,-7.02638104258681));
#17749=CARTESIAN_POINT('Ctrl Pts',(2.48041826042216,-1.01089498991809,-7.02868321650994));
#17750=CARTESIAN_POINT('Ctrl Pts',(2.45224944605684,-0.979631082306741,
-7.03098539043306));
#17751=CARTESIAN_POINT('Ctrl Pts',(2.41581120538601,-0.939189132032269,
-7.03396340599272));
#17752=CARTESIAN_POINT('Ctrl Pts',(2.3815476665173,-0.896617035648219,-7.03694142155237));
#17753=CARTESIAN_POINT('Ctrl Pts',(2.34972042974617,-0.852180434083961,
-7.03991943711203));
#17754=CARTESIAN_POINT('Ctrl Pts',(2.31793967594817,-0.807808731190343,
-7.04289310334603));
#17755=CARTESIAN_POINT('Ctrl Pts',(2.28858849220199,-0.761578348565858,
-7.04586676958003));
#17756=CARTESIAN_POINT('Ctrl Pts',(2.26188971872353,-0.71378956337369,-7.04884043581404));
#17757=CARTESIAN_POINT('Ctrl Pts',(2.23521883903141,-0.666050705949342,
-7.05181099528321));
#17758=CARTESIAN_POINT('Ctrl Pts',(2.21119514271729,-0.616757140291217,
-7.05478155475238));
#17759=CARTESIAN_POINT('Ctrl Pts',(2.18999801491327,-0.566237781075023,
-7.05775211422155));
#17760=CARTESIAN_POINT('Ctrl Pts',(2.1688087009087,-0.515737044577197,-7.06072157866708));
#17761=CARTESIAN_POINT('Ctrl Pts',(2.15044411167435,-0.46401190207085,-7.06369104311261));
#17762=CARTESIAN_POINT('Ctrl Pts',(2.13503653174213,-0.41141354464803,-7.06666050755815));
#17763=CARTESIAN_POINT('Ctrl Pts',(2.11963252895492,-0.358827398873818,
-7.06962928258945));
#17764=CARTESIAN_POINT('Ctrl Pts',(2.10718431885292,-0.305368960812494,
-7.07259805762075));
#17765=CARTESIAN_POINT('Ctrl Pts',(2.09777422802999,-0.251404290144346,
-7.07556683265205));
#17766=CARTESIAN_POINT('Ctrl Pts',(2.08835749173144,-0.197401509227279,
-7.07853770425419));
#17767=CARTESIAN_POINT('Ctrl Pts',(2.08198324268079,-0.142892316244514,
-7.08150857585634));
#17768=CARTESIAN_POINT('Ctrl Pts',(2.07868228623638,-0.0882507699727326,
-7.08447944745849));
#17769=CARTESIAN_POINT('Ctrl Pts',(2.07688025327064,-0.0584212737832516,
-7.08610128302469));
#17770=CARTESIAN_POINT('Ctrl Pts',(2.07599321388797,-0.0285524121464094,
-7.08772311859089));
#17771=CARTESIAN_POINT('Ctrl Pts',(2.07601962331001,0.00129492856329364,
-7.08934495415709));
#17772=CARTESIAN_POINT('Origin',(3.53951905042299,8.32667268468867E-16,
0.));
#17773=CARTESIAN_POINT('',(2.07589476394848,-0.00050215083052111,-7.6606550766331));
#17774=CARTESIAN_POINT('',(2.07592822643732,-0.000573461297524445,-7.5893449794238));
#17775=CARTESIAN_POINT('',(2.07601905042299,1.01189432752408E-15,0.));
#17776=CARTESIAN_POINT('Ctrl Pts',(2.07601913675002,-0.000502672062860379,
-7.66065504584291));
#17777=CARTESIAN_POINT('Ctrl Pts',(2.07602887184672,-0.0288458290411398,
-7.65910533372452));
#17778=CARTESIAN_POINT('Ctrl Pts',(2.07686192127292,-0.0571737031003173,
-7.65755562160613));
#17779=CARTESIAN_POINT('Ctrl Pts',(2.07851596390768,-0.0854530935234271,
-7.65600590948774));
#17780=CARTESIAN_POINT('Ctrl Pts',(2.08172874199899,-0.140382394665887,
-7.65299578082649));
#17781=CARTESIAN_POINT('Ctrl Pts',(2.08805034112436,-0.195245670108624,
-7.64998565216525));
#17782=CARTESIAN_POINT('Ctrl Pts',(2.09747171776502,-0.249663253952273,
-7.64697552350401));
#17783=CARTESIAN_POINT('Ctrl Pts',(2.10687634996474,-0.303984122416255,
-7.64397074468956));
#17784=CARTESIAN_POINT('Ctrl Pts',(2.1193697373145,-0.357860355081879,-7.64096596587511));
#17785=CARTESIAN_POINT('Ctrl Pts',(2.1348910037667,-0.410916415523307,-7.63796118706066));
#17786=CARTESIAN_POINT('Ctrl Pts',(2.15039691449719,-0.463919985782878,
-7.63495938097704));
#17787=CARTESIAN_POINT('Ctrl Pts',(2.16892462266722,-0.516104486831484,
-7.63195757489342));
#17788=CARTESIAN_POINT('Ctrl Pts',(2.19036240340789,-0.56710545034849,-7.6289557688098));
#17789=CARTESIAN_POINT('Ctrl Pts',(2.21178744242093,-0.618076101008329,
-7.6259557468752));
#17790=CARTESIAN_POINT('Ctrl Pts',(2.23611892153535,-0.667864122529575,
-7.6229557249406));
#17791=CARTESIAN_POINT('Ctrl Pts',(2.26319632586426,-0.716123280430809,
-7.619955703006));
#17792=CARTESIAN_POINT('Ctrl Pts',(2.29026833079506,-0.764372815164213,
-7.61695627929391));
#17793=CARTESIAN_POINT('Ctrl Pts',(2.32008491524729,-0.811093631412306,
-7.61395685558183));
#17794=CARTESIAN_POINT('Ctrl Pts',(2.35243986307617,-0.855964516185112,
-7.61095743186974));
#17795=CARTESIAN_POINT('Ctrl Pts',(2.38482455659332,-0.900876653237421,
-7.60795525062198));
#17796=CARTESIAN_POINT('Ctrl Pts',(2.4197519662859,-0.943935031661007,-7.60495306937423));
#17797=CARTESIAN_POINT('Ctrl Pts',(2.4569736731441,-0.984849103229583,-7.60195088812647));
#17798=CARTESIAN_POINT('Ctrl Pts',(2.49421232249701,-1.02578179797531,-7.59894734035245));
#17799=CARTESIAN_POINT('Ctrl Pts',(2.53374697313804,-1.06456786970263,-7.59594379257843));
#17800=CARTESIAN_POINT('Ctrl Pts',(2.57529249527056,-1.10095385931422,-7.59294024480442));
#17801=CARTESIAN_POINT('Ctrl Pts',(2.61691642758427,-1.13740852135769,-7.58993102833945));
#17802=CARTESIAN_POINT('Ctrl Pts',(2.66055839543228,-1.17145372677265,-7.58692181187449));
#17803=CARTESIAN_POINT('Ctrl Pts',(2.70590129794752,-1.20287725589844,-7.58391259540953));
#17804=CARTESIAN_POINT('Ctrl Pts',(2.74059047667024,-1.22691754351735,-7.58161042148642));
#17805=CARTESIAN_POINT('Ctrl Pts',(2.77627451397957,-1.24942424404648,-7.57930824756331));
#17806=CARTESIAN_POINT('Ctrl Pts',(2.81280196490454,-1.27032063968731,-7.57700607364021));
#17807=CARTESIAN_POINT('Ctrl Pts',(2.86056218225717,-1.29764300608354,-7.57399594497897));
#17808=CARTESIAN_POINT('Ctrl Pts',(2.90996574891832,-1.32232557501311,-7.57098581631774));
#17809=CARTESIAN_POINT('Ctrl Pts',(2.96068974313619,-1.34416847270939,-7.5679756876565));
#17810=CARTESIAN_POINT('Ctrl Pts',(3.01132358652386,-1.36597254942179,-7.56497090884205));
#17811=CARTESIAN_POINT('Ctrl Pts',(3.06327271915266,-1.38494676331381,-7.56196613002761));
#17812=CARTESIAN_POINT('Ctrl Pts',(3.11618935672575,-1.4009369080848,-7.55896135121317));
#17813=CARTESIAN_POINT('Ctrl Pts',(3.16905364205286,-1.41691123325669,-7.55595954512955));
#17814=CARTESIAN_POINT('Ctrl Pts',(3.22288303313078,-1.429907185546,-7.55295773904593));
#17815=CARTESIAN_POINT('Ctrl Pts',(3.27731123190228,-1.43981919347764,-7.54995593296231));
#17816=CARTESIAN_POINT('Ctrl Pts',(3.33170708081012,-1.44972531012293,-7.54695591102771));
#17817=CARTESIAN_POINT('Ctrl Pts',(3.3867005134482,-1.45655102104369,-7.5439558890931));
#17818=CARTESIAN_POINT('Ctrl Pts',(3.44191384441607,-1.46024158061615,-7.5409558671585));
#17819=CARTESIAN_POINT('Ctrl Pts',(3.49711616551202,-1.46393140426872,-7.53795644344641));
#17820=CARTESIAN_POINT('Ctrl Pts',(3.55253777121056,-1.46448728292818,-7.53495701973431));
#17821=CARTESIAN_POINT('Ctrl Pts',(3.60779696129584,-1.46190641864889,-7.53195759602222));
#17822=CARTESIAN_POINT('Ctrl Pts',(3.66310695420265,-1.45932318163872,-7.52895541477446));
#17823=CARTESIAN_POINT('Ctrl Pts',(3.71825370450435,-1.45359746496207,-7.5259532335267));
#17824=CARTESIAN_POINT('Ctrl Pts',(3.77285813507016,-1.44477857181508,-7.52295105227893));
#17825=CARTESIAN_POINT('Ctrl Pts',(3.82748742036061,-1.43595566450369,-7.51994750450491));
#17826=CARTESIAN_POINT('Ctrl Pts',(3.88157337719182,-1.42403688793093,-7.51694395673089));
#17827=CARTESIAN_POINT('Ctrl Pts',(3.9347479329469,-1.40912255691934,-7.51394040895687));
#17828=CARTESIAN_POINT('Ctrl Pts',(3.98802284672706,-1.39418007761795,-7.51093119249191));
#17829=CARTESIAN_POINT('Ctrl Pts',(4.0403824224292,-1.37623092160211,-7.50792197602694));
#17830=CARTESIAN_POINT('Ctrl Pts',(4.09147565770711,-1.3554247133926,-7.50491275956197));
#17831=CARTESIAN_POINT('Ctrl Pts',(4.13056407666066,-1.33950711140665,-7.50261058563885));
#17832=CARTESIAN_POINT('Ctrl Pts',(4.16891166197947,-1.32191834261424,-7.50030841171573));
#17833=CARTESIAN_POINT('Ctrl Pts',(4.20637141150496,-1.30274332795045,-7.49800623779262));
#17834=CARTESIAN_POINT('Ctrl Pts',(4.25535062396027,-1.27767169429169,-7.49499610913138));
#17835=CARTESIAN_POINT('Ctrl Pts',(4.30301685460356,-1.24978133638674,-7.49198598047014));
#17836=CARTESIAN_POINT('Ctrl Pts',(4.34902626059857,-1.21923349965203,-7.4889758518089));
#17837=CARTESIAN_POINT('Ctrl Pts',(4.39495389491509,-1.18873995503065,-7.48597107299446));
#17838=CARTESIAN_POINT('Ctrl Pts',(4.43923011183765,-1.1555985943354,-7.48296629418001));
#17839=CARTESIAN_POINT('Ctrl Pts',(4.48153573146479,-1.12001643855748,-7.47996151536556));
#17840=CARTESIAN_POINT('Ctrl Pts',(4.52379949669023,-1.08446948542769,-7.47695970928195));
#17841=CARTESIAN_POINT('Ctrl Pts',(4.56409612446335,-1.04648685900667,-7.47395790319833));
#17842=CARTESIAN_POINT('Ctrl Pts',(4.60213705201202,-1.00631765993594,-7.47095609711471));
#17843=CARTESIAN_POINT('Ctrl Pts',(4.6401553696113,-0.966172335770903,-7.46795607518011));
#17844=CARTESIAN_POINT('Ctrl Pts',(4.67592028191785,-0.923843397553667,
-7.46495605324551));
#17845=CARTESIAN_POINT('Ctrl Pts',(4.70917957217821,-0.879617254177804,
-7.46195603131091));
#17846=CARTESIAN_POINT('Ctrl Pts',(4.74243223033506,-0.835399929762271,
-7.45895660759882));
#17847=CARTESIAN_POINT('Ctrl Pts',(4.77317994146253,-0.789286573348888,
-7.45595718388673));
#17848=CARTESIAN_POINT('Ctrl Pts',(4.80121180270633,-0.74159534035462,-7.45295776017464));
#17849=CARTESIAN_POINT('Ctrl Pts',(4.82926943518642,-0.693860262179192,
-7.44995557892688));
#17850=CARTESIAN_POINT('Ctrl Pts',(4.85460596125388,-0.644544865525292,
-7.44695339767913));
#17851=CARTESIAN_POINT('Ctrl Pts',(4.8770555474062,-0.593993576764832,-7.44395121643137));
#17852=CARTESIAN_POINT('Ctrl Pts',(4.89951535211179,-0.54341927817989,-7.44094766865735));
#17853=CARTESIAN_POINT('Ctrl Pts',(4.91908541045481,-0.491608460990895,
-7.43794412088333));
#17854=CARTESIAN_POINT('Ctrl Pts',(4.93564862536595,-0.438924207545657,
-7.43494057310931));
#17855=CARTESIAN_POINT('Ctrl Pts',(4.95224310055777,-0.38614052143844,-7.43193135664435));
#17856=CARTESIAN_POINT('Ctrl Pts',(4.96581926595016,-0.33248061925228,-7.42892214017938));
#17857=CARTESIAN_POINT('Ctrl Pts',(4.97631064980204,-0.278320229149412,
-7.42591292371442));
#17858=CARTESIAN_POINT('Ctrl Pts',(4.98433698841955,-0.236885311052895,
-7.4236107497913));
#17859=CARTESIAN_POINT('Ctrl Pts',(4.99055889127085,-0.19515774208079,-7.42130857586819));
#17860=CARTESIAN_POINT('Ctrl Pts',(4.99496716052216,-0.153307040962731,
-7.41900640194507));
#17861=CARTESIAN_POINT('Ctrl Pts',(5.00073104199375,-0.0985865901473312,
-7.41599627328384));
#17862=CARTESIAN_POINT('Ctrl Pts',(5.00341675794117,-0.043425657072795,
-7.4129861446226));
#17863=CARTESIAN_POINT('Ctrl Pts',(5.00297148136434,0.0117996767691311,
-7.40997601596136));
#17864=CARTESIAN_POINT('Ctrl Pts',(5.00252699616945,0.0669268596320173,
-7.40697123714692));
#17865=CARTESIAN_POINT('Ctrl Pts',(4.99896256577096,0.122117692291433,-7.40396645833247));
#17866=CARTESIAN_POINT('Ctrl Pts',(4.99227717717537,0.176991737532915,-7.40096167951803));
#17867=CARTESIAN_POINT('Ctrl Pts',(4.9855984026642,0.231811493997805,-7.39795987343441));
#17868=CARTESIAN_POINT('Ctrl Pts',(4.97580485003877,0.286314562229754,-7.39495806735079));
#17869=CARTESIAN_POINT('Ctrl Pts',(4.96294747822448,0.340123155528362,-7.39195626126717));
#17870=CARTESIAN_POINT('Ctrl Pts',(4.95009774829868,0.393899767231109,-7.38895623933257));
#17871=CARTESIAN_POINT('Ctrl Pts',(4.93418793103073,0.446982209501532,-7.38595621739797));
#17872=CARTESIAN_POINT('Ctrl Pts',(4.91532009133315,0.49900275132561,-7.38295619546338));
#17873=CARTESIAN_POINT('Ctrl Pts',(4.89645601399685,0.551012919939193,-7.37995677175128));
#17874=CARTESIAN_POINT('Ctrl Pts',(4.87463526561117,0.601961112440734,-7.37695734803919));
#17875=CARTESIAN_POINT('Ctrl Pts',(4.85000907340865,0.65149685314286,-7.3739579243271));
#17876=CARTESIAN_POINT('Ctrl Pts',(4.82536024098924,0.701078134783833,-7.37095574307934));
#17877=CARTESIAN_POINT('Ctrl Pts',(4.79790104745124,0.749243896384174,-7.36795356183158));
#17878=CARTESIAN_POINT('Ctrl Pts',(4.7678293483759,0.795667054704943,-7.36495138058382));
#17879=CARTESIAN_POINT('Ctrl Pts',(4.73774396133068,0.842111343816857,-7.3619478328098));
#17880=CARTESIAN_POINT('Ctrl Pts',(4.70504401060774,0.88681102148971,-7.35894428503578));
#17881=CARTESIAN_POINT('Ctrl Pts',(4.66996960606598,0.92946962900702,-7.35594073726176));
#17882=CARTESIAN_POINT('Ctrl Pts',(4.63482900448844,0.972208747466868,-7.3529315207968));
#17883=CARTESIAN_POINT('Ctrl Pts',(4.59730535573755,1.01289871126396,-7.34992230433183));
#17884=CARTESIAN_POINT('Ctrl Pts',(4.55767702236274,1.05127855213332,-7.34691308786687));
#17885=CARTESIAN_POINT('Ctrl Pts',(4.52735972323377,1.08064070332837,-7.34461091394374));
#17886=CARTESIAN_POINT('Ctrl Pts',(4.49581138450125,1.10865149429612,-7.34230874002062));
#17887=CARTESIAN_POINT('Ctrl Pts',(4.46316895700323,1.13521059723485,-7.3400065660975));
#17888=CARTESIAN_POINT('Ctrl Pts',(4.42048846896653,1.16993704260448,-7.33699643743626));
#17889=CARTESIAN_POINT('Ctrl Pts',(4.37575716762441,1.20232611928238,-7.33398630877503));
#17890=CARTESIAN_POINT('Ctrl Pts',(4.3292611668822,1.23212809378349,-7.33097618011379));
#17891=CARTESIAN_POINT('Ctrl Pts',(4.28284780263447,1.26187710177862,-7.32797140129934));
#17892=CARTESIAN_POINT('Ctrl Pts',(4.2346764041576,1.28904784969781,-7.3249666224849));
#17893=CARTESIAN_POINT('Ctrl Pts',(4.1850650443617,1.31343161973118,-7.32196184367045));
#17894=CARTESIAN_POINT('Ctrl Pts',(4.13550276678703,1.33779126606386,-7.31896003758683));
#17895=CARTESIAN_POINT('Ctrl Pts',(4.08450382159625,1.35936916469073,-7.31595823150321));
#17896=CARTESIAN_POINT('Ctrl Pts',(4.03241245907508,1.37800157391323,-7.31295642541959));
#17897=CARTESIAN_POINT('Ctrl Pts',(3.98035205749902,1.39662290880456,-7.309956403485));
#17898=CARTESIAN_POINT('Ctrl Pts',(3.92720102179366,1.41230204673812,-7.3069563815504));
#17899=CARTESIAN_POINT('Ctrl Pts',(3.87332310444746,1.42492354304251,-7.3039563596158));
#17900=CARTESIAN_POINT('Ctrl Pts',(3.81945593068366,1.43754252254425,-7.3009569359037));
#17901=CARTESIAN_POINT('Ctrl Pts',(3.76486267703996,1.44710495089072,-7.29795751219161));
#17902=CARTESIAN_POINT('Ctrl Pts',(3.70991950630306,1.45354598641937,-7.29495808847952));
#17903=CARTESIAN_POINT('Ctrl Pts',(3.65492582327863,1.45999294354728,-7.29195590723176));
#17904=CARTESIAN_POINT('Ctrl Pts',(3.59958210610123,1.46331271300988,-7.288953725984));
#17905=CARTESIAN_POINT('Ctrl Pts',(3.54427040329912,1.46349228718359,-7.28595154473625));
#17906=CARTESIAN_POINT('Ctrl Pts',(3.48893352383772,1.46367194309547,-7.28294799696223));
#17907=CARTESIAN_POINT('Ctrl Pts',(3.43362921607942,1.46070858272003,-7.27994444918821));
#17908=CARTESIAN_POINT('Ctrl Pts',(3.37873696726217,1.45464132064728,-7.27694090141419));
#17909=CARTESIAN_POINT('Ctrl Pts',(3.32374111856326,1.44856260763845,-7.27393168494922));
#17910=CARTESIAN_POINT('Ctrl Pts',(3.26915940442258,1.43936837842359,-7.27092246848426));
#17911=CARTESIAN_POINT('Ctrl Pts',(3.21536248898975,1.42714917709389,-7.26791325201929));
#17912=CARTESIAN_POINT('Ctrl Pts',(3.17420564391213,1.41780098729431,-7.26561107809617));
#17913=CARTESIAN_POINT('Ctrl Pts',(3.13350796418715,1.40668339077259,-7.26330890417305));
#17914=CARTESIAN_POINT('Ctrl Pts',(3.09342830644917,1.39385626882433,-7.26100673024994));
#17915=CARTESIAN_POINT('Ctrl Pts',(3.04102352274529,1.37708460486362,-7.2579966015887));
#17916=CARTESIAN_POINT('Ctrl Pts',(2.98945579188682,1.35731820048865,-7.25498647292746));
#17917=CARTESIAN_POINT('Ctrl Pts',(2.93909060390324,1.33466023039944,-7.25197634426622));
#17918=CARTESIAN_POINT('Ctrl Pts',(2.88881492905009,1.3120425299074,-7.24897156545178));
#17919=CARTESIAN_POINT('Ctrl Pts',(2.83973803339766,1.28654367725034,-7.24596678663733));
#17920=CARTESIAN_POINT('Ctrl Pts',(2.79220851751837,1.25831602445881,-7.24296200782289));
#17921=CARTESIAN_POINT('Ctrl Pts',(2.74472602422066,1.23011629825313,-7.23996020173927));
#17922=CARTESIAN_POINT('Ctrl Pts',(2.69878832994593,1.19919338822763,-7.23695839565565));
#17923=CARTESIAN_POINT('Ctrl Pts',(2.65472066977822,1.16574614544007,-7.23395658957203));
#17924=CARTESIAN_POINT('Ctrl Pts',(2.6106792015998,1.13231878230625,-7.23095656763743));
#17925=CARTESIAN_POINT('Ctrl Pts',(2.56850598434983,1.09637037886917,-7.22795654570284));
#17926=CARTESIAN_POINT('Ctrl Pts',(2.52849645897932,1.05814250911232,-7.22495652376824));
#17927=CARTESIAN_POINT('Ctrl Pts',(2.48849491174998,1.01992226222375,-7.22195710005615));
#17928=CARTESIAN_POINT('Ctrl Pts',(2.45065658117789,0.979423816342425,-7.21895767634406));
#17929=CARTESIAN_POINT('Ctrl Pts',(2.41524130777047,0.936926788695978,-7.21595825263197));
#17930=CARTESIAN_POINT('Ctrl Pts',(2.37979347514869,0.894390691187862,-7.21295607138421));
#17931=CARTESIAN_POINT('Ctrl Pts',(2.34677348907133,0.849852747591995,-7.20995389013645));
#17932=CARTESIAN_POINT('Ctrl Pts',(2.31640099358928,0.803625826518375,-7.20695170888869));
#17933=CARTESIAN_POINT('Ctrl Pts',(2.28601467322152,0.757377863976449,-7.20394816111467));
#17934=CARTESIAN_POINT('Ctrl Pts',(2.25827851063289,0.70943984935134,-7.20094461334065));
#17935=CARTESIAN_POINT('Ctrl Pts',(2.23336709663869,0.660150985476387,-7.19794106556663));
#17936=CARTESIAN_POINT('Ctrl Pts',(2.20840866654298,0.610769097165842,-7.19493184910167));
#17937=CARTESIAN_POINT('Ctrl Pts',(2.1862858466144,0.560031751868736,-7.1919226326367));
#17938=CARTESIAN_POINT('Ctrl Pts',(2.16712533317604,0.508298863722015,-7.18891341617174));
#17939=CARTESIAN_POINT('Ctrl Pts',(2.1524667551359,0.468721084108749,-7.18661124224862));
#17940=CARTESIAN_POINT('Ctrl Pts',(2.13954098899165,0.428561070948839,-7.1843090683255));
#17941=CARTESIAN_POINT('Ctrl Pts',(2.12838468118806,0.387984589853703,-7.18200689440238));
#17942=CARTESIAN_POINT('Ctrl Pts',(2.11011855844064,0.321549081136019,-7.17823756567768));
#17943=CARTESIAN_POINT('Ctrl Pts',(2.09653491201419,0.253774759083523,-7.17446823695298));
#17944=CARTESIAN_POINT('Ctrl Pts',(2.0877904184246,0.185246400872139,-7.17069890822829));
#17945=CARTESIAN_POINT('Ctrl Pts',(2.08002348789786,0.124378954188602,-7.16735095971221));
#17946=CARTESIAN_POINT('Ctrl Pts',(2.07607370014426,0.0629167803784564,
-7.16400301119612));
#17947=CARTESIAN_POINT('Ctrl Pts',(2.0760196139518,0.00128430857734538,
-7.16065506268004));
#17948=CARTESIAN_POINT('Ctrl Pts',(2.07601962331082,0.00129492948150936,
-7.08934495420699));
#17949=CARTESIAN_POINT('Ctrl Pts',(2.07608179175475,0.0715562706402045,
-7.0931627932276));
#17950=CARTESIAN_POINT('Ctrl Pts',(2.0812075995991,0.141595414252205,-7.09698063224821));
#17951=CARTESIAN_POINT('Ctrl Pts',(2.09127877754473,0.210789852728969,-7.10079847126883));
#17952=CARTESIAN_POINT('Ctrl Pts',(2.09935677175096,0.266290041101816,-7.10386072293943));
#17953=CARTESIAN_POINT('Ctrl Pts',(2.11061538540839,0.321247370894252,-7.10692297461003));
#17954=CARTESIAN_POINT('Ctrl Pts',(2.12497181061545,0.375350977556833,-7.10998522628063));
#17955=CARTESIAN_POINT('Ctrl Pts',(2.13908387312279,0.428533679244935,-7.11299535494186));
#17956=CARTESIAN_POINT('Ctrl Pts',(2.15622901998243,0.481031160584161,-7.1160054836031));
#17957=CARTESIAN_POINT('Ctrl Pts',(2.17632260802631,0.532473200674955,-7.11901561226434));
#17958=CARTESIAN_POINT('Ctrl Pts',(2.19638048410248,0.583823813765733,-7.12202039107878));
#17959=CARTESIAN_POINT('Ctrl Pts',(2.21937621153617,0.634122220236513,-7.12502516989323));
#17960=CARTESIAN_POINT('Ctrl Pts',(2.24517518188764,0.68301259138096,-7.12802994870767));
#17961=CARTESIAN_POINT('Ctrl Pts',(2.27094862843214,0.731854593602992,-7.13103175479129));
#17962=CARTESIAN_POINT('Ctrl Pts',(2.29951957877341,0.779290855221282,-7.13403356087491));
#17963=CARTESIAN_POINT('Ctrl Pts',(2.33070580806938,0.824986542381488,-7.13703536695852));
#17964=CARTESIAN_POINT('Ctrl Pts',(2.36187350156428,0.870655069920728,-7.14003538889312));
#17965=CARTESIAN_POINT('Ctrl Pts',(2.39565309595574,0.914584638159451,-7.14303541082772));
#17966=CARTESIAN_POINT('Ctrl Pts',(2.43181819766048,0.956468018696495,-7.14603543276232));
#17967=CARTESIAN_POINT('Ctrl Pts',(2.46797608782533,0.998343047434297,-7.14903485647441));
#17968=CARTESIAN_POINT('Ctrl Pts',(2.5065181956584,1.03817229928607,-7.1520342801865));
#17969=CARTESIAN_POINT('Ctrl Pts',(2.54717834026204,1.07568218585104,-7.15503370389859));
#17970=CARTESIAN_POINT('Ctrl Pts',(2.58787586597944,1.11322655732377,-7.15803588514635));
#17971=CARTESIAN_POINT('Ctrl Pts',(2.63069492977307,1.1484469445467,-7.16103806639411));
#17972=CARTESIAN_POINT('Ctrl Pts',(2.67533411782859,1.18110823055163,-7.16404024764187));
#17973=CARTESIAN_POINT('Ctrl Pts',(2.71999362465158,1.21378438324892,-7.16704379541588));
#17974=CARTESIAN_POINT('Ctrl Pts',(2.76647446325922,1.24389882502802,-7.1700473431899));
#17975=CARTESIAN_POINT('Ctrl Pts',(2.81444665079178,1.2712601092196,-7.17305089096391));
#17976=CARTESIAN_POINT('Ctrl Pts',(2.86250937775492,1.29867303323039,-7.17606010742888));
#17977=CARTESIAN_POINT('Ctrl Pts',(2.91206860236527,1.32332218383257,-7.17906932389384));
#17978=CARTESIAN_POINT('Ctrl Pts',(2.96277124546302,1.34506290539657,-7.18207854035881));
#17979=CARTESIAN_POINT('Ctrl Pts',(3.00156084539114,1.36169544839813,-7.18438071428193));
#17980=CARTESIAN_POINT('Ctrl Pts',(3.04101917939818,1.37662668963308,-7.18668288820506));
#17981=CARTESIAN_POINT('Ctrl Pts',(3.08098253705965,1.38981168361494,-7.18898506212818));
#17982=CARTESIAN_POINT('Ctrl Pts',(3.13323525658173,1.40705127089563,-7.19199519078942));
#17983=CARTESIAN_POINT('Ctrl Pts',(3.18657135100372,1.42137616669333,-7.19500531945066));
#17984=CARTESIAN_POINT('Ctrl Pts',(3.24063450166375,1.43265497469314,-7.19801544811189));
#17985=CARTESIAN_POINT('Ctrl Pts',(3.2946015668717,1.4439137370731,-7.20102022692634));
#17986=CARTESIAN_POINT('Ctrl Pts',(3.34929261116631,1.45213704830831,-7.20402500574078));
#17987=CARTESIAN_POINT('Ctrl Pts',(3.40433606890657,1.45724322318147,-7.20702978455523));
#17988=CARTESIAN_POINT('Ctrl Pts',(3.45932507026464,1.46234434634056,-7.21003159063885));
#17989=CARTESIAN_POINT('Ctrl Pts',(3.51466527112711,1.46433439363332,-7.21303339672246));
#17990=CARTESIAN_POINT('Ctrl Pts',(3.56997667219122,1.4631830313656,-7.21603520280609));
#17991=CARTESIAN_POINT('Ctrl Pts',(3.62525519845288,1.46203235341985,-7.21903522474069));
#17992=CARTESIAN_POINT('Ctrl Pts',(3.68050443189642,1.45774397764399,-7.22203524667529));
#17993=CARTESIAN_POINT('Ctrl Pts',(3.73534335990227,1.45033964636459,-7.22503526860989));
#17994=CARTESIAN_POINT('Ctrl Pts',(3.79017135269438,1.44293679155361,-7.22803469232198));
#17995=CARTESIAN_POINT('Ctrl Pts',(3.84458867946096,1.4324192858196,-7.23103411603407));
#17996=CARTESIAN_POINT('Ctrl Pts',(3.89822076235576,1.41886057519987,-7.23403353974616));
#17997=CARTESIAN_POINT('Ctrl Pts',(3.95190215218274,1.40528939930955,-7.23703572099392));
#17998=CARTESIAN_POINT('Ctrl Pts',(4.00479634273179,1.38867156231254,-7.24003790224168));
#17999=CARTESIAN_POINT('Ctrl Pts',(4.05654172588942,1.36913103940183,-7.24304008348944));
#18000=CARTESIAN_POINT('Ctrl Pts',(4.10831066239682,1.34958162207885,-7.24604363126346));
#18001=CARTESIAN_POINT('Ctrl Pts',(4.15892926560436,1.32710708157942,-7.24904717903748));
#18002=CARTESIAN_POINT('Ctrl Pts',(4.2080568924349,1.30187918172081,-7.2520507268115));
#18003=CARTESIAN_POINT('Ctrl Pts',(4.25727723939323,1.27660366844691,-7.25505994327647));
#18004=CARTESIAN_POINT('Ctrl Pts',(4.30500053218034,1.24856468317737,-7.25806915974144));
#18005=CARTESIAN_POINT('Ctrl Pts',(4.3509126967465,1.21797889994279,-7.2610783762064));
#18006=CARTESIAN_POINT('Ctrl Pts',(4.38603738426848,1.1945795222641,-7.26338055012952));
#18007=CARTESIAN_POINT('Ctrl Pts',(4.42010257944943,1.1696904771901,-7.26568272405263));
#18008=CARTESIAN_POINT('Ctrl Pts',(4.45298118850154,1.14342431856987,-7.26798489797575));
#18009=CARTESIAN_POINT('Ctrl Pts',(4.49597048763992,1.10908090251015,-7.27099502663699));
#18010=CARTESIAN_POINT('Ctrl Pts',(4.53711060601078,1.07223755483061,-7.27400515529822));
#18011=CARTESIAN_POINT('Ctrl Pts',(4.57609680454605,1.03312090756948,-7.27701528395946));
#18012=CARTESIAN_POINT('Ctrl Pts',(4.61501371362141,0.994073781612415,-7.2800200627739));
#18013=CARTESIAN_POINT('Ctrl Pts',(4.65178393000102,0.952761745096384,-7.28302484158835));
#18014=CARTESIAN_POINT('Ctrl Pts',(4.68613601810939,0.909451361763591,-7.28602962040279));
#18015=CARTESIAN_POINT('Ctrl Pts',(4.7204541205178,0.866183826879724,-7.28903142648641));
#18016=CARTESIAN_POINT('Ctrl Pts',(4.7523585071905,0.82092227331864,-7.29203323257003));
#18017=CARTESIAN_POINT('Ctrl Pts',(4.78161614271498,0.773968386511875,-7.29503503865365));
#18018=CARTESIAN_POINT('Ctrl Pts',(4.81085638871451,0.727042407147772,-7.29803506058825));
#18019=CARTESIAN_POINT('Ctrl Pts',(4.83745272285583,0.678426535530215,-7.30103508252285));
#18020=CARTESIAN_POINT('Ctrl Pts',(4.86121517112297,0.628451759904153,-7.30403510445745));
#18021=CARTESIAN_POINT('Ctrl Pts',(4.88497288101429,0.578486949550428,-7.30703452816954));
#18022=CARTESIAN_POINT('Ctrl Pts',(4.90589760062895,0.527164250007887,-7.31003395188163));
#18023=CARTESIAN_POINT('Ctrl Pts',(4.92384617513506,0.474837510930213,-7.31303337559372));
#18024=CARTESIAN_POINT('Ctrl Pts',(4.94181125075578,0.422462664994939,-7.31603555684148));
#18025=CARTESIAN_POINT('Ctrl Pts',(4.95679454310981,0.369082435972092,-7.31903773808924));
#18026=CARTESIAN_POINT('Ctrl Pts',(4.96870230350416,0.315067419947433,-7.322039919337));
#18027=CARTESIAN_POINT('Ctrl Pts',(4.98061548404671,0.261027817486531,-7.32504346711102));
#18028=CARTESIAN_POINT('Ctrl Pts',(4.98945025760604,0.206353374302396,-7.32804701488504));
#18029=CARTESIAN_POINT('Ctrl Pts',(4.99516435496168,0.151423239215319,-7.33105056265906));
#18030=CARTESIAN_POINT('Ctrl Pts',(5.00088923671444,0.0963894327426314,
-7.33405977912402));
#18031=CARTESIAN_POINT('Ctrl Pts',(5.0034816517754,0.0410994991783652,-7.33706899558899));
#18032=CARTESIAN_POINT('Ctrl Pts',(5.00295146164869,-0.0140651261684224,
-7.34007821205395));
#18033=CARTESIAN_POINT('Ctrl Pts',(5.00254584447285,-0.0562683253834388,
-7.34238038597707));
#18034=CARTESIAN_POINT('Ctrl Pts',(5.00031368830613,-0.0983981196657256,
-7.3446825599002));
#18035=CARTESIAN_POINT('Ctrl Pts',(4.99627981647953,-0.140286565566228,
-7.34698473382331));
#18036=CARTESIAN_POINT('Ctrl Pts',(4.99100546553712,-0.195056368279009,
-7.34999486248455));
#18037=CARTESIAN_POINT('Ctrl Pts',(4.98262696947039,-0.249643385155416,
-7.35300499114579));
#18038=CARTESIAN_POINT('Ctrl Pts',(4.97116763048022,-0.303668558168483,
-7.35601511980703));
#18039=CARTESIAN_POINT('Ctrl Pts',(4.95972865796432,-0.357597713226465,
-7.35901989862147));
#18040=CARTESIAN_POINT('Ctrl Pts',(4.94521981743802,-0.410966493616206,
-7.36202467743592));
#18041=CARTESIAN_POINT('Ctrl Pts',(4.92771605187653,-0.463401915355784,
-7.36502945625036));
#18042=CARTESIAN_POINT('Ctrl Pts',(4.91022960339115,-0.51578546093271,-7.36803126233398));
#18043=CARTESIAN_POINT('Ctrl Pts',(4.88975426579602,-0.567236978598274,
-7.3710330684176));
#18044=CARTESIAN_POINT('Ctrl Pts',(4.86641537912471,-0.61739645518735,-7.37403487450122));
#18045=CARTESIAN_POINT('Ctrl Pts',(4.84309036411953,-0.667526119064172,
-7.37703489643582));
#18046=CARTESIAN_POINT('Ctrl Pts',(4.81690539581176,-0.716364786097724,
-7.38003491837042));
#18047=CARTESIAN_POINT('Ctrl Pts',(4.78803388470787,-0.763572497259173,
-7.38303494030502));
#18048=CARTESIAN_POINT('Ctrl Pts',(4.75916813075781,-0.810770794917652,
-7.38603436401711));
#18049=CARTESIAN_POINT('Ctrl Pts',(4.72761717330138,-0.856338332297551,
-7.3890337877292));
#18050=CARTESIAN_POINT('Ctrl Pts',(4.69359915170852,-0.89996187131277,-7.39203321144129));
#18051=CARTESIAN_POINT('Ctrl Pts',(4.65954985547196,-0.943625515853699,
-7.39503539268905));
#18052=CARTESIAN_POINT('Ctrl Pts',(4.62302928917016,-0.985341174032534,
-7.39803757393681));
#18053=CARTESIAN_POINT('Ctrl Pts',(4.58429661308093,-1.0248278365494,-7.40103975518456));
#18054=CARTESIAN_POINT('Ctrl Pts',(4.54554630673736,-1.0643324725185,-7.40404330295858));
#18055=CARTESIAN_POINT('Ctrl Pts',(4.50458227471166,-1.10160573426922,-7.4070468507326));
#18056=CARTESIAN_POINT('Ctrl Pts',(4.46169896860869,-1.13640505476481,-7.41005039850662));
#18057=CARTESIAN_POINT('Ctrl Pts',(4.41873472748243,-1.17127005312134,-7.41305961497159));
#18058=CARTESIAN_POINT('Ctrl Pts',(4.37384440552029,-1.20365147315699,-7.41606883143655));
#18059=CARTESIAN_POINT('Ctrl Pts',(4.32735285334631,-1.23334915939136,-7.41907804790152));
#18060=CARTESIAN_POINT('Ctrl Pts',(4.2917849105591,-1.25606910646785,-7.42138022182464));
#18061=CARTESIAN_POINT('Ctrl Pts',(4.25528043264427,-1.27721916981486,-7.42368239574776));
#18062=CARTESIAN_POINT('Ctrl Pts',(4.21799364013086,-1.2967283759989,-7.42598456967087));
#18063=CARTESIAN_POINT('Ctrl Pts',(4.16924057169274,-1.32223697033352,-7.42899469833211));
#18064=CARTESIAN_POINT('Ctrl Pts',(4.11894449860163,-1.34504588612142,-7.43200482699335));
#18065=CARTESIAN_POINT('Ctrl Pts',(4.06743562438777,-1.36496752376505,-7.43501495565459));
#18066=CARTESIAN_POINT('Ctrl Pts',(4.01601829595701,-1.38485375504527,-7.43801973446903));
#18067=CARTESIAN_POINT('Ctrl Pts',(3.96339293256247,-1.40186270272871,-7.44102451328347));
#18068=CARTESIAN_POINT('Ctrl Pts',(3.90991286687456,-1.4158533365905,-7.44402929209792));
#18069=CARTESIAN_POINT('Ctrl Pts',(3.8564857108514,-1.42983012903796,-7.44703109818154));
#18070=CARTESIAN_POINT('Ctrl Pts',(3.80220603601128,-1.44079439002423,-7.45003290426516));
#18071=CARTESIAN_POINT('Ctrl Pts',(3.7474438483713,-1.44865438542054,-7.45303471034878));
#18072=CARTESIAN_POINT('Ctrl Pts',(3.6927142091041,-1.45650970916162,-7.45603473228338));
#18073=CARTESIAN_POINT('Ctrl Pts',(3.6375031471802,-1.46126434943483,-7.45903475421797));
#18074=CARTESIAN_POINT('Ctrl Pts',(3.58219013825552,-1.46287778992751,-7.46203477615257));
#18075=CARTESIAN_POINT('Ctrl Pts',(3.52688815907917,-1.4644909086904,-7.46503419986466));
#18076=CARTESIAN_POINT('Ctrl Pts',(3.47148480086988,-1.46296405623551,-7.46803362357676));
#18077=CARTESIAN_POINT('Ctrl Pts',(3.41636159945032,-1.45830877809534,-7.47103304728885));
#18078=CARTESIAN_POINT('Ctrl Pts',(3.36118772023106,-1.45364922010118,-7.4740352285366));
#18079=CARTESIAN_POINT('Ctrl Pts',(3.3062950397537,-1.44585553481704,-7.47703740978436));
#18080=CARTESIAN_POINT('Ctrl Pts',(3.25206051502811,-1.43499123357205,-7.48003959103212));
#18081=CARTESIAN_POINT('Ctrl Pts',(3.19780130395077,-1.42412198713829,-7.48304313880614));
#18082=CARTESIAN_POINT('Ctrl Pts',(3.14420135781168,-1.41017947175448,-7.48604668658016));
#18083=CARTESIAN_POINT('Ctrl Pts',(3.09162472023332,-1.39327776088759,-7.48905023435418));
#18084=CARTESIAN_POINT('Ctrl Pts',(3.0389488530998,-1.37634415088588,-7.49205945081915));
#18085=CARTESIAN_POINT('Ctrl Pts',(2.98730064664274,-1.35644037890267,-7.49506866728411));
#18086=CARTESIAN_POINT('Ctrl Pts',(2.93702523356946,-1.33372915190951,-7.49807788374908));
#18087=CARTESIAN_POINT('Ctrl Pts',(2.89856248211946,-1.31635413248025,-7.5003800576722));
#18088=CARTESIAN_POINT('Ctrl Pts',(2.86090283142582,-1.29733696136966,-7.50268223159532));
#18089=CARTESIAN_POINT('Ctrl Pts',(2.82418998914086,-1.2767680228159,-7.50498440551843));
#18090=CARTESIAN_POINT('Ctrl Pts',(2.77618736966552,-1.24987381171822,-7.50799453417967));
#18091=CARTESIAN_POINT('Ctrl Pts',(2.72960271194419,-1.22021219893684,-7.51100466284091));
#18092=CARTESIAN_POINT('Ctrl Pts',(2.68477355760134,-1.18795723513141,-7.51401479150215));
#18093=CARTESIAN_POINT('Ctrl Pts',(2.64002407729726,-1.15575959748514,-7.51701957031659));
#18094=CARTESIAN_POINT('Ctrl Pts',(2.59702433387971,-1.12097806158276,-7.52002434913103));
#18095=CARTESIAN_POINT('Ctrl Pts',(2.55608550354162,-1.08383149468371,-7.52302912794548));
#18096=CARTESIAN_POINT('Ctrl Pts',(2.51518717539366,-1.0467216781584,-7.52603093402909));
#18097=CARTESIAN_POINT('Ctrl Pts',(2.47634611048559,-1.00725181881574,-7.52903274011271));
#18098=CARTESIAN_POINT('Ctrl Pts',(2.43984130845434,-0.965681683485155,
-7.53203454619633));
#18099=CARTESIAN_POINT('Ctrl Pts',(2.40335820336318,-0.924136255718675,
-7.53503456813093));
#18100=CARTESIAN_POINT('Ctrl Pts',(2.36920895667512,-0.88049342224595,-7.53803459006553));
#18101=CARTESIAN_POINT('Ctrl Pts',(2.33763484590116,-0.835048866187434,
-7.54103461200013));
#18102=CARTESIAN_POINT('Ctrl Pts',(2.30606703119571,-0.789613372048069,
-7.54403403571222));
#18103=CARTESIAN_POINT('Ctrl Pts',(2.27707363378539,-0.742377302293122,
-7.54703345942431));
#18104=CARTESIAN_POINT('Ctrl Pts',(2.25085345365173,-0.69366651187596,-7.5500328831364));
#18105=CARTESIAN_POINT('Ctrl Pts',(2.22460916786017,-0.64491093894229,-7.55303506438416));
#18106=CARTESIAN_POINT('Ctrl Pts',(2.20114344391124,-0.594678402674966,
-7.55603724563191));
#18107=CARTESIAN_POINT('Ctrl Pts',(2.18060905718792,-0.543319317055689,
-7.55903942687967));
#18108=CARTESIAN_POINT('Ctrl Pts',(2.16006532366759,-0.491936853920719,
-7.56204297465369));
#18109=CARTESIAN_POINT('Ctrl Pts',(2.14245575537787,-0.439427320824445,
-7.56504652242771));
#18110=CARTESIAN_POINT('Ctrl Pts',(2.12788372472633,-0.386157943392716,
-7.56805007020173));
#18111=CARTESIAN_POINT('Ctrl Pts',(2.11328419181931,-0.332788028975963,
-7.5710592866667));
#18112=CARTESIAN_POINT('Ctrl Pts',(2.101733759267,-0.278655923186127,-7.57406850313166));
#18113=CARTESIAN_POINT('Ctrl Pts',(2.09328473475822,-0.224139586404663,
-7.57707771959663));
#18114=CARTESIAN_POINT('Ctrl Pts',(2.08682088474065,-0.182432354511015,
-7.57937989351975));
#18115=CARTESIAN_POINT('Ctrl Pts',(2.08217119205194,-0.140500475882394,
-7.58168206744287));
#18116=CARTESIAN_POINT('Ctrl Pts',(2.0793384787572,-0.0985136951381293,
-7.583984241366));
#18117=CARTESIAN_POINT('Ctrl Pts',(2.07713977977388,-0.0659243426234165,
-7.58577114562969));
#18118=CARTESIAN_POINT('Ctrl Pts',(2.07603198051246,-0.0332605710567609,
-7.58755804989339));
#18119=CARTESIAN_POINT('Ctrl Pts',(2.07601916294366,-0.000573888477519203,
-7.58934495415709));
#18120=CARTESIAN_POINT('Origin',(3.53951905042299,8.32667268468867E-16,
0.));
#18121=CARTESIAN_POINT('',(2.07789371708856,-0.000813024483110047,-8.16065504584291));
#18122=CARTESIAN_POINT('',(2.07796531875306,-0.000756418292827756,-8.08934495415709));
#18123=CARTESIAN_POINT('',(2.07601905042299,1.01189432752408E-15,0.));
#18124=CARTESIAN_POINT('Ctrl Pts',(2.07789371708856,-0.000813024483110047,
-8.16065504584291));
#18125=CARTESIAN_POINT('Ctrl Pts',(2.07693198018494,-0.18926297634554,-8.15043833875298));
#18126=CARTESIAN_POINT('Ctrl Pts',(2.19803679261536,-0.862248877409424,
-8.11388835304717));
#18127=CARTESIAN_POINT('Ctrl Pts',(3.20845871698005,-1.69493867564852,-8.05100508872559));
#18128=CARTESIAN_POINT('Ctrl Pts',(4.77818574047571,-1.20337977775244,-7.97200525287798));
#18129=CARTESIAN_POINT('Ctrl Pts',(5.22418461769582,0.379894702512827,-7.89300541703046));
#18130=CARTESIAN_POINT('Ctrl Pts',(4.14184166559634,1.61852572602733,-7.81400558118286));
#18131=CARTESIAN_POINT('Ctrl Pts',(2.54502163675168,1.39332412042453,-7.73655563325641));
#18132=CARTESIAN_POINT('Ctrl Pts',(2.07592938050414,0.453437848859226,-7.68543896394578));
#18133=CARTESIAN_POINT('Ctrl Pts',(2.07388874310075,-0.000493743824116852,
-7.66065557325101));
#18134=CARTESIAN_POINT('Ctrl Pts',(2.07395567091487,-0.000564195093096354,
-7.58934552749836));
#18135=CARTESIAN_POINT('Ctrl Pts',(2.07622157562037,0.449077329977556,-7.61389171073677));
#18136=CARTESIAN_POINT('Ctrl Pts',(2.53748680820253,1.38510922610061,-7.66477117259103));
#18137=CARTESIAN_POINT('Ctrl Pts',(4.1273450240176,1.62384686131859,-7.74198391306112));
#18138=CARTESIAN_POINT('Ctrl Pts',(5.22072030366117,0.394943477419077,-7.82098374890869));
#18139=CARTESIAN_POINT('Ctrl Pts',(4.7888966068738,-1.19225572998487,-7.89998358475626));
#18140=CARTESIAN_POINT('Ctrl Pts',(3.22362778172652,-1.69783117847794,-7.97898342060381));
#18141=CARTESIAN_POINT('Ctrl Pts',(2.20196131736979,-0.871103028593394,
-8.04210387707076));
#18142=CARTESIAN_POINT('Ctrl Pts',(2.0770525139401,-0.193605137899811,-8.07889105492185));
#18143=CARTESIAN_POINT('Ctrl Pts',(2.07796531875306,-0.000756418292827756,
-8.08934495415709));
#18144=CARTESIAN_POINT('Origin',(3.53951905042299,8.32667268468867E-16,
0.));
#18145=CARTESIAN_POINT('',(2.07672228599458,0.00126145580453749,-8.66065504584291));
#18146=CARTESIAN_POINT('',(2.07601960916399,0.00127884111782682,-8.58934497249013));
#18147=CARTESIAN_POINT('',(2.07601905042299,1.01189432752408E-15,0.));
#18148=CARTESIAN_POINT('Ctrl Pts',(2.07672228599458,0.00126145580453749,
-8.66065504584291));
#18149=CARTESIAN_POINT('Ctrl Pts',(2.07963777649526,-0.346349860195879,
-8.64177134378144));
#18150=CARTESIAN_POINT('Ctrl Pts',(2.37702178386745,-1.18318906413124,-8.59655436310413));
#18151=CARTESIAN_POINT('Ctrl Pts',(3.7699732897758,-1.71152239351114,-8.52500410381095));
#18152=CARTESIAN_POINT('Ctrl Pts',(5.09888440860025,-0.742157488805154,
-8.44600426796337));
#18153=CARTESIAN_POINT('Ctrl Pts',(5.01312703127878,0.900498515814794,-8.36700443211582));
#18154=CARTESIAN_POINT('Ctrl Pts',(3.59050092423819,1.72621519727753,-8.28800459626826));
#18155=CARTESIAN_POINT('Ctrl Pts',(2.3115872043854,1.08163819160217,-8.21922146751061));
#18156=CARTESIAN_POINT('Ctrl Pts',(2.07941083032865,0.296461537811273,-8.17677161736884));
#18157=CARTESIAN_POINT('Ctrl Pts',(2.07789371708856,-0.000813024483110047,
-8.16065504584291));
#18158=CARTESIAN_POINT('Ctrl Pts',(2.07796531875306,-0.000756418292827756,
-8.08934495415709));
#18159=CARTESIAN_POINT('Ctrl Pts',(2.07935186109475,0.292179060880606,-8.1052243335377));
#18160=CARTESIAN_POINT('Ctrl Pts',(2.30635466103924,1.07287711057751,-8.14743699153416));
#18161=CARTESIAN_POINT('Ctrl Pts',(3.57506339039297,1.72660203989655,-8.21598292814651));
#18162=CARTESIAN_POINT('Ctrl Pts',(5.00501601458435,0.913639235277645,-8.29498276399406));
#18163=CARTESIAN_POINT('Ctrl Pts',(5.10545828694895,-0.728184256712089,
-8.37398259984163));
#18164=CARTESIAN_POINT('Ctrl Pts',(3.78526818937201,-1.70939327399081,-8.45298243568918));
#18165=CARTESIAN_POINT('Ctrl Pts',(2.3830149561948,-1.19182649892971,-8.52476988712768));
#18166=CARTESIAN_POINT('Ctrl Pts',(2.07961074474305,-0.350624743640976,
-8.57022405995031));
#18167=CARTESIAN_POINT('Ctrl Pts',(2.07659996625117,0.00127799658744232,
-8.58934495415709));
#18168=CARTESIAN_POINT('Origin',(3.53951905042299,8.32667268468867E-16,
0.));
#18169=CARTESIAN_POINT('',(2.07585468749027,-0.000399586479062222,-9.16065504584292));
#18170=CARTESIAN_POINT('',(2.07601912703111,-0.000473531363087066,-9.08934495420967));
#18171=CARTESIAN_POINT('',(2.07601905042299,1.01189432752408E-15,0.));
#18172=CARTESIAN_POINT('Ctrl Pts',(2.0738084935334,-0.000400145098551985,
-9.16065504584292));
#18173=CARTESIAN_POINT('Ctrl Pts',(2.07372679669453,-0.0226950761968628,
-9.15943762742576));
#18174=CARTESIAN_POINT('Ctrl Pts',(2.08425249274981,-0.527160066346179,
-9.13188693039255));
#18175=CARTESIAN_POINT('Ctrl Pts',(2.66326349110611,-1.48815124140486,-9.07800295474405));
#18176=CARTESIAN_POINT('Ctrl Pts',(4.30710318516207,-1.54700766169977,-8.99900311889623));
#18177=CARTESIAN_POINT('Ctrl Pts',(5.25458455049922,-0.202406515394875,
-8.92000328304879));
#18178=CARTESIAN_POINT('Ctrl Pts',(4.64614501576207,1.32581937401458,-8.84100344720118));
#18179=CARTESIAN_POINT('Ctrl Pts',(3.03376572375074,1.65125153735703,-8.76200361135363));
#18180=CARTESIAN_POINT('Ctrl Pts',(2.15594970700447,0.758946513770955,-8.70188747756755));
#18181=CARTESIAN_POINT('Ctrl Pts',(2.07557213177123,0.138393311691988,-8.6681046223973));
#18182=CARTESIAN_POINT('Ctrl Pts',(2.07672228599458,0.00126145580453749,
-8.66065504584291));
#18183=CARTESIAN_POINT('Ctrl Pts',(2.07601960916399,0.00127884111782682,
-8.58934497249013));
#18184=CARTESIAN_POINT('Ctrl Pts',(2.07607995389544,0.0703370528976135,
-8.59309584414968));
#18185=CARTESIAN_POINT('Ctrl Pts',(2.08103218347023,0.139181342753791,-8.59684671580924));
#18186=CARTESIAN_POINT('Ctrl Pts',(2.09076283215383,0.207214068119058,-8.6005975874688));
#18187=CARTESIAN_POINT('Ctrl Pts',(2.09974279949806,0.269998335847097,-8.60405909410731));
#18188=CARTESIAN_POINT('Ctrl Pts',(2.11279171882277,0.332091823618981,-8.60752060074581));
#18189=CARTESIAN_POINT('Ctrl Pts',(2.12978476702327,0.393041346689484,-8.61098210738432));
#18190=CARTESIAN_POINT('Ctrl Pts',(2.14456193393777,0.44604309570737,-8.61399223604218));
#18191=CARTESIAN_POINT('Ctrl Pts',(2.16236336355835,0.498321683152169,-8.61700236470005));
#18192=CARTESIAN_POINT('Ctrl Pts',(2.18309978165723,0.549507977486184,-8.62001249335791));
#18193=CARTESIAN_POINT('Ctrl Pts',(2.20379934529848,0.600603299352993,-8.62301727216902));
#18194=CARTESIAN_POINT('Ctrl Pts',(2.22742334894202,0.650609695140782,-8.62602205098014));
#18195=CARTESIAN_POINT('Ctrl Pts',(2.25383273729771,0.699173050283212,-8.62902682979125));
#18196=CARTESIAN_POINT('Ctrl Pts',(2.28021599793915,0.747688360031737,-8.63202863587156));
#18197=CARTESIAN_POINT('Ctrl Pts',(2.30937893336773,0.794762995570515,-8.63503044195187));
#18198=CARTESIAN_POINT('Ctrl Pts',(2.34113513862651,0.840064432021361,-8.63803224803218));
#18199=CARTESIAN_POINT('Ctrl Pts',(2.37287246931444,0.885338943177917,-8.6410322699635));
#18200=CARTESIAN_POINT('Ctrl Pts',(2.40719971227237,0.928841912593762,-8.64403229189482));
#18201=CARTESIAN_POINT('Ctrl Pts',(2.44388664307717,0.970268971973029,-8.64703231382614));
#18202=CARTESIAN_POINT('Ctrl Pts',(2.48056625828663,1.01168777054673,-8.65003173753498));
#18203=CARTESIAN_POINT('Ctrl Pts',(2.51960427694535,1.0510310860224,-8.65303116124383));
#18204=CARTESIAN_POINT('Ctrl Pts',(2.56073111184097,1.08802868587476,-8.65603058495268));
#18205=CARTESIAN_POINT('Ctrl Pts',(2.60189575690564,1.12506029966251,-8.65903276619728));
#18206=CARTESIAN_POINT('Ctrl Pts',(2.64515266137718,1.15974153536591,-8.66203494744187));
#18207=CARTESIAN_POINT('Ctrl Pts',(2.69019748981689,1.1918410702311,-8.66503712868647));
#18208=CARTESIAN_POINT('Ctrl Pts',(2.73526282166318,1.22395521609243,-8.66804067645736));
#18209=CARTESIAN_POINT('Ctrl Pts',(2.78211725221439,1.25348503649361,-8.67104422422826));
#18210=CARTESIAN_POINT('Ctrl Pts',(2.83042842627935,1.28024323343323,-8.67404777199916));
#18211=CARTESIAN_POINT('Ctrl Pts',(2.87883077955668,1.30705193196735,-8.6770569884611));
#18212=CARTESIAN_POINT('Ctrl Pts',(2.92869489168338,1.33107832755431,-8.68006620492305));
#18213=CARTESIAN_POINT('Ctrl Pts',(2.9796658991248,1.352182198885,-8.683075421385));
#18214=CARTESIAN_POINT('Ctrl Pts',(3.01866080925094,1.36832752555526,-8.68537759533396));
#18215=CARTESIAN_POINT('Ctrl Pts',(3.05830308904755,1.3827633067805,-8.68767976928291));
#18216=CARTESIAN_POINT('Ctrl Pts',(3.09842847790439,1.39544665137554,-8.68998194323187));
#18217=CARTESIAN_POINT('Ctrl Pts',(3.15089305509941,1.41203032397176,-8.69299207188863));
#18218=CARTESIAN_POINT('Ctrl Pts',(3.20440441028564,1.42568596251956,-8.69600220054538));
#18219=CARTESIAN_POINT('Ctrl Pts',(3.25860460677885,1.43628664456372,-8.69901232920214));
#18220=CARTESIAN_POINT('Ctrl Pts',(3.31270847424938,1.44686848620863,-8.70201710801203));
#18221=CARTESIAN_POINT('Ctrl Pts',(3.36749823936066,1.45440604571561,-8.70502188682191));
#18222=CARTESIAN_POINT('Ctrl Pts',(3.42260134236897,1.45882229882306,-8.7080266656318));
#18223=CARTESIAN_POINT('Ctrl Pts',(3.47764992998511,1.46323418277965,-8.71102847171082));
#18224=CARTESIAN_POINT('Ctrl Pts',(3.53301071757116,1.46453083556383,-8.71403027778983));
#18225=CARTESIAN_POINT('Ctrl Pts',(3.58830335565611,1.46268668605513,-8.71703208386885));
#18226=CARTESIAN_POINT('Ctrl Pts',(3.64356313008982,1.46084363263241,-8.72003210579881));
#18227=CARTESIAN_POINT('Ctrl Pts',(3.69875430853763,1.45586349453199,-8.72303212772878));
#18228=CARTESIAN_POINT('Ctrl Pts',(3.75349618063956,1.44777278526165,-8.72603214965874));
#18229=CARTESIAN_POINT('Ctrl Pts',(3.8082271368808,1.43968368932773,-8.72903157336616));
#18230=CARTESIAN_POINT('Ctrl Pts',(3.86250844255891,1.42848533121913,-8.73203099707359));
#18231=CARTESIAN_POINT('Ctrl Pts',(3.91596646926689,1.41425584349005,-8.73503042078102));
#18232=CARTESIAN_POINT('Ctrl Pts',(3.96947364288763,1.400013273808,-8.73803260202411));
#18233=CARTESIAN_POINT('Ctrl Pts',(4.02215551393625,1.38273414320771,-8.7410347832672));
#18234=CARTESIAN_POINT('Ctrl Pts',(4.07365205569197,1.36254694696452,-8.7440369645103));
#18235=CARTESIAN_POINT('Ctrl Pts',(4.12517203753024,1.34235056195776,-8.74704051227964));
#18236=CARTESIAN_POINT('Ctrl Pts',(4.17550513375568,1.31924369335141,-8.75004406004898));
#18237=CARTESIAN_POINT('Ctrl Pts',(4.22431287967973,1.29340235866953,-8.75304760781833));
#18238=CARTESIAN_POINT('Ctrl Pts',(4.27321274201106,1.26751225281689,-8.75605682427866));
#18239=CARTESIAN_POINT('Ctrl Pts',(4.32058105004415,1.23887764518127,-8.759066040739));
#18240=CARTESIAN_POINT('Ctrl Pts',(4.36610646861661,1.20771912715002,-8.76207525719933));
#18241=CARTESIAN_POINT('Ctrl Pts',(4.4009352802155,1.18388158346036,-8.76437743115937));
#18242=CARTESIAN_POINT('Ctrl Pts',(4.43468602173213,1.15856776131379,-8.76667960511941));
#18243=CARTESIAN_POINT('Ctrl Pts',(4.46723301928997,1.13189179781862,-8.76898177907944));
#18244=CARTESIAN_POINT('Ctrl Pts',(4.5097887307986,1.09701255574114,-8.77199190776219));
#18245=CARTESIAN_POINT('Ctrl Pts',(4.550464090331,1.05965674258027,-8.77500203644493));
#18246=CARTESIAN_POINT('Ctrl Pts',(4.58895722171386,1.02005479001751,-8.77801216512767));
#18247=CARTESIAN_POINT('Ctrl Pts',(4.62738193995691,0.980523221282205,-8.78101694396365));
#18248=CARTESIAN_POINT('Ctrl Pts',(4.66363176171128,0.938753810976068,-8.78402172279962));
#18249=CARTESIAN_POINT('Ctrl Pts',(4.69743861190192,0.895016502163194,-8.7870265016356));
#18250=CARTESIAN_POINT('Ctrl Pts',(4.73121201581545,0.851322464170957,-8.79002830774075));
#18251=CARTESIAN_POINT('Ctrl Pts',(4.76254691457255,0.80566480019676,-8.79303011384591));
#18252=CARTESIAN_POINT('Ctrl Pts',(4.7912140702125,0.75834809120491,-8.79603191995106));
#18253=CARTESIAN_POINT('Ctrl Pts',(4.81986418728404,0.711059505302565,-8.79903194190715));
#18254=CARTESIAN_POINT('Ctrl Pts',(4.84584943088369,0.662114279615942,-8.80203196386324));
#18255=CARTESIAN_POINT('Ctrl Pts',(4.86898398814057,0.611845756199704,-8.80503198581934));
#18256=CARTESIAN_POINT('Ctrl Pts',(4.89211393222636,0.561587256632074,-8.80803140955285));
#18257=CARTESIAN_POINT('Ctrl Pts',(4.91239409820926,0.510006462855934,-8.81103083328636));
#18258=CARTESIAN_POINT('Ctrl Pts',(4.92968577511037,0.45745899004389,-8.81403025701987));
#18259=CARTESIAN_POINT('Ctrl Pts',(4.9469933492021,0.404863207446886,-8.81703243828877));
#18260=CARTESIAN_POINT('Ctrl Pts',(4.96130677966633,0.351299472995499,-8.82003461955766));
#18261=CARTESIAN_POINT('Ctrl Pts',(4.97253696756643,0.297139528077074,-8.82303680082656));
#18262=CARTESIAN_POINT('Ctrl Pts',(4.98377226719827,0.242954930756435,-8.82604034862159));
#18263=CARTESIAN_POINT('Ctrl Pts',(4.99192144879532,0.188174105266585,-8.82904389641662));
#18264=CARTESIAN_POINT('Ctrl Pts',(4.996946995993,0.133176700182812,-8.83204744421164));
#18265=CARTESIAN_POINT('Ctrl Pts',(5.0019820280644,0.0780754967619093,-8.83505666069715));
#18266=CARTESIAN_POINT('Ctrl Pts',(5.00388163072279,0.0227574262903489,
-8.83806587718266));
#18267=CARTESIAN_POINT('Ctrl Pts',(5.0026604428803,-0.0323962293808541,
-8.84107509366817));
#18268=CARTESIAN_POINT('Ctrl Pts',(5.001726184208,-0.0745910329373488,-8.84337726742111));
#18269=CARTESIAN_POINT('Ctrl Pts',(4.99896644966508,-0.11668955655156,-8.84567944117405));
#18270=CARTESIAN_POINT('Ctrl Pts',(4.9944081644295,-0.158524180948359,-8.84798161492699));
#18271=CARTESIAN_POINT('Ctrl Pts',(4.98844813431173,-0.213223614723226,
-8.85099174355975));
#18272=CARTESIAN_POINT('Ctrl Pts',(4.97938649241697,-0.267701391859348,
-8.8540018721925));
#18273=CARTESIAN_POINT('Ctrl Pts',(4.96725128751742,-0.321578775980827,
-8.85701200082525));
#18274=CARTESIAN_POINT('Ctrl Pts',(4.95513765029562,-0.375360404812791,
-8.86001677961143));
#18275=CARTESIAN_POINT('Ctrl Pts',(4.93996140571602,-0.428543247190867,
-8.86302155839762));
#18276=CARTESIAN_POINT('Ctrl Pts',(4.92180216318462,-0.480755287203381,
-8.8660263371838));
#18277=CARTESIAN_POINT('Ctrl Pts',(4.90366088621443,-0.532915672054686,
-8.86902814323931));
#18278=CARTESIAN_POINT('Ctrl Pts',(4.88254263007397,-0.584106660785801,
-8.87202994929483));
#18279=CARTESIAN_POINT('Ctrl Pts',(4.85857723478985,-0.633969838600237,
-8.87503175535034));
#18280=CARTESIAN_POINT('Ctrl Pts',(4.8346260835411,-0.683803379813211,-8.87803177725704));
#18281=CARTESIAN_POINT('Ctrl Pts',(4.80783137555879,-0.732310199304294,
-8.88103179916373));
#18282=CARTESIAN_POINT('Ctrl Pts',(4.77837076635551,-0.779152537011243,
-8.88403182107043));
#18283=CARTESIAN_POINT('Ctrl Pts',(4.74891603177336,-0.825985534076756,
-8.88703124475487));
#18284=CARTESIAN_POINT('Ctrl Pts',(4.71679673270429,-0.871154261713097,
-8.89003066843931));
#18285=CARTESIAN_POINT('Ctrl Pts',(4.68223491528552,-0.914348239015901,
-8.89303009212375));
#18286=CARTESIAN_POINT('Ctrl Pts',(4.6476413232743,-0.957581926933696,-8.89603227334446));
#18287=CARTESIAN_POINT('Ctrl Pts',(4.61060105727068,-0.998836824145652,
-8.89903445456518));
#18288=CARTESIAN_POINT('Ctrl Pts',(4.5713767773759,-1.03783518986763,-8.90203663578589));
#18289=CARTESIAN_POINT('Ctrl Pts',(4.53213464345563,-1.07685130678395,-8.90504018353316));
#18290=CARTESIAN_POINT('Ctrl Pts',(4.4907069096717,-1.11360849359802,-8.90804373128042));
#18291=CARTESIAN_POINT('Ctrl Pts',(4.44739104312258,-1.14786789086187,-8.91104727902769));
#18292=CARTESIAN_POINT('Ctrl Pts',(4.40399342515271,-1.18219194698225,-8.91405649546671));
#18293=CARTESIAN_POINT('Ctrl Pts',(4.35870098891423,-1.21400849197432,-8.91706571190573));
#18294=CARTESIAN_POINT('Ctrl Pts',(4.31184106685614,-1.24312145542285,-8.92007492834476));
#18295=CARTESIAN_POINT('Ctrl Pts',(4.27599130227328,-1.26539406792625,-8.92237710248803));
#18296=CARTESIAN_POINT('Ctrl Pts',(4.23922474156701,-1.28608518774481,-8.9246792766313));
#18297=CARTESIAN_POINT('Ctrl Pts',(4.20169648228609,-1.30512577889305,-8.92698145077457));
#18298=CARTESIAN_POINT('Ctrl Pts',(4.15262769724198,-1.3300216491537,-8.92999157941722));
#18299=CARTESIAN_POINT('Ctrl Pts',(4.10204984709073,-1.35219872375596,-8.93300170805987));
#18300=CARTESIAN_POINT('Ctrl Pts',(4.05029545947883,-1.37147355422991,-8.93601183670252));
#18301=CARTESIAN_POINT('Ctrl Pts',(3.99863305400672,-1.39071412789525,-8.93901661549781));
#18302=CARTESIAN_POINT('Ctrl Pts',(3.94579875165924,-1.40706251090148,-8.94202139429311));
#18303=CARTESIAN_POINT('Ctrl Pts',(3.8921476240414,-1.42038211023226,-8.9450261730884));
#18304=CARTESIAN_POINT('Ctrl Pts',(3.83854957533194,-1.43368853202467,-8.94802797915254));
#18305=CARTESIAN_POINT('Ctrl Pts',(3.78413681222264,-1.44397197940106,-8.95102978521668));
#18306=CARTESIAN_POINT('Ctrl Pts',(3.72928046083283,-1.4511453604375,-8.95403159128083));
#18307=CARTESIAN_POINT('Ctrl Pts',(3.67445671378833,-1.45831447791307,-8.95703161319566));
#18308=CARTESIAN_POINT('Ctrl Pts',(3.61919042364834,-1.46237712454633,-8.9600316351105));
#18309=CARTESIAN_POINT('Ctrl Pts',(3.56386154383068,-1.46329754083532,-8.96303165702533));
#18310=CARTESIAN_POINT('Ctrl Pts',(3.50854369693081,-1.46421777358765,-8.9660310807174));
#18311=CARTESIAN_POINT('Ctrl Pts',(3.45316381288654,-1.46199701157743,-8.96903050440947));
#18312=CARTESIAN_POINT('Ctrl Pts',(3.39810325295033,-1.45665157887024,-8.97202992810155));
#18313=CARTESIAN_POINT('Ctrl Pts',(3.34299207280798,-1.45130123181228,-8.97503210932907));
#18314=CARTESIAN_POINT('Ctrl Pts',(3.28820133006719,-1.44282052595289,-8.97803429055658));
#18315=CARTESIAN_POINT('Ctrl Pts',(3.23410715655957,-1.43127768971879,-8.9810364717841));
#18316=CARTESIAN_POINT('Ctrl Pts',(3.17998836058761,-1.41972959944244,-8.98404001953772));
#18317=CARTESIAN_POINT('Ctrl Pts',(3.12656727618178,-1.40511673990528,-8.98704356729135));
#18318=CARTESIAN_POINT('Ctrl Pts',(3.07420648941548,-1.38755773594061,-8.99004711504497));
#18319=CARTESIAN_POINT('Ctrl Pts',(3.02174688047532,-1.36996559231074,-8.99305633148955));
#18320=CARTESIAN_POINT('Ctrl Pts',(2.97035205832455,-1.34941639313374,-8.99606554793413));
#18321=CARTESIAN_POINT('Ctrl Pts',(2.92036509038084,-1.32607715603735,-8.99907476437871));
#18322=CARTESIAN_POINT('Ctrl Pts',(2.88212300839229,-1.30822168179465,-9.00137693845985));
#18323=CARTESIAN_POINT('Ctrl Pts',(2.8447045352404,-1.28873424481411,-9.00367911254098));
#18324=CARTESIAN_POINT('Ctrl Pts',(2.80825223510219,-1.26770702246638,-9.00598128662213));
#18325=CARTESIAN_POINT('Ctrl Pts',(2.76059027961522,-1.24021359868372,-9.00899141542504));
#18326=CARTESIAN_POINT('Ctrl Pts',(2.7143808416501,-1.20997075273178,-9.01200154422795));
#18327=CARTESIAN_POINT('Ctrl Pts',(2.6699592560569,-1.17715674997938,-9.01501167303087));
#18328=CARTESIAN_POINT('Ctrl Pts',(2.62561662012888,-1.14440106694914,-9.01801645198736));
#18329=CARTESIAN_POINT('Ctrl Pts',(2.58305595211978,-1.10908360690832,-9.02102123094385));
#18330=CARTESIAN_POINT('Ctrl Pts',(2.54258566210338,-1.07142711803163,-9.02402600990033));
#18331=CARTESIAN_POINT('Ctrl Pts',(2.50215541073065,-1.03380788400882,-9.02702781612611));
#18332=CARTESIAN_POINT('Ctrl Pts',(2.46381182531109,-0.993854563216969,
-9.03002962235189));
#18333=CARTESIAN_POINT('Ctrl Pts',(2.42783062954249,-0.951830397119265,
-9.03303142857766));
#18334=CARTESIAN_POINT('Ctrl Pts',(2.39187081950476,-0.909831208443431,
-9.03603145065428));
#18335=CARTESIAN_POINT('Ctrl Pts',(2.35827095887694,-0.865764014397917,
-9.0390314727309));
#18336=CARTESIAN_POINT('Ctrl Pts',(2.32726860227162,-0.819927497378155,
-9.04203149480753));
#18337=CARTESIAN_POINT('Ctrl Pts',(2.29627242772731,-0.774100120442426,
-9.04503091866125));
#18338=CARTESIAN_POINT('Ctrl Pts',(2.26787302427423,-0.726504558411053,
-9.04803034251498));
#18339=CARTESIAN_POINT('Ctrl Pts',(2.24226509436996,-0.677469131034583,
-9.05102976636871));
#18340=CARTESIAN_POINT('Ctrl Pts',(2.21663362169899,-0.628388622715184,
-9.05403194775638));
#18341=CARTESIAN_POINT('Ctrl Pts',(2.19379899481406,-0.577866073507391,
-9.05703412914405));
#18342=CARTESIAN_POINT('Ctrl Pts',(2.17390958753799,-0.526253783719348,
-9.06003631053172));
#18343=CARTESIAN_POINT('Ctrl Pts',(2.15401112705056,-0.474618001176516,
-9.06303985844492));
#18344=CARTESIAN_POINT('Ctrl Pts',(2.13706072047535,-0.421891992911413,
-9.06604340635811));
#18345=CARTESIAN_POINT('Ctrl Pts',(2.12315713193944,-0.368444250694168,
-9.06904695427131));
#18346=CARTESIAN_POINT('Ctrl Pts',(2.10922730273489,-0.314895634915433,
-9.0720561708725));
#18347=CARTESIAN_POINT('Ctrl Pts',(2.09835588277445,-0.260623083176926,
-9.0750653874737));
#18348=CARTESIAN_POINT('Ctrl Pts',(2.09059044100075,-0.206005181482704,
-9.0780746040749));
#18349=CARTESIAN_POINT('Ctrl Pts',(2.08464956296263,-0.164220270576309,
-9.08037677687317));
#18350=CARTESIAN_POINT('Ctrl Pts',(2.08052551225042,-0.122233456462208,
-9.08267894967144));
#18351=CARTESIAN_POINT('Ctrl Pts',(2.07821898435105,-0.0802145055345787,
-9.08498112246972));
#18352=CARTESIAN_POINT('Ctrl Pts',(2.07676162205074,-0.0536651475157462,
-9.08643573303217));
#18353=CARTESIAN_POINT('Ctrl Pts',(2.07602773447542,-0.0270757155095218,
-9.08789034359462));
#18354=CARTESIAN_POINT('Ctrl Pts',(2.07601912703142,-0.000473532324670548,
-9.08934495415709));
#18355=CARTESIAN_POINT('Origin',(3.53951905042299,8.32667268468867E-16,
0.));
#18356=CARTESIAN_POINT('',(2.07601932070519,-0.000889446977639352,-9.66065500905984));
#18357=CARTESIAN_POINT('',(2.07601928958954,-0.000836684188483706,-9.58934491816123));
#18358=CARTESIAN_POINT('',(2.07601905042299,1.01189432752408E-15,0.));
#18359=CARTESIAN_POINT('Ctrl Pts',(2.07601932070519,-0.000889446977639352,
-9.66065500905984));
#18360=CARTESIAN_POINT('Ctrl Pts',(2.07605714525543,-0.0631261181238673,
-9.65728432050564));
#18361=CARTESIAN_POINT('Ctrl Pts',(2.08006908018252,-0.125215714240401,
-9.65391363195144));
#18362=CARTESIAN_POINT('Ctrl Pts',(2.08797468161632,-0.186684748669116,
-9.65054294339725));
#18363=CARTESIAN_POINT('Ctrl Pts',(2.09594128600493,-0.248628104091767,
-9.6471462451886));
#18364=CARTESIAN_POINT('Ctrl Pts',(2.10786175311519,-0.309941017617402,
-9.64374954697994));
#18365=CARTESIAN_POINT('Ctrl Pts',(2.12360383412636,-0.370157196687643,
-9.64035284877129));
#18366=CARTESIAN_POINT('Ctrl Pts',(2.13804971351566,-0.425415180655378,
-9.63723583440646));
#18367=CARTESIAN_POINT('Ctrl Pts',(2.1557131111941,-0.479749678775611,-9.63411882004164));
#18368=CARTESIAN_POINT('Ctrl Pts',(2.17645673853775,-0.532816463632704,
-9.63100180567681));
#18369=CARTESIAN_POINT('Ctrl Pts',(2.19648926087477,-0.584064084667966,
-9.62799164458715));
#18370=CARTESIAN_POINT('Ctrl Pts',(2.21945805143587,-0.634288035178362,
-9.62498148349749));
#18371=CARTESIAN_POINT('Ctrl Pts',(2.24523715874897,-0.683130027801967,
-9.62197132240783));
#18372=CARTESIAN_POINT('Ctrl Pts',(2.27097045388209,-0.731885223077252,
-9.61896651069043));
#18373=CARTESIAN_POINT('Ctrl Pts',(2.29950391016743,-0.77926287092397,-9.61596169897304));
#18374=CARTESIAN_POINT('Ctrl Pts',(2.33066355794073,-0.82492463188795,-9.61295688725564));
#18375=CARTESIAN_POINT('Ctrl Pts',(2.36179238148982,-0.87054122262511,-9.60995504800413));
#18376=CARTESIAN_POINT('Ctrl Pts',(2.39554195395406,-0.914444854911577,
-9.60695320875262));
#18377=CARTESIAN_POINT('Ctrl Pts',(2.43169336758349,-0.956323431921016,
-9.60395136950111));
#18378=CARTESIAN_POINT('Ctrl Pts',(2.46782329701041,-0.99817712116705,-9.60095131419429));
#18379=CARTESIAN_POINT('Ctrl Pts',(2.50635189404797,-1.03800774151046,-9.59795125888746));
#18380=CARTESIAN_POINT('Ctrl Pts',(2.5470194855512,-1.07553561713656,-9.59495120358064));
#18381=CARTESIAN_POINT('Ctrl Pts',(2.58767896973404,-1.11305601136284,-9.59195174635226));
#18382=CARTESIAN_POINT('Ctrl Pts',(2.63047621363907,-1.14827421461551,-9.58895228912388));
#18383=CARTESIAN_POINT('Ctrl Pts',(2.67511581404292,-1.18094847259974,-9.58595283189549));
#18384=CARTESIAN_POINT('Ctrl Pts',(2.71979645295554,-1.21365276899853,-9.58295061717711));
#18385=CARTESIAN_POINT('Ctrl Pts',(2.76632240516495,-1.2438081350728,-9.57994840245873));
#18386=CARTESIAN_POINT('Ctrl Pts',(2.81436760856459,-1.27121502365677,-9.57694618774034));
#18387=CARTESIAN_POINT('Ctrl Pts',(2.86243468124854,-1.29863438734743,-9.57394260646957));
#18388=CARTESIAN_POINT('Ctrl Pts',(2.91202190999988,-1.3233025440241,-9.5709390251988));
#18389=CARTESIAN_POINT('Ctrl Pts',(2.96277978240611,-1.34506656590941,-9.56793544392803));
#18390=CARTESIAN_POINT('Ctrl Pts',(3.0136334443206,-1.36687166053588,-9.56492619434299));
#18391=CARTESIAN_POINT('Ctrl Pts',(3.06566166553807,-1.38576149126953,-9.56191694475794));
#18392=CARTESIAN_POINT('Ctrl Pts',(3.1184972736761,-1.4016322319014,-9.55890769517289));
#18393=CARTESIAN_POINT('Ctrl Pts',(3.15891357324997,-1.41377246517289,-9.55660578672501));
#18394=CARTESIAN_POINT('Ctrl Pts',(3.19980192479155,-1.42414712434995,-9.55430387827713));
#18395=CARTESIAN_POINT('Ctrl Pts',(3.24099464769623,-1.43273006214591,-9.55200196982925));
#18396=CARTESIAN_POINT('Ctrl Pts',(3.29486108501997,-1.44395370186281,-9.54899183603887));
#18397=CARTESIAN_POINT('Ctrl Pts',(3.34947453901964,-1.45215886917043,-9.5459817022485));
#18398=CARTESIAN_POINT('Ctrl Pts',(3.4044661220345,-1.45725528186852,-9.54297156845813));
#18399=CARTESIAN_POINT('Ctrl Pts',(3.45935997522778,-1.462342637335,-9.53996678421076));
#18400=CARTESIAN_POINT('Ctrl Pts',(3.51463010223504,-1.46433215387418,-9.5369619999634));
#18401=CARTESIAN_POINT('Ctrl Pts',(3.56989808465953,-1.46318466513248,-9.53395721571603));
#18402=CARTESIAN_POINT('Ctrl Pts',(3.62511139201718,-1.46203831156926,-9.53095540401755));
#18403=CARTESIAN_POINT('Ctrl Pts',(3.68032203359013,-1.4577611112248,-9.52795359231907));
#18404=CARTESIAN_POINT('Ctrl Pts',(3.73514901532542,-1.45036587343755,-9.52495178062059));
#18405=CARTESIAN_POINT('Ctrl Pts',(3.78994341337512,-1.44297503064152,-9.52195175289937));
#18406=CARTESIAN_POINT('Ctrl Pts',(3.84435408118658,-1.43246989372409,-9.51895172517814));
#18407=CARTESIAN_POINT('Ctrl Pts',(3.8980049037048,-1.41891512889137,-9.51595169745692));
#18408=CARTESIAN_POINT('Ctrl Pts',(3.9516450308391,-1.40536306622437,-9.5129522677964));
#18409=CARTESIAN_POINT('Ctrl Pts',(4.00452510176795,-1.38876271229221,-9.50995283813587));
#18410=CARTESIAN_POINT('Ctrl Pts',(4.05628123869077,-1.36922937843763,-9.50695340847535));
#18411=CARTESIAN_POINT('Ctrl Pts',(4.10808496132246,-1.34967808521449,-9.50395122107448));
#18412=CARTESIAN_POINT('Ctrl Pts',(4.15876219025388,-1.32718861140194,-9.50094903367362));
#18413=CARTESIAN_POINT('Ctrl Pts',(4.20796764522582,-1.3019250078657,-9.49794684627275));
#18414=CARTESIAN_POINT('Ctrl Pts',(4.25719549940164,-1.27664990388493,-9.49494329222245));
#18415=CARTESIAN_POINT('Ctrl Pts',(4.30494978790693,-1.24859842076241,-9.49193973817214));
#18416=CARTESIAN_POINT('Ctrl Pts',(4.35091146235571,-1.21797972226881,-9.48893618412183));
#18417=CARTESIAN_POINT('Ctrl Pts',(4.39695988346231,-1.18730323498068,-9.48592696125552));
#18418=CARTESIAN_POINT('Ctrl Pts',(4.44120850857435,-1.15405017116868,-9.48291773838922));
#18419=CARTESIAN_POINT('Ctrl Pts',(4.48336976390905,-1.11847131418372,-9.47990851552291));
#18420=CARTESIAN_POINT('Ctrl Pts',(4.51562412863315,-1.09125264100738,-9.4776063883425));
#18421=CARTESIAN_POINT('Ctrl Pts',(4.54665747809227,-1.06267364596613,-9.4753042611621));
#18422=CARTESIAN_POINT('Ctrl Pts',(4.57635626090245,-1.03286051767176,-9.47300213398169));
#18423=CARTESIAN_POINT('Ctrl Pts',(4.61518852194012,-0.993878745668635,
-9.46999201723103));
#18424=CARTESIAN_POINT('Ctrl Pts',(4.65190093845684,-0.952622063388328,
-9.46698190048036));
#18425=CARTESIAN_POINT('Ctrl Pts',(4.68621633738463,-0.909350087741141,
-9.46397178372969));
#18426=CARTESIAN_POINT('Ctrl Pts',(4.72047074445351,-0.866155023285883,
-9.46096701713148));
#18427=CARTESIAN_POINT('Ctrl Pts',(4.75233626330003,-0.820952184343345,
-9.45796225053327));
#18428=CARTESIAN_POINT('Ctrl Pts',(4.781573323665,-0.774037100093561,-9.45495748393507));
#18429=CARTESIAN_POINT('Ctrl Pts',(4.81078145695544,-0.727168433511017,
-9.45195569024543));
#18430=CARTESIAN_POINT('Ctrl Pts',(4.83736600545975,-0.678591323539135,
-9.4489538965558));
#18431=CARTESIAN_POINT('Ctrl Pts',(4.86112952218744,-0.628631856433107,
-9.44595210286616));
#18432=CARTESIAN_POINT('Ctrl Pts',(4.88487891357995,-0.57870208586682,-9.4429520934807));
#18433=CARTESIAN_POINT('Ctrl Pts',(4.90581037043906,-0.527392062776655,
-9.43995208409524));
#18434=CARTESIAN_POINT('Ctrl Pts',(4.92377254285713,-0.475052122070712,
-9.43695207470978));
#18435=CARTESIAN_POINT('Ctrl Pts',(4.94173113269943,-0.422722620625602,
-9.43395266367961));
#18436=CARTESIAN_POINT('Ctrl Pts',(4.95672144290561,-0.369364108760113,
-9.43095325264944));
#18437=CARTESIAN_POINT('Ctrl Pts',(4.96864122643677,-0.315344345161995,
-9.42795384161927));
#18438=CARTESIAN_POINT('Ctrl Pts',(4.98057196811161,-0.261274919895944,
-9.42495167315839));
#18439=CARTESIAN_POINT('Ctrl Pts',(4.98942642946449,-0.206543545206128,
-9.42194950469752));
#18440=CARTESIAN_POINT('Ctrl Pts',(4.99515334565316,-0.151529035335643,
-9.41894733623665));
#18441=CARTESIAN_POINT('Ctrl Pts',(5.00088286846927,-0.0964894854041399,
-9.41594380132752));
#18442=CARTESIAN_POINT('Ctrl Pts',(5.00348198361674,-0.0411670718573775,
-9.41294026641838));
#18443=CARTESIAN_POINT('Ctrl Pts',(5.00295154250228,0.0140567110877411,
-9.40993673150925));
#18444=CARTESIAN_POINT('Ctrl Pts',(5.0024201002595,0.0693847206689516,-9.40692752787691));
#18445=CARTESIAN_POINT('Ctrl Pts',(4.99874733759426,0.124613199534061,-9.40391832424457));
#18446=CARTESIAN_POINT('Ctrl Pts',(4.99198616106228,0.179364273229523,-9.40090912061223));
#18447=CARTESIAN_POINT('Ctrl Pts',(4.98681333664813,0.22125309085957,-9.39860684645286));
#18448=CARTESIAN_POINT('Ctrl Pts',(4.97983381238854,0.262862521635656,-9.39630457229348));
#18449=CARTESIAN_POINT('Ctrl Pts',(4.97109123950477,0.304028481309916,-9.39400229813412));
#18450=CARTESIAN_POINT('Ctrl Pts',(4.95966066485512,0.357851375478105,-9.39099216404745));
#18451=CARTESIAN_POINT('Ctrl Pts',(4.94516648060807,0.411141823506292,-9.38798202996078));
#18452=CARTESIAN_POINT('Ctrl Pts',(4.92767468155269,0.46352582858229,-9.38497189587411));
#18453=CARTESIAN_POINT('Ctrl Pts',(4.91021396976422,0.515816734283992,-9.38196711154258));
#18454=CARTESIAN_POINT('Ctrl Pts',(4.8897663815523,0.567203897148697,-9.37896232721104));
#18455=CARTESIAN_POINT('Ctrl Pts',(4.86644853509855,0.617325192016863,-9.37595754287951));
#18456=CARTESIAN_POINT('Ctrl Pts',(4.84315375734608,0.667396901123263,-9.37295573122696));
#18457=CARTESIAN_POINT('Ctrl Pts',(4.81699456811533,0.716204746586315,-9.36995391957441));
#18458=CARTESIAN_POINT('Ctrl Pts',(4.78813619375466,0.763405186895047,-9.36695210792186));
#18459=CARTESIAN_POINT('Ctrl Pts',(4.75929497118225,0.81057757392719,-9.36395208037666));
#18460=CARTESIAN_POINT('Ctrl Pts',(4.72775801812582,0.856143999701005,-9.36095205283147));
#18461=CARTESIAN_POINT('Ctrl Pts',(4.69373605686976,0.899786281307431,-9.35795202528627));
#18462=CARTESIAN_POINT('Ctrl Pts',(4.65972087942777,0.943419860854571,-9.35495259593202));
#18463=CARTESIAN_POINT('Ctrl Pts',(4.62322200233724,0.985129641903256,-9.35195316657776));
#18464=CARTESIAN_POINT('Ctrl Pts',(4.58449157015024,1.02462904654069,-9.3489537372235));
#18465=CARTESIAN_POINT('Ctrl Pts',(4.54572553095928,1.06416476514049,-9.34595155032985));
#18466=CARTESIAN_POINT('Ctrl Pts',(4.50472420839937,1.10148566952206,-9.34294936343619));
#18467=CARTESIAN_POINT('Ctrl Pts',(4.46177686261144,1.13634184023003,-9.33994717654253));
#18468=CARTESIAN_POINT('Ctrl Pts',(4.41880996802786,1.17121387678829,-9.33694362311185));
#18469=CARTESIAN_POINT('Ctrl Pts',(4.37389571347937,1.20361863370915,-9.33394006968117));
#18470=CARTESIAN_POINT('Ctrl Pts',(4.32735407960895,1.2333483760834,-9.33093651625049));
#18471=CARTESIAN_POINT('Ctrl Pts',(4.28072460722553,1.26313422771178,-9.32792729418196));
#18472=CARTESIAN_POINT('Ctrl Pts',(4.23246208159446,1.2902347202587,-9.32491807211343));
#18473=CARTESIAN_POINT('Ctrl Pts',(4.18291189430237,1.31448769429189,-9.32190885004491));
#18474=CARTESIAN_POINT('Ctrl Pts',(4.14500477643329,1.33304181881886,-9.31960672079213));
#18475=CARTESIAN_POINT('Ctrl Pts',(4.1063445805378,1.34993033667301,-9.31730459153935));
#18476=CARTESIAN_POINT('Ctrl Pts',(4.06709255049389,1.3651001619013,-9.31500246228657));
#18477=CARTESIAN_POINT('Ctrl Pts',(4.01576890418584,1.38493533332302,-9.3119923334501));
#18478=CARTESIAN_POINT('Ctrl Pts',(3.9632172527145,1.401913734746,-9.30898220461363));
#18479=CARTESIAN_POINT('Ctrl Pts',(3.90978688627271,1.41588628771352,-9.30597207577716));
#18480=CARTESIAN_POINT('Ctrl Pts',(3.8564514800765,1.4298340076666,-9.30296729675565));
#18481=CARTESIAN_POINT('Ctrl Pts',(3.80224096494489,1.44078634827748,-9.29996251773414));
#18482=CARTESIAN_POINT('Ctrl Pts',(3.74752234880744,1.44864311611287,-9.29695773871262));
#18483=CARTESIAN_POINT('Ctrl Pts',(3.69285786731907,1.45649211102927,-9.29395593240258));
#18484=CARTESIAN_POINT('Ctrl Pts',(3.63768680079154,1.46125152521657,-9.29095412609254));
#18485=CARTESIAN_POINT('Ctrl Pts',(3.58238715228655,1.46287202989278,-9.2879523197825));
#18486=CARTESIAN_POINT('Ctrl Pts',(3.52712037124722,1.46449157141853,-9.28495229760253));
#18487=CARTESIAN_POINT('Ctrl Pts',(3.47172568654132,1.46297588577145,-9.28195227542256));
#18488=CARTESIAN_POINT('Ctrl Pts',(3.41658472162056,1.45832760407321,-9.27895225324259));
#18489=CARTESIAN_POINT('Ctrl Pts',(3.36145475179931,1.45368024924159,-9.27595282926656));
#18490=CARTESIAN_POINT('Ctrl Pts',(3.30657892724477,1.44590158320243,-9.27295340529053));
#18491=CARTESIAN_POINT('Ctrl Pts',(3.25233503441008,1.43504619819248,-9.2699539813145));
#18492=CARTESIAN_POINT('Ctrl Pts',(3.19804127169103,1.42418083313194,-9.26695179977593));
#18493=CARTESIAN_POINT('Ctrl Pts',(3.14438112036593,1.41023320173145,-9.26394961823736));
#18494=CARTESIAN_POINT('Ctrl Pts',(3.09172194430631,1.39330901158125,-9.26094743669879));
#18495=CARTESIAN_POINT('Ctrl Pts',(3.03903879869131,1.37637711782945,-9.25794388861859));
#18496=CARTESIAN_POINT('Ctrl Pts',(2.98735803026844,1.35646615466497,-9.25494034053838));
#18497=CARTESIAN_POINT('Ctrl Pts',(2.93702845779043,1.33373060840234,-9.25193679245818));
#18498=CARTESIAN_POINT('Ctrl Pts',(2.88660389636236,1.3109521524633,-9.24892757566543));
#18499=CARTESIAN_POINT('Ctrl Pts',(2.83753609454638,1.28533870902024,-9.24591835887269));
#18500=CARTESIAN_POINT('Ctrl Pts',(2.79014958485059,1.25709094900398,-9.24290914207994));
#18501=CARTESIAN_POINT('Ctrl Pts',(2.75389699899805,1.23548027643693,-9.24060697019963));
#18502=CARTESIAN_POINT('Ctrl Pts',(2.71862795991674,1.21232874178303,-9.23830479831931));
#18503=CARTESIAN_POINT('Ctrl Pts',(2.68447503902291,1.18774239150115,-9.236002626439));
#18504=CARTESIAN_POINT('Ctrl Pts',(2.63790054159497,1.15421387101162,-9.23286314391416));
#18505=CARTESIAN_POINT('Ctrl Pts',(2.59319110532703,1.11786235311868,-9.22972366138932));
#18506=CARTESIAN_POINT('Ctrl Pts',(2.55070897341634,1.07892858040285,-9.22658417886449));
#18507=CARTESIAN_POINT('Ctrl Pts',(2.51033977708129,1.04193125837264,-9.22360084491359));
#18508=CARTESIAN_POINT('Ctrl Pts',(2.47198205987822,1.00260285108754,-9.2206175109627));
#18509=CARTESIAN_POINT('Ctrl Pts',(2.43591635001457,0.961193700380545,-9.2176341770118));
#18510=CARTESIAN_POINT('Ctrl Pts',(2.39988516651582,0.919824191412278,-9.21465369906116));
#18511=CARTESIAN_POINT('Ctrl Pts',(2.36614199649358,0.876378285783741,-9.21167322111052));
#18512=CARTESIAN_POINT('Ctrl Pts',(2.33493064869678,0.831143208133652,-9.20869274315988));
#18513=CARTESIAN_POINT('Ctrl Pts',(2.30373639736095,0.785932908642596,-9.20571389780855));
#18514=CARTESIAN_POINT('Ctrl Pts',(2.27507152439762,0.73893581989652,-9.20273505245723));
#18515=CARTESIAN_POINT('Ctrl Pts',(2.24913812526181,0.690470359957754,-9.1997562071059));
#18516=CARTESIAN_POINT('Ctrl Pts',(2.22320831111068,0.642011599793678,-9.19677777354459));
#18517=CARTESIAN_POINT('Ctrl Pts',(2.2000094727482,0.592085344999108,-9.19379933998328));
#18518=CARTESIAN_POINT('Ctrl Pts',(2.17969790159473,0.541034835476783,-9.19082090642197));
#18519=CARTESIAN_POINT('Ctrl Pts',(2.15936755744828,0.489937142462359,-9.18783972004002));
#18520=CARTESIAN_POINT('Ctrl Pts',(2.14193000421592,0.437713620569443,-9.18485853365807));
#18521=CARTESIAN_POINT('Ctrl Pts',(2.1274928285188,0.384726134613917,-9.18187734727612));
#18522=CARTESIAN_POINT('Ctrl Pts',(2.11304788526616,0.331710140088062,-9.17889455694259));
#18523=CARTESIAN_POINT('Ctrl Pts',(2.10160664299598,0.27792988860327,-9.17591176660907));
#18524=CARTESIAN_POINT('Ctrl Pts',(2.09322560589289,0.223757731283741,-9.17292897627554));
#18525=CARTESIAN_POINT('Ctrl Pts',(2.08483022592481,0.16949286659056,-9.16994108135192));
#18526=CARTESIAN_POINT('Ctrl Pts',(2.07950554880692,0.114835291698482,-9.16695318642829));
#18527=CARTESIAN_POINT('Ctrl Pts',(2.07725611812157,0.0601611736690593,
-9.16396529150466));
#18528=CARTESIAN_POINT('Ctrl Pts',(2.07642541419144,0.0399702849170984,
-9.16286187628408));
#18529=CARTESIAN_POINT('Ctrl Pts',(2.076013596649,0.019777117921205,-9.1617584610635));
#18530=CARTESIAN_POINT('Ctrl Pts',(2.07601910496125,-0.000399541592406468,
-9.16065504584292));
#18531=CARTESIAN_POINT('Ctrl Pts',(2.07601912703111,-0.000473531363085116,
-9.08934495420967));
#18532=CARTESIAN_POINT('Ctrl Pts',(2.07600072508622,0.0563996707828281,
-9.09245478771415));
#18533=CARTESIAN_POINT('Ctrl Pts',(2.07930259651659,0.113405113069047,-9.09556462121863));
#18534=CARTESIAN_POINT('Ctrl Pts',(2.08594013758935,0.170119352706743,-9.09867445472312));
#18535=CARTESIAN_POINT('Ctrl Pts',(2.0922999035551,0.22446015257039,-9.10165414450043));
#18536=CARTESIAN_POINT('Ctrl Pts',(2.10172163808173,0.278533036092905,-9.10463383427774));
#18537=CARTESIAN_POINT('Ctrl Pts',(2.11416586932496,0.331964695613464,-9.10761352405505));
#18538=CARTESIAN_POINT('Ctrl Pts',(2.12659876553803,0.385347686039009,-9.11059049973352));
#18539=CARTESIAN_POINT('Ctrl Pts',(2.14204858610979,0.438090087384239,-9.11356747541199));
#18540=CARTESIAN_POINT('Ctrl Pts',(2.16042447852284,0.489826920202991,-9.11654445109047));
#18541=CARTESIAN_POINT('Ctrl Pts',(2.17879119649404,0.541537922626467,-9.11951994046887));
#18542=CARTESIAN_POINT('Ctrl Pts',(2.20008091182603,0.59224384532183,-9.12249542984727));
#18543=CARTESIAN_POINT('Ctrl Pts',(2.22415311018739,0.641595428029321,-9.12547091922567));
#18544=CARTESIAN_POINT('Ctrl Pts',(2.24822319763209,0.69094268304404,-9.12844614768024));
#18545=CARTESIAN_POINT('Ctrl Pts',(2.27507504589748,0.738935351725389,-9.13142137613481));
#18546=CARTESIAN_POINT('Ctrl Pts',(2.30452128333745,0.785246945421463,-9.13439660458939));
#18547=CARTESIAN_POINT('Ctrl Pts',(2.33399651661026,0.831604142337015,-9.13737476276382));
#18548=CARTESIAN_POINT('Ctrl Pts',(2.36607094607567,0.876276507662001,-9.14035292093826));
#18549=CARTESIAN_POINT('Ctrl Pts',(2.40051369859436,0.918966298895521,-9.1433310791127));
#18550=CARTESIAN_POINT('Ctrl Pts',(2.43497662413391,0.961681093416718,-9.1463109815858));
#18551=CARTESIAN_POINT('Ctrl Pts',(2.47181027029991,1.00241060609859,-9.1492908840589));
#18552=CARTESIAN_POINT('Ctrl Pts',(2.5107455181391,1.04089253492959,-9.152270786532));
#18553=CARTESIAN_POINT('Ctrl Pts',(2.54974830824503,1.07944121963979,-9.15525585834083));
#18554=CARTESIAN_POINT('Ctrl Pts',(2.59085956673665,1.11573419130838,-9.15824093014965));
#18555=CARTESIAN_POINT('Ctrl Pts',(2.63377688597688,1.14954920797001,-9.16122600195848));
#18556=CARTESIAN_POINT('Ctrl Pts',(2.64697984491329,1.1599519610851,-9.16214432074474));
#18557=CARTESIAN_POINT('Ctrl Pts',(2.66035352883006,1.1701205127387,-9.163062639531));
#18558=CARTESIAN_POINT('Ctrl Pts',(2.67388862910717,1.18004924629975,-9.16398095831725));
#18559=CARTESIAN_POINT('Ctrl Pts',(2.71825491382426,1.2125943335936,-9.16699108693825));
#18560=CARTESIAN_POINT('Ctrl Pts',(2.76455236415568,1.2427022655566,-9.17000121555925));
#18561=CARTESIAN_POINT('Ctrl Pts',(2.81248271675935,1.27013795295351,-9.17301134418025));
#18562=CARTESIAN_POINT('Ctrl Pts',(2.86032788355696,1.29752487936664,-9.17601612295049));
#18563=CARTESIAN_POINT('Ctrl Pts',(2.9097997386984,1.32224872606603,-9.17902090172074));
#18564=CARTESIAN_POINT('Ctrl Pts',(2.96057015433098,1.34411696876196,-9.18202568049099));
#18565=CARTESIAN_POINT('Ctrl Pts',(3.01129034100766,1.3659635764371,-9.18502748652803));
#18566=CARTESIAN_POINT('Ctrl Pts',(3.06330606057254,1.3849599687024,-9.18802929256507));
#18567=CARTESIAN_POINT('Ctrl Pts',(3.11626529340335,1.40095985209026,-9.19103109860211));
#18568=CARTESIAN_POINT('Ctrl Pts',(3.16919304942238,1.41695022579886,-9.19403112048786));
#18569=CARTESIAN_POINT('Ctrl Pts',(3.22306270265424,1.42994746826493,-9.19703114237362));
#18570=CARTESIAN_POINT('Ctrl Pts',(3.2775051748386,1.4398544992468,-9.20003116425937));
#18571=CARTESIAN_POINT('Ctrl Pts',(3.33193679082557,1.44975955469964,-9.20303058792045));
#18572=CARTESIAN_POINT('Ctrl Pts',(3.38694047962898,1.45657552793621,-9.20603001158154));
#18573=CARTESIAN_POINT('Ctrl Pts',(3.44213730285502,1.46025649981112,-9.20902943524262));
#18574=CARTESIAN_POINT('Ctrl Pts',(3.49738487151301,1.46394085580302,-9.21203161643648));
#18575=CARTESIAN_POINT('Ctrl Pts',(3.55282540125534,1.46448441700218,-9.21503379763035));
#18576=CARTESIAN_POINT('Ctrl Pts',(3.60807667158193,1.4618933280445,-9.21803597882421));
#18577=CARTESIAN_POINT('Ctrl Pts',(3.66335309102968,1.45930105968208,-9.22103952654265));
#18578=CARTESIAN_POINT('Ctrl Pts',(3.71843955313624,1.45357135162408,-9.22404307426108));
#18579=CARTESIAN_POINT('Ctrl Pts',(3.77295900615846,1.44476227700831,-9.22704662197952));
#18580=CARTESIAN_POINT('Ctrl Pts',(3.82758135543828,1.43593657675231,-9.23005583838688));
#18581=CARTESIAN_POINT('Ctrl Pts',(3.88163404087832,1.42402001397532,-9.23306505479425));
#18582=CARTESIAN_POINT('Ctrl Pts',(3.93475139873487,1.40912158483499,-9.23607427120162));
#18583=CARTESIAN_POINT('Ctrl Pts',(3.97538836221842,1.39772367376847,-9.23837644552268));
#18584=CARTESIAN_POINT('Ctrl Pts',(4.01547811093556,1.38458157483124,-9.24067861984375));
#18585=CARTESIAN_POINT('Ctrl Pts',(4.0548649868777,1.3697630509616,-9.24298079416481));
#18586=CARTESIAN_POINT('Ctrl Pts',(4.10636395406392,1.35038759514652,-9.24599092373162));
#18587=CARTESIAN_POINT('Ctrl Pts',(4.15687691820343,1.32806308232201,-9.24900105329842));
#18588=CARTESIAN_POINT('Ctrl Pts',(4.20604401566905,1.30291086445073,-9.25201118286523));
#18589=CARTESIAN_POINT('Ctrl Pts',(4.2551237294341,1.27780334911404,-9.25501596258886));
#18590=CARTESIAN_POINT('Ctrl Pts',(4.30286185706654,1.24987834069035,-9.25802074231249));
#18591=CARTESIAN_POINT('Ctrl Pts',(4.34891786639811,1.21930546078416,-9.26102552203612));
#18592=CARTESIAN_POINT('Ctrl Pts',(4.39492831097592,1.18876282765282,-9.26402732903046));
#18593=CARTESIAN_POINT('Ctrl Pts',(4.43925949607256,1.15557780303837,-9.26702913602479));
#18594=CARTESIAN_POINT('Ctrl Pts',(4.48159655472588,1.11996527887539,-9.27003094301913));
#18595=CARTESIAN_POINT('Ctrl Pts',(4.52390844999407,1.0843739213142,-9.27303096586436));
#18596=CARTESIAN_POINT('Ctrl Pts',(4.56422816467261,1.04635826321566,-9.27603098870958));
#18597=CARTESIAN_POINT('Ctrl Pts',(4.60227272843954,1.00617437348717,-9.2790310115548));
#18598=CARTESIAN_POINT('Ctrl Pts',(4.6403097058712,0.965998496689559,-9.28203043617582));
#18599=CARTESIAN_POINT('Ctrl Pts',(4.67607207049773,0.923655630197818,-9.28502986079683));
#18600=CARTESIAN_POINT('Ctrl Pts',(4.70931431326071,0.879438055261666,-9.28802928541785));
#18601=CARTESIAN_POINT('Ctrl Pts',(4.74258711733265,0.8351798288274,-9.29103146756468));
#18602=CARTESIAN_POINT('Ctrl Pts',(4.77333485268551,0.789043873624383,-9.29403364971151));
#18603=CARTESIAN_POINT('Ctrl Pts',(4.80135382175268,0.741353667194913,-9.29703583185834));
#18604=CARTESIAN_POINT('Ctrl Pts',(4.82938554439063,0.693641753313561,-9.30003938052734));
#18605=CARTESIAN_POINT('Ctrl Pts',(4.85468578308905,0.644374648546172,-9.30304292919634));
#18606=CARTESIAN_POINT('Ctrl Pts',(4.87709715598709,0.593899874992042,-9.30604647786535));
#18607=CARTESIAN_POINT('Ctrl Pts',(4.89955082643404,0.543329839125654,-9.30905569520745));
#18608=CARTESIAN_POINT('Ctrl Pts',(4.91910455238094,0.491548076564944,-9.31206491254955));
#18609=CARTESIAN_POINT('Ctrl Pts',(4.93564982372366,0.438920395792753,-9.31507412989166));
#18610=CARTESIAN_POINT('Ctrl Pts',(4.94830759101384,0.39865820108846,-9.31737629659856));
#18611=CARTESIAN_POINT('Ctrl Pts',(4.95920556962158,0.357901299559934,-9.31967846330547));
#18612=CARTESIAN_POINT('Ctrl Pts',(4.96831546214218,0.31681708264922,-9.32198063001237));
#18613=CARTESIAN_POINT('Ctrl Pts',(4.9802268205484,0.263098684615905,-9.32499075693701));
#18614=CARTESIAN_POINT('Ctrl Pts',(4.98912952154896,0.208594737591463,-9.32800088386164));
#18615=CARTESIAN_POINT('Ctrl Pts',(4.99492857241083,0.15367294266439,-9.33101101078628));
#18616=CARTESIAN_POINT('Ctrl Pts',(5.00071731673245,0.0988487591746224,
-9.33401578787091));
#18617=CARTESIAN_POINT('Ctrl Pts',(5.00341330256137,0.0436087224915531,
-9.33702056495555));
#18618=CARTESIAN_POINT('Ctrl Pts',(5.00297252691122,-0.0116692825189981,
-9.34002534204018));
#18619=CARTESIAN_POINT('Ctrl Pts',(5.00253218733501,-0.0668925991702068,
-9.34302714639943));
#18620=CARTESIAN_POINT('Ctrl Pts',(4.99896123796156,-0.122153284234078,
-9.34602895075867));
#18621=CARTESIAN_POINT('Ctrl Pts',(4.99226761429001,-0.17707021257766,-9.34903075511791));
#18622=CARTESIAN_POINT('Ctrl Pts',(4.98557796901429,-0.231954500711812,
-9.35203077533652));
#18623=CARTESIAN_POINT('Ctrl Pts',(4.97576939188507,-0.286494913898792,
-9.35503079555514));
#18624=CARTESIAN_POINT('Ctrl Pts',(4.96290173342562,-0.34031454234024,-9.35803081577376));
#18625=CARTESIAN_POINT('Ctrl Pts',(4.95003664080778,-0.394123439020127,
-9.36103023778123));
#18626=CARTESIAN_POINT('Ctrl Pts',(4.93411380100649,-0.447211323036412,
-9.3640296597887));
#18627=CARTESIAN_POINT('Ctrl Pts',(4.91524386204612,-0.499212873115784,
-9.36702908179617));
#18628=CARTESIAN_POINT('Ctrl Pts',(4.89635657470561,-0.551262231651783,
-9.37003126137023));
#18629=CARTESIAN_POINT('Ctrl Pts',(4.87451695558412,-0.602222763392148,
-9.37303344094428));
#18630=CARTESIAN_POINT('Ctrl Pts',(4.84988462607803,-0.651747119777476,
-9.37603562051834));
#18631=CARTESIAN_POINT('Ctrl Pts',(4.82524108435636,-0.701294018803769,
-9.37903916663325));
#18632=CARTESIAN_POINT('Ctrl Pts',(4.79780256031205,-0.749402979776172,
-9.38204271274816));
#18633=CARTESIAN_POINT('Ctrl Pts',(4.76777412001656,-0.795752306950904,
-9.38504625886307));
#18634=CARTESIAN_POINT('Ctrl Pts',(4.73768900561841,-0.842189111413878,
-9.38805547371333));
#18635=CARTESIAN_POINT('Ctrl Pts',(4.70500452290369,-0.886859220529012,
-9.39106468856358));
#18636=CARTESIAN_POINT('Ctrl Pts',(4.66996775660819,-0.929471878371908,
-9.39407390341384));
#18637=CARTESIAN_POINT('Ctrl Pts',(4.64316302222061,-0.96207251752321,-9.39637609089587));
#18638=CARTESIAN_POINT('Ctrl Pts',(4.61498239082923,-0.993469570782487,
-9.3986782783779));
#18639=CARTESIAN_POINT('Ctrl Pts',(4.58555059930908,-1.02354787320133,-9.40098046585993));
#18640=CARTESIAN_POINT('Ctrl Pts',(4.54706829075826,-1.06287550004913,-9.40399059485479));
#18641=CARTESIAN_POINT('Ctrl Pts',(4.5062841429003,-1.10011251335244,-9.40700072384964));
#18642=CARTESIAN_POINT('Ctrl Pts',(4.46345421198909,-1.13497844350535,-9.4100108528445));
#18643=CARTESIAN_POINT('Ctrl Pts',(4.42070040231218,-1.16978240676777,-9.41301563196533));
#18644=CARTESIAN_POINT('Ctrl Pts',(4.37590843140498,-1.20222331908433,-9.41602041108617));
#18645=CARTESIAN_POINT('Ctrl Pts',(4.32937074529078,-1.23205785177258,-9.41902519020701));
#18646=CARTESIAN_POINT('Ctrl Pts',(4.28287910076274,-1.26186286796954,-9.4220269965802));
#18647=CARTESIAN_POINT('Ctrl Pts',(4.23464560475323,-1.28906632898799,-9.4250288029534));
#18648=CARTESIAN_POINT('Ctrl Pts',(4.1849937960761,-1.313466635558,-9.42803060932659));
#18649=CARTESIAN_POINT('Ctrl Pts',(4.13537149865489,-1.33785243946011,-9.43103063153364));
#18650=CARTESIAN_POINT('Ctrl Pts',(4.08433303246491,-1.35943815876272,-9.43403065374068));
#18651=CARTESIAN_POINT('Ctrl Pts',(4.03222677203278,-1.37806797766514,-9.43703067594773));
#18652=CARTESIAN_POINT('Ctrl Pts',(3.98013090220608,-1.39669408156103,-9.44003009991482));
#18653=CARTESIAN_POINT('Ctrl Pts',(3.92696815801702,-1.41236527796435,-9.44302952388191));
#18654=CARTESIAN_POINT('Ctrl Pts',(3.87310496385929,-1.42497462726775,-9.446028947849));
#18655=CARTESIAN_POINT('Ctrl Pts',(3.81919225081428,-1.43759556892019,-9.44903112932313));
#18656=CARTESIAN_POINT('Ctrl Pts',(3.76457831657979,-1.44714891904127,-9.45203331079727));
#18657=CARTESIAN_POINT('Ctrl Pts',(3.70964129179006,-1.45357857475688,-9.4550354922714));
#18658=CARTESIAN_POINT('Ctrl Pts',(3.65467926117246,-1.46001115707553,-9.45803904025625));
#18659=CARTESIAN_POINT('Ctrl Pts',(3.59939437493514,-1.4633171791083,-9.4610425882411));
#18660=CARTESIAN_POINT('Ctrl Pts',(3.5441681096177,-1.46349261571373,-9.46404613622595));
#18661=CARTESIAN_POINT('Ctrl Pts',(3.48883761453575,-1.46366838342457,-9.46705535287403));
#18662=CARTESIAN_POINT('Ctrl Pts',(3.43356649003813,-1.46070179108835,-9.4700645695221));
#18663=CARTESIAN_POINT('Ctrl Pts',(3.37873325859932,-1.45464091072252,-9.47307378617018));
#18664=CARTESIAN_POINT('Ctrl Pts',(3.33678362971101,-1.45000409331432,-9.47537595801595));
#18665=CARTESIAN_POINT('Ctrl Pts',(3.2950902483301,-1.44355731500171,-9.47767812986172));
#18666=CARTESIAN_POINT('Ctrl Pts',(3.25381772053166,-1.43534211953051,-9.4799803017075));
#18667=CARTESIAN_POINT('Ctrl Pts',(3.19985309155182,-1.42460059243613,-9.48299043595737));
#18668=CARTESIAN_POINT('Ctrl Pts',(3.14638169686634,-1.41078889917564,-9.48600057020725));
#18669=CARTESIAN_POINT('Ctrl Pts',(3.09377834646457,-1.39396824742698,-9.48901070445713));
#18670=CARTESIAN_POINT('Ctrl Pts',(3.04126848630545,-1.37717749048163,-9.49201548889222));
#18671=CARTESIAN_POINT('Ctrl Pts',(2.98962410779196,-1.3573885471936,-9.49502027332732));
#18672=CARTESIAN_POINT('Ctrl Pts',(2.93920879747361,-1.33471339627796,-9.49802505776242));
#18673=CARTESIAN_POINT('Ctrl Pts',(2.88884336440228,-1.31206067851003,-9.501026869482));
#18674=CARTESIAN_POINT('Ctrl Pts',(2.83970507005814,-1.28652762509496,-9.50402868120157));
#18675=CARTESIAN_POINT('Ctrl Pts',(2.79213954034621,-1.25827505654264,-9.50703049292115));
#18676=CARTESIAN_POINT('Ctrl Pts',(2.74460228147621,-1.23003928006442,-9.51003052049693));
#18677=CARTESIAN_POINT('Ctrl Pts',(2.69863638759028,-1.19908746133809,-9.51303054807271));
#18678=CARTESIAN_POINT('Ctrl Pts',(2.65456270975754,-1.16562623731452,-9.51603057564849));
#18679=CARTESIAN_POINT('Ctrl Pts',(2.61049782053701,-1.13217168570262,-9.51903000499694));
#18680=CARTESIAN_POINT('Ctrl Pts',(2.56832481841323,-1.09620904171744,-9.52202943434538));
#18681=CARTESIAN_POINT('Ctrl Pts',(2.52833348165112,-1.05798676527993,-9.52502886369382));
#18682=CARTESIAN_POINT('Ctrl Pts',(2.48830537941433,-1.01972934972857,-9.52803105052558));
#18683=CARTESIAN_POINT('Ctrl Pts',(2.45046333223626,-0.979208517103823,
-9.53103323735734));
#18684=CARTESIAN_POINT('Ctrl Pts',(2.41506093746071,-0.93671030857641,-9.53403542418909));
#18685=CARTESIAN_POINT('Ctrl Pts',(2.37964242857244,-0.894192756133781,
-9.53703897752663));
#18686=CARTESIAN_POINT('Ctrl Pts',(2.346666100702,-0.849696458651381,-9.54004253086416));
#18687=CARTESIAN_POINT('Ctrl Pts',(2.31634376287682,-0.803538714646867,
-9.54304608420169));
#18688=CARTESIAN_POINT('Ctrl Pts',(2.28596419788774,-0.757293857412609,
-9.54605530612718));
#18689=CARTESIAN_POINT('Ctrl Pts',(2.25824889400525,-0.709381747993645,
-9.54906452805268));
#18690=CARTESIAN_POINT('Ctrl Pts',(2.23336441339684,-0.660145676479889,
-9.55207374997818));
#18691=CARTESIAN_POINT('Ctrl Pts',(2.21432717032797,-0.622478864143564,
-9.55437587917048));
#18692=CARTESIAN_POINT('Ctrl Pts',(2.19694576991218,-0.584037740428541,
-9.55667800836277));
#18693=CARTESIAN_POINT('Ctrl Pts',(2.18127535534639,-0.544982857330992,
-9.55898013755507));
#18694=CARTESIAN_POINT('Ctrl Pts',(2.15828431881751,-0.487683017549696,
-9.56235773398892));
#18695=CARTESIAN_POINT('Ctrl Pts',(2.1388962543463,-0.428859532790245,-9.56573533042276));
#18696=CARTESIAN_POINT('Ctrl Pts',(2.12328935970264,-0.368952182704129,
-9.56911292685661));
#18697=CARTESIAN_POINT('Ctrl Pts',(2.10770833125499,-0.309144120483749,
-9.57248492540738));
#18698=CARTESIAN_POINT('Ctrl Pts',(2.09589612654762,-0.24825603324965,-9.57585692395815));
#18699=CARTESIAN_POINT('Ctrl Pts',(2.08798271930862,-0.186747234129522,
-9.57922892250892));
#18700=CARTESIAN_POINT('Ctrl Pts',(2.08006931206962,-0.125238435009388,
-9.5826009210597));
#18701=CARTESIAN_POINT('Ctrl Pts',(2.07605489084021,-0.0631091910183387,
-9.58597291961046));
#18702=CARTESIAN_POINT('Ctrl Pts',(2.07601928958954,-0.000836684188483706,
-9.58934491816123));
#18703=CARTESIAN_POINT('Origin',(3.53951905042299,8.32667268468867E-16,
0.));
#18704=CARTESIAN_POINT('',(2.07692213061801,0.00132420044191561,-10.1606550458429));
#18705=CARTESIAN_POINT('',(2.07677307172911,0.00126791318965598,-10.0893449541571));
#18706=CARTESIAN_POINT('',(2.07601905042299,1.01189432752408E-15,0.));
#18707=CARTESIAN_POINT('Ctrl Pts',(2.07692213061801,0.00132420044191561,
-10.1606550458429));
#18708=CARTESIAN_POINT('Ctrl Pts',(2.07968635796469,-0.340292586538367,
-10.1421036374827));
#18709=CARTESIAN_POINT('Ctrl Pts',(2.3686807329946,-1.17120535538033,-10.0972189505064));
#18710=CARTESIAN_POINT('Ctrl Pts',(3.74854525128539,-1.71419019754643,-10.0260009849147));
#18711=CARTESIAN_POINT('Ctrl Pts',(5.08944937204478,-0.761677757650357,
-9.94700114906702));
#18712=CARTESIAN_POINT('Ctrl Pts',(5.02430011578218,0.881991624007174,-9.86800131321952));
#18713=CARTESIAN_POINT('Ctrl Pts',(3.6121165985489,1.72542879024637,-9.78900147737193));
#18714=CARTESIAN_POINT('Ctrl Pts',(2.31901753288414,1.09390323182268,-9.71988605491308));
#18715=CARTESIAN_POINT('Ctrl Pts',(2.07948494644385,0.302460268914583,-9.67710391107006));
#18716=CARTESIAN_POINT('Ctrl Pts',(2.07778482844489,-0.000887695637598399,
-9.66065504584291));
#18717=CARTESIAN_POINT('Ctrl Pts',(2.07786355472798,-0.00083496590290807,
-9.5893449541571));
#18718=CARTESIAN_POINT('Ctrl Pts',(2.07943303720893,0.298178416615211,-9.60555662723894));
#18719=CARTESIAN_POINT('Ctrl Pts',(2.31370169398425,1.08514940936176,-9.64810157893662));
#18720=CARTESIAN_POINT('Ctrl Pts',(3.5966891679774,1.72601943169721,-9.71697980925019));
#18721=CARTESIAN_POINT('Ctrl Pts',(5.01634665164319,0.895213050221392,-9.79597964509776));
#18722=CARTESIAN_POINT('Ctrl Pts',(5.09621241255259,-0.747750182775267,
-9.8749794809453));
#18723=CARTESIAN_POINT('Ctrl Pts',(3.76383778077046,-1.71232472144846,-9.95397931679288));
#18724=CARTESIAN_POINT('Ctrl Pts',(2.37463262236157,-1.17974343592703,-10.0254344745302));
#18725=CARTESIAN_POINT('Ctrl Pts',(2.07964814994376,-0.344625173506082,
-10.0705563536515));
#18726=CARTESIAN_POINT('Ctrl Pts',(2.07677307172911,0.00126791318965598,
-10.0893449541571));
#18727=CARTESIAN_POINT('Origin',(3.53951905042299,8.32667268468867E-16,
0.));
#18728=CARTESIAN_POINT('',(2.904562511392,-1.32104332876118,-10.4999647974346));
#18729=CARTESIAN_POINT('Ctrl Pts',(2.07677307172911,0.00126791318965598,
-10.0893449541571));
#18730=CARTESIAN_POINT('Ctrl Pts',(2.0756185663861,0.140163409899335,-10.0968896322674));
#18731=CARTESIAN_POINT('Ctrl Pts',(2.15728834009292,0.762509891316419,-10.1307675889936));
#18732=CARTESIAN_POINT('Ctrl Pts',(3.03967406104186,1.65296546888283,-10.1909788243355));
#18733=CARTESIAN_POINT('Ctrl Pts',(4.65091988412873,1.3220120331683,-10.2699786601832));
#18734=CARTESIAN_POINT('Ctrl Pts',(5.25379341461138,-0.208875272215984,
-10.3489784960306));
#18735=CARTESIAN_POINT('Ctrl Pts',(4.32983134761648,-1.5094750881873,-10.4256405417812));
#18736=CARTESIAN_POINT('Ctrl Pts',(3.3020958806422,-1.50905208505225,-10.4759693089158));
#18737=CARTESIAN_POINT('Ctrl Pts',(2.904562511392,-1.32104332876118,-10.4999647974346));
#18738=CARTESIAN_POINT('',(4.1735261449982,-1.31904027763685,-10.5));
#18739=CARTESIAN_POINT('Origin',(3.53951905042299,8.32667268468867E-16,
-10.5));
#18740=CARTESIAN_POINT('Ctrl Pts',(4.1735261449982,-1.31904027763685,-10.5));
#18741=CARTESIAN_POINT('Ctrl Pts',(4.61001469460598,-1.10923861968599,-10.4736667213841));
#18742=CARTESIAN_POINT('Ctrl Pts',(5.25113005292935,-0.226200379926371,
-10.4210001641525));
#18743=CARTESIAN_POINT('Ctrl Pts',(4.66306375306162,1.31298734088882,-10.3420003283048));
#18744=CARTESIAN_POINT('Ctrl Pts',(3.05428328236686,1.65687129011178,-10.2630004924574));
#18745=CARTESIAN_POINT('Ctrl Pts',(2.16068644613406,0.771444902797137,-10.20255206497));
#18746=CARTESIAN_POINT('Ctrl Pts',(2.07576260363487,0.14462423792681,-10.1684369160985));
#18747=CARTESIAN_POINT('Ctrl Pts',(2.07692213061801,0.00132420044191561,
-10.1606550458429));
#18748=CARTESIAN_POINT('Origin',(3.53951905042299,8.32667268468867E-16,
0.924367114736157));
#18749=CARTESIAN_POINT('',(4.21285985862019,0.966285267670136,-10.5));
#18750=CARTESIAN_POINT('Ctrl Pts',(4.21285985862019,0.966285267670136,-10.5));
#18751=CARTESIAN_POINT('Ctrl Pts',(4.12691296029429,1.02617602241623,-10.4924697639478));
#18752=CARTESIAN_POINT('Ctrl Pts',(4.03333366517216,1.07435164214843,-10.4846304956294));
#18753=CARTESIAN_POINT('Ctrl Pts',(3.8990102589921,1.12217937116524,-10.47446765702));
#18754=CARTESIAN_POINT('Ctrl Pts',(3.86285169382147,1.13312709505302,-10.4718237382524));
#18755=CARTESIAN_POINT('Ctrl Pts',(3.81653974099716,1.14475077295999,-10.4685493303852));
#18756=CARTESIAN_POINT('Ctrl Pts',(3.8068227682405,1.14705864197507,-10.4678683481899));
#18757=CARTESIAN_POINT('Ctrl Pts',(3.79111786242873,1.15057828923006,-10.4667771191176));
#18758=CARTESIAN_POINT('Ctrl Pts',(3.78514797849336,1.15186752446851,-10.466364484865));
#18759=CARTESIAN_POINT('Ctrl Pts',(3.77371953385572,1.15424268105789,-10.4655785992848));
#18760=CARTESIAN_POINT('Ctrl Pts',(3.76826279376341,1.1553364595976,-10.4652051148072));
#18761=CARTESIAN_POINT('Ctrl Pts',(3.7558197159075,1.15773900456352,-10.4643573277347));
#18762=CARTESIAN_POINT('Ctrl Pts',(3.74882882859123,1.15902329612631,-10.463883787959));
#18763=CARTESIAN_POINT('Ctrl Pts',(3.72680360950976,1.16286375339913,-10.4624002136484));
#18764=CARTESIAN_POINT('Ctrl Pts',(3.71173062999975,1.16519132362581,-10.461397137812));
#18765=CARTESIAN_POINT('Ctrl Pts',(3.61932276551113,1.17762851309365,-10.4553134950841));
#18766=CARTESIAN_POINT('Ctrl Pts',(3.54118478086041,1.18032900442303,-10.4504671690847));
#18767=CARTESIAN_POINT('Ctrl Pts',(3.43590521451579,1.17350560927382,-10.4439098990448));
#18768=CARTESIAN_POINT('Ctrl Pts',(3.40853530504769,1.17076660427417,-10.4422007519744));
#18769=CARTESIAN_POINT('Ctrl Pts',(3.35005555590813,1.16283789793965,-10.4384979914452));
#18770=CARTESIAN_POINT('Ctrl Pts',(3.31900877578698,1.15735186523851,-10.4365008725666));
#18771=CARTESIAN_POINT('Ctrl Pts',(3.27663502097098,1.1480974274304,-10.433687591134));
#18772=CARTESIAN_POINT('Ctrl Pts',(3.26508774453619,1.14539213879608,-10.4329118325623));
#18773=CARTESIAN_POINT('Ctrl Pts',(3.24513042288521,1.14039744528032,-10.4315521241759));
#18774=CARTESIAN_POINT('Ctrl Pts',(3.23670111984714,1.13818815997004,-10.4309719066595));
#18775=CARTESIAN_POINT('Ctrl Pts',(3.22452608118542,1.13485231746078,-10.4301242189358));
#18776=CARTESIAN_POINT('Ctrl Pts',(3.22075999106738,1.13380025318935,-10.4298606607323));
#18777=CARTESIAN_POINT('Ctrl Pts',(3.21697597771734,1.13272283871051,-10.429594429032));
#18778=CARTESIAN_POINT('Ctrl Pts',(3.21695268015998,1.132716204467,-10.4295927898323));
#18779=CARTESIAN_POINT('Ctrl Pts',(3.21690580728414,1.13270285532099,-10.4295894917808));
#18780=CARTESIAN_POINT('Ctrl Pts',(3.21688223196395,1.13269614039932,-10.4295878329275));
#18781=CARTESIAN_POINT('Ctrl Pts',(3.21683479462963,1.13268262729623,-10.4295844949363));
#18782=CARTESIAN_POINT('Ctrl Pts',(3.21681093261599,1.13267582909545,-10.429582815797));
#18783=CARTESIAN_POINT('Ctrl Pts',(3.21676291263406,1.13266214673687,-10.4295794365779));
#18784=CARTESIAN_POINT('Ctrl Pts',(3.21673875466121,1.13265526255739,-10.4295777364964));
#18785=CARTESIAN_POINT('Ctrl Pts',(3.21669013313684,1.13264140543728,-10.4295743147112));
#18786=CARTESIAN_POINT('Ctrl Pts',(3.21666566960863,1.132634432482,-10.4295725930078));
#18787=CARTESIAN_POINT('Ctrl Pts',(3.21661642702002,1.13262039490881,-10.4295691272736));
#18788=CARTESIAN_POINT('Ctrl Pts',(3.21659164794706,1.13261333026504,-10.4295673832405));
#18789=CARTESIAN_POINT('Ctrl Pts',(3.21654176391438,1.13259910629536,-10.4295638721137));
#18790=CARTESIAN_POINT('Ctrl Pts',(3.21651665897117,1.13259194695085,-10.4295621050194));
#18791=CARTESIAN_POINT('Ctrl Pts',(3.21646611244882,1.13257753044381,-10.4295585470087));
#18792=CARTESIAN_POINT('Ctrl Pts',(3.21644067087711,1.13257027325899,-10.429556756091));
#18793=CARTESIAN_POINT('Ctrl Pts',(3.21638943993205,1.13255565781255,-10.4295531496421));
#18794=CARTESIAN_POINT('Ctrl Pts',(3.21636365057277,1.13254829952938,-10.4295513341101));
#18795=CARTESIAN_POINT('Ctrl Pts',(3.21631171245287,1.1325334784993,-10.4295476776107));
#18796=CARTESIAN_POINT('Ctrl Pts',(3.21628556369563,1.13252601572658,-10.4295458366416));
#18797=CARTESIAN_POINT('Ctrl Pts',(3.21623289471368,1.13251098219282,-10.4295421284127));
#18798=CARTESIAN_POINT('Ctrl Pts',(3.21620637449497,1.13250341140542,-10.4295402611513));
#18799=CARTESIAN_POINT('Ctrl Pts',(3.21615295003582,1.13248815817352,-10.429536499448));
#18800=CARTESIAN_POINT('Ctrl Pts',(3.21612604579817,1.13248047570039,-10.4295346050041));
#18801=CARTESIAN_POINT('Ctrl Pts',(3.21607184022346,1.13246499527372,-10.4295307880087));
#18802=CARTESIAN_POINT('Ctrl Pts',(3.21604453890365,1.13245719729423,-10.4295288654561));
#18803=CARTESIAN_POINT('Ctrl Pts',(3.21598952556157,1.13244148187604,-10.4295249912787));
#18804=CARTESIAN_POINT('Ctrl Pts',(3.21596181353872,1.13243356440476,-10.4295230396515));
#18805=CARTESIAN_POINT('Ctrl Pts',(3.2159059646182,1.13241760585583,-10.4295191063199));
#18806=CARTESIAN_POINT('Ctrl Pts',(3.21587782771689,1.1324095647431,-10.4295171246129));
#18807=CARTESIAN_POINT('Ctrl Pts',(3.21582111424197,1.13239335457936,-10.4295131300719));
#18808=CARTESIAN_POINT('Ctrl Pts',(3.21579253768988,1.13238518549874,-10.4295111172371));
#18809=CARTESIAN_POINT('Ctrl Pts',(3.21573492949764,1.13236871488414,-10.4295070593472));
#18810=CARTESIAN_POINT('Ctrl Pts',(3.2157058978657,1.13236041331489,-10.42950501429));
#18811=CARTESIAN_POINT('Ctrl Pts',(3.21564736342919,1.13234367300984,-10.4295008908144));
#18812=CARTESIAN_POINT('Ctrl Pts',(3.21561786063733,1.13233523423811,-10.4294988123941));
#18813=CARTESIAN_POINT('Ctrl Pts',(3.21555836708481,1.13231821460407,-10.4294946210004));
#18814=CARTESIAN_POINT('Ctrl Pts',(3.21552837633875,1.13230963370428,-10.4294925080251));
#18815=CARTESIAN_POINT('Ctrl Pts',(3.21546788933872,1.1322923246698,-10.429488246277));
#18816=CARTESIAN_POINT('Ctrl Pts',(3.21543739309562,1.13228359649434,-10.4294860975017));
#18817=CARTESIAN_POINT('Ctrl Pts',(3.21537587676924,1.1322659875289,-10.4294817628525));
#18818=CARTESIAN_POINT('Ctrl Pts',(3.21534485670016,1.13225710669674,-10.4294795769763));
#18819=CARTESIAN_POINT('Ctrl Pts',(3.21528227355241,1.13223918678984,-10.4294751667644));
#18820=CARTESIAN_POINT('Ctrl Pts',(3.21525071048926,1.13223014767076,-10.4294729424264));
#18821=CARTESIAN_POINT('Ctrl Pts',(3.21518702130536,1.13221190530096,-10.4294684538676));
#18822=CARTESIAN_POINT('Ctrl Pts',(3.21515489519293,1.13220270200114,-10.4294661896438));
#18823=CARTESIAN_POINT('Ctrl Pts',(3.2150900589162,1.13218412509967,-10.4294616198228));
#18824=CARTESIAN_POINT('Ctrl Pts',(3.21505734877094,1.13217475144912,-10.4294593142232));
#18825=CARTESIAN_POINT('Ctrl Pts',(3.2149913224468,1.13215582738234,-10.4294546600893));
#18826=CARTESIAN_POINT('Ctrl Pts',(3.21495800628006,1.13214627691214,-10.4294523115519));
#18827=CARTESIAN_POINT('Ctrl Pts',(3.21489074487493,1.13212699242798,-10.4294475699064));
#18828=CARTESIAN_POINT('Ctrl Pts',(3.21485679965562,1.13211725835873,-10.4294451767953));
#18829=CARTESIAN_POINT('Ctrl Pts',(3.21478825600129,1.13209759956896,-10.429440344287));
#18830=CARTESIAN_POINT('Ctrl Pts',(3.21475365756872,1.13208767478485,-10.4294379048856));
#18831=CARTESIAN_POINT('Ctrl Pts',(3.21468378213638,1.13206762709836,-10.4294329779954));
#18832=CARTESIAN_POINT('Ctrl Pts',(3.21464850516653,1.13205750413648,-10.429430490504));
#18833=CARTESIAN_POINT('Ctrl Pts',(3.21457724606094,1.13203705225551,-10.4294254655438));
#18834=CARTESIAN_POINT('Ctrl Pts',(3.2145412639418,1.13202672326902,-10.4294229280711));
#18835=CARTESIAN_POINT('Ctrl Pts',(3.21447950250827,1.13200899091429,-10.4294185724067));
#18836=CARTESIAN_POINT('Ctrl Pts',(3.21445372294447,1.13200158837816,-10.4294167542611));
#18837=CARTESIAN_POINT('Ctrl Pts',(3.21439966149649,1.13198606277194,-10.4294129413488));
#18838=CARTESIAN_POINT('Ctrl Pts',(3.21437137966856,1.13197793952392,-10.4294109465724));
#18839=CARTESIAN_POINT('Ctrl Pts',(3.21431203566975,1.13196089203638,-10.4294067607464));
#18840=CARTESIAN_POINT('Ctrl Pts',(3.21428097357151,1.13195196758098,-10.4294045696853));
#18841=CARTESIAN_POINT('Ctrl Pts',(3.21421575320059,1.1319332262017,-10.4293999689597));
#18842=CARTESIAN_POINT('Ctrl Pts',(3.21418159499902,1.1319234090085,-10.4293975592799));
#18843=CARTESIAN_POINT('Ctrl Pts',(3.21410982221765,1.13190277772899,-10.4293924958429));
#18844=CARTESIAN_POINT('Ctrl Pts',(3.21407220772992,1.13189196331316,-10.4293898420671));
#18845=CARTESIAN_POINT('Ctrl Pts',(3.21399310983144,1.13186921787157,-10.429384261254));
#18846=CARTESIAN_POINT('Ctrl Pts',(3.21395162654273,1.13185728644171,-10.4293813341944));
#18847=CARTESIAN_POINT('Ctrl Pts',(3.21386431640998,1.13183216909085,-10.4293751732267));
#18848=CARTESIAN_POINT('Ctrl Pts',(3.21381848970678,1.13181898266601,-10.4293719392903));
#18849=CARTESIAN_POINT('Ctrl Pts',(3.21372194394328,1.1317911957137,-10.4293651257208));
#18850=CARTESIAN_POINT('Ctrl Pts',(3.2136712250741,1.13177659456317,-10.4293615460533));
#18851=CARTESIAN_POINT('Ctrl Pts',(3.21356425701046,1.13174579238354,-10.4293539958449));
#18852=CARTESIAN_POINT('Ctrl Pts',(3.21350800804115,1.13172959056992,-10.4293500252599));
#18853=CARTESIAN_POINT('Ctrl Pts',(3.21338923377783,1.13169536953595,-10.4293416403688));
#18854=CARTESIAN_POINT('Ctrl Pts',(3.21332670877271,1.13167734932834,-10.4293372260073));
#18855=CARTESIAN_POINT('Ctrl Pts',(3.21319450451768,1.13163923513577,-10.4293278913432));
#18856=CARTESIAN_POINT('Ctrl Pts',(3.21312482563956,1.13161913989954,-10.4293229709707));
#18857=CARTESIAN_POINT('Ctrl Pts',(3.21297778778636,1.13157671979344,-10.4293125868531));
#18858=CARTESIAN_POINT('Ctrl Pts',(3.21290042924635,1.13155439342679,-10.4293071230237));
#18859=CARTESIAN_POINT('Ctrl Pts',(3.21268346681041,1.13149175202437,-10.429291797269));
#18860=CARTESIAN_POINT('Ctrl Pts',(3.21254386815168,1.1314514191043,-10.4292819343375));
#18861=CARTESIAN_POINT('Ctrl Pts',(3.20946721188047,1.13056189295936,-10.4290645184194));
#18862=CARTESIAN_POINT('Ctrl Pts',(3.20653357160968,1.12970132343361,-10.4288563207278));
#18863=CARTESIAN_POINT('Ctrl Pts',(3.19957106784925,1.12762942957046,-10.4283600901626));
#18864=CARTESIAN_POINT('Ctrl Pts',(3.19554535715557,1.12640794487554,-10.4280714987364));
#18865=CARTESIAN_POINT('Ctrl Pts',(3.18253528599118,1.12238417060919,-10.4271336143682));
#18866=CARTESIAN_POINT('Ctrl Pts',(3.17357821558417,1.11949583571058,-10.4264798085899));
#18867=CARTESIAN_POINT('Ctrl Pts',(3.09149691085084,1.09193726525416,-10.4204195290882));
#18868=CARTESIAN_POINT('Ctrl Pts',(3.02093453246352,1.06024479488837,-10.4147173204694));
#18869=CARTESIAN_POINT('Ctrl Pts',(2.88642961043058,0.983174122961987,-10.403369426687));
#18870=CARTESIAN_POINT('Ctrl Pts',(2.8228683152307,0.93785552016733,-10.3977556629365));
#18871=CARTESIAN_POINT('Ctrl Pts',(2.75434645728467,0.877936049323524,-10.3914726025992));
#18872=CARTESIAN_POINT('Ctrl Pts',(2.7446004613044,0.86912149234229,-10.3905723030498));
#18873=CARTESIAN_POINT('Ctrl Pts',(2.73009293144841,0.855552238370565,-10.389221445348));
#18874=CARTESIAN_POINT('Ctrl Pts',(2.72522153716476,0.850917056936007,-10.3887659629644));
#18875=CARTESIAN_POINT('Ctrl Pts',(2.71647260729152,0.842448419557565,-10.3879443656035));
#18876=CARTESIAN_POINT('Ctrl Pts',(2.71258151907054,0.83862930315528,-10.3875776567349));
#18877=CARTESIAN_POINT('Ctrl Pts',(2.70426746309748,0.830354898431243,-10.3867912024319));
#18878=CARTESIAN_POINT('Ctrl Pts',(2.69985329798885,0.825890972362758,-10.3863718461832));
#18879=CARTESIAN_POINT('Ctrl Pts',(2.68800218394732,0.813713030465413,-10.3852408418027));
#18880=CARTESIAN_POINT('Ctrl Pts',(2.68063435032583,0.805932350826788,-10.3845321458456));
#18881=CARTESIAN_POINT('Ctrl Pts',(2.64243016607699,0.76446840655799,-10.3808255239602));
#18882=CARTESIAN_POINT('Ctrl Pts',(2.61346400703542,0.729111240885981,-10.3779057225038));
#18883=CARTESIAN_POINT('Ctrl Pts',(2.53978414887236,0.627675753345193,-10.3700228969018));
#18884=CARTESIAN_POINT('Ctrl Pts',(2.49961464066712,0.558609729728254,-10.3651888901604));
#18885=CARTESIAN_POINT('Ctrl Pts',(2.45017983010922,0.449492132932587,-10.3576570484934));
#18886=CARTESIAN_POINT('Ctrl Pts',(2.4355098468213,0.412148085575772,-10.355093007927));
#18887=CARTESIAN_POINT('Ctrl Pts',(2.42066117638748,0.367826539462877,-10.3519864476286));
#18888=CARTESIAN_POINT('Ctrl Pts',(2.41860172422818,0.361501933869866,-10.3515416665765));
#18889=CARTESIAN_POINT('Ctrl Pts',(2.41551103640892,0.351729998438064,-10.3508516866609));
#18890=CARTESIAN_POINT('Ctrl Pts',(2.41444180320891,0.34829469462588,-10.3506086022224));
#18891=CARTESIAN_POINT('Ctrl Pts',(2.41249932019603,0.341951471292379,-10.3501586951136));
#18892=CARTESIAN_POINT('Ctrl Pts',(2.41162155800402,0.339045022177699,-10.3499521345814));
#18893=CARTESIAN_POINT('Ctrl Pts',(2.40964757276049,0.332416250311918,-10.3494800816322));
#18894=CARTESIAN_POINT('Ctrl Pts',(2.40855851318749,0.328691925112741,-10.349214193736));
#18895=CARTESIAN_POINT('Ctrl Pts',(2.40575315599553,0.318919249303073,-10.3485148743054));
#18896=CARTESIAN_POINT('Ctrl Pts',(2.40406687890954,0.312862514262297,-10.3480798356185));
#18897=CARTESIAN_POINT('Ctrl Pts',(2.39162515800205,0.266748794412219,-10.3447567741295));
#18898=CARTESIAN_POINT('Ctrl Pts',(2.38294509815073,0.226166371157745,-10.3417712626954));
#18899=CARTESIAN_POINT('Ctrl Pts',(2.36526271536538,0.115126766491998,-10.333576132822));
#18900=CARTESIAN_POINT('Ctrl Pts',(2.36045907240003,0.0441668277872275,
-10.3283200339461));
#18901=CARTESIAN_POINT('Ctrl Pts',(2.36324626146657,-0.0783134036235878,
-10.3194747209279));
#18902=CARTESIAN_POINT('Ctrl Pts',(2.36779877002687,-0.129705798184287,
-10.3158297201827));
#18903=CARTESIAN_POINT('Ctrl Pts',(2.37734497666333,-0.191208906323424,
-10.311553974777));
#18904=CARTESIAN_POINT('Ctrl Pts',(2.37912909944433,-0.201753806456629,
-10.3108238314908));
#18905=CARTESIAN_POINT('Ctrl Pts',(2.38216761299106,-0.218336223749617,
-10.3096799713337));
#18906=CARTESIAN_POINT('Ctrl Pts',(2.38332617151421,-0.22439047573263,-10.3092632600904));
#18907=CARTESIAN_POINT('Ctrl Pts',(2.38558646377435,-0.235719495316486,
-10.3084851040733));
#18908=CARTESIAN_POINT('Ctrl Pts',(2.38667696508284,-0.240996313106781,
-10.3081233147359));
#18909=CARTESIAN_POINT('Ctrl Pts',(2.3892023845812,-0.252806997371728,-10.3073149382348));
#18910=CARTESIAN_POINT('Ctrl Pts',(2.39065684135969,-0.259336532989567,
-10.3068689834752));
#18911=CARTESIAN_POINT('Ctrl Pts',(2.39450494226832,-0.275943904992911,
-10.3057369432805));
#18912=CARTESIAN_POINT('Ctrl Pts',(2.39697607705039,-0.286003342217437,
-10.3050533305825));
#18913=CARTESIAN_POINT('Ctrl Pts',(2.41612685914796,-0.359748551490968,
-10.3000543016118));
#18914=CARTESIAN_POINT('Ctrl Pts',(2.43798835149292,-0.421972621601104,
-10.295914200806));
#18915=CARTESIAN_POINT('Ctrl Pts',(2.50133953419122,-0.563194112899108,
-10.2863123921748));
#18916=CARTESIAN_POINT('Ctrl Pts',(2.54680839404966,-0.63994180278262,-10.2809323599877));
#18917=CARTESIAN_POINT('Ctrl Pts',(2.60825253629757,-0.721113044748076,
-10.2742771728897));
#18918=CARTESIAN_POINT('Ctrl Pts',(2.61620325781039,-0.731265517311831,
-10.2734252352242));
#18919=CARTESIAN_POINT('Ctrl Pts',(2.62724940399224,-0.744903239726535,
-10.2722507364804));
#18920=CARTESIAN_POINT('Ctrl Pts',(2.63020153461821,-0.74850410685098,-10.2719377025984));
#18921=CARTESIAN_POINT('Ctrl Pts',(2.6351842922247,-0.754508853025449,-10.2714105875542));
#18922=CARTESIAN_POINT('Ctrl Pts',(2.63720338307405,-0.756922321241501,
-10.2711973265075));
#18923=CARTESIAN_POINT('Ctrl Pts',(2.64107454456425,-0.761512113330287,
-10.270789022964));
#18924=CARTESIAN_POINT('Ctrl Pts',(2.64292489092453,-0.763689820257783,
-10.2705941150436));
#18925=CARTESIAN_POINT('Ctrl Pts',(2.64734500091451,-0.768853724101917,
-10.2701291644115));
#18926=CARTESIAN_POINT('Ctrl Pts',(2.64992183856594,-0.771833779529966,
-10.2698586210713));
#18927=CARTESIAN_POINT('Ctrl Pts',(2.65911808138479,-0.78236179932678,-10.2688950874734));
#18928=CARTESIAN_POINT('Ctrl Pts',(2.66581876783266,-0.789837737037588,
-10.2681966373822));
#18929=CARTESIAN_POINT('Ctrl Pts',(2.71604221672672,-0.844450760888732,
-10.2629936637172));
#18930=CARTESIAN_POINT('Ctrl Pts',(2.76325243813557,-0.888042645332946,
-10.2582838914359));
#18931=CARTESIAN_POINT('Ctrl Pts',(2.86230090177843,-0.965540015174516,
-10.2490537663441));
#18932=CARTESIAN_POINT('Ctrl Pts',(2.91374024413245,-0.999647077829176,
-10.2445477290543));
#18933=CARTESIAN_POINT('Ctrl Pts',(2.99853794554455,-1.04675002924201,-10.2376490200572));
#18934=CARTESIAN_POINT('Ctrl Pts',(3.03021947955894,-1.06252556601585,-10.235175725431));
#18935=CARTESIAN_POINT('Ctrl Pts',(3.07142952627252,-1.08077806658095,-10.2320862223871));
#18936=CARTESIAN_POINT('Ctrl Pts',(3.08034118993985,-1.08459427159758,-10.2314254271313));
#18937=CARTESIAN_POINT('Ctrl Pts',(3.09482989261593,-1.09058811613258,-10.2303625889635));
#18938=CARTESIAN_POINT('Ctrl Pts',(3.10037804191978,-1.09283395950394,-10.2299582902402));
#18939=CARTESIAN_POINT('Ctrl Pts',(3.11104761559829,-1.09705853641024,-10.2291858406323));
#18940=CARTESIAN_POINT('Ctrl Pts',(3.11616621260847,-1.0990439387123,-10.2288174774336));
#18941=CARTESIAN_POINT('Ctrl Pts',(3.12789786117898,-1.10350029159658,-10.2279781377109));
#18942=CARTESIAN_POINT('Ctrl Pts',(3.13451966402631,-1.10594773729313,-10.2275079426231));
#18943=CARTESIAN_POINT('Ctrl Pts',(3.15558235257554,-1.11351804882051,-10.2260232491265));
#18944=CARTESIAN_POINT('Ctrl Pts',(3.17010177858657,-1.118418860395,-10.2250159613216));
#18945=CARTESIAN_POINT('Ctrl Pts',(3.26358518269553,-1.14795351306181,-10.2186245553719));
#18946=CARTESIAN_POINT('Ctrl Pts',(3.34486469702706,-1.16449494768915,-10.2135142232708));
#18947=CARTESIAN_POINT('Ctrl Pts',(3.45198811315878,-1.17475646615739,-10.2068518494481));
#18948=CARTESIAN_POINT('Ctrl Pts',(3.4768301435026,-1.17634368906135,-10.2053100587526));
#18949=CARTESIAN_POINT('Ctrl Pts',(3.54582105443965,-1.1785600256522,-10.2009971443494));
#18950=CARTESIAN_POINT('Ctrl Pts',(3.58997887832675,-1.17749581089715,-10.1982018206856));
#18951=CARTESIAN_POINT('Ctrl Pts',(3.64349202072682,-1.17319051698836,-10.1946631559371));
#18952=CARTESIAN_POINT('Ctrl Pts',(3.65300657211122,-1.17230837916763,-10.19402811157));
#18953=CARTESIAN_POINT('Ctrl Pts',(3.66665642796826,-1.17087511753538,-10.1931072544528));
#18954=CARTESIAN_POINT('Ctrl Pts',(3.67080147375498,-1.17041760822355,-10.1928263162972));
#18955=CARTESIAN_POINT('Ctrl Pts',(3.67800869530667,-1.16958334437505,-10.1923354305104));
#18956=CARTESIAN_POINT('Ctrl Pts',(3.68107196558551,-1.16921655529465,-10.1921260317118));
#18957=CARTESIAN_POINT('Ctrl Pts',(3.68755939112151,-1.16841389678158,-10.1916809044332));
#18958=CARTESIAN_POINT('Ctrl Pts',(3.69098302676092,-1.16797501675569,-10.1914450236572));
#18959=CARTESIAN_POINT('Ctrl Pts',(3.70032082580992,-1.16673624651299,-10.1907991060319));
#18960=CARTESIAN_POINT('Ctrl Pts',(3.70623081811424,-1.16590645536315,-10.1903874871926));
#18961=CARTESIAN_POINT('Ctrl Pts',(3.73466520507534,-1.16169352071419,-10.188394344782));
#18962=CARTESIAN_POINT('Ctrl Pts',(3.75709300669732,-1.15770258127492,-10.1867837182827));
#18963=CARTESIAN_POINT('Ctrl Pts',(3.80078763369272,-1.14861285962786,-10.1835872535575));
#18964=CARTESIAN_POINT('Ctrl Pts',(3.8220571347356,-1.14356675299423,-10.1820036044542));
#18965=CARTESIAN_POINT('Ctrl Pts',(3.92442490187191,-1.11625021341218,-10.1742799219596));
#18966=CARTESIAN_POINT('Ctrl Pts',(4.00313175086993,-1.08592497142648,-10.1680515336758));
#18967=CARTESIAN_POINT('Ctrl Pts',(4.07801580972292,-1.04743320081398,-10.1620447146955));
#18968=CARTESIAN_POINT('Ctrl Pts',(4.07809254084581,-1.04739374895876,-10.1620385595981));
#18969=CARTESIAN_POINT('Ctrl Pts',(4.07816926754606,-1.0473542887167,-10.1620324047393));
#18970=CARTESIAN_POINT('',(2.85485462588355,0.95829519891841,-10.5));
#18971=CARTESIAN_POINT('Origin',(3.53951905042299,8.32667268468867E-16,
-10.5));
#18972=CARTESIAN_POINT('',(2.36176905131988,-4.59633220793995E-5,-10.4243671147817));
#18973=CARTESIAN_POINT('Ctrl Pts',(2.36176905131988,-4.59633220629141E-5,
-10.4243671147817));
#18974=CARTESIAN_POINT('Ctrl Pts',(2.36176719489522,0.0475224899499069,
-10.4276061092289));
#18975=CARTESIAN_POINT('Ctrl Pts',(2.36465152554336,0.0951870191939661,
-10.4308451036761));
#18976=CARTESIAN_POINT('Ctrl Pts',(2.37043099647105,0.14257694276026,-10.4340840981233));
#18977=CARTESIAN_POINT('Ctrl Pts',(2.3762006347751,0.189886241769647,-10.4373175820638));
#18978=CARTESIAN_POINT('Ctrl Pts',(2.38485558852686,0.236921338236482,-10.4405510660043));
#18979=CARTESIAN_POINT('Ctrl Pts',(2.39635290126212,0.283312932837025,-10.4437845499448));
#18980=CARTESIAN_POINT('Ctrl Pts',(2.40783503551282,0.329643282334564,-10.4470137651151));
#18981=CARTESIAN_POINT('Ctrl Pts',(2.42215196230261,0.375331301165948,-10.4502429802854));
#18982=CARTESIAN_POINT('Ctrl Pts',(2.43920948510574,0.420016574638867,-10.4534721954557));
#18983=CARTESIAN_POINT('Ctrl Pts',(2.45625098279648,0.464659867424579,-10.4566983768598));
#18984=CARTESIAN_POINT('Ctrl Pts',(2.47602778023458,0.508301788416858,-10.4599245582639));
#18985=CARTESIAN_POINT('Ctrl Pts',(2.4983962137101,0.550598130558847,-10.463150739668));
#18986=CARTESIAN_POINT('Ctrl Pts',(2.52075937488268,0.592884503333545,-10.466376160652));
#18987=CARTESIAN_POINT('Ctrl Pts',(2.54571272466943,0.633825450117072,-10.469601581636));
#18988=CARTESIAN_POINT('Ctrl Pts',(2.57306577657067,0.673099644896752,-10.47282700262));
#18989=CARTESIAN_POINT('Ctrl Pts',(2.60041300765289,0.712365481999164,-10.4760517372239));
#18990=CARTESIAN_POINT('Ctrl Pts',(2.63015861772617,0.749964838514729,-10.4792764718278));
#18991=CARTESIAN_POINT('Ctrl Pts',(2.66206929628169,0.785606129976958,-10.4825012064317));
#18992=CARTESIAN_POINT('Ctrl Pts',(2.69400664615116,0.821277210842526,-10.485728636306));
#18993=CARTESIAN_POINT('Ctrl Pts',(2.72811232122637,0.854986562867321,-10.4889560661803));
#18994=CARTESIAN_POINT('Ctrl Pts',(2.76411439808519,0.886477685919338,-10.4921834960547));
#18995=CARTESIAN_POINT('Ctrl Pts',(2.79317884324904,0.911900442019834,-10.4947889973698));
#18996=CARTESIAN_POINT('Ctrl Pts',(2.82347841660538,0.935878125041895,-10.4973944986849));
#18997=CARTESIAN_POINT('Ctrl Pts',(2.85485462588355,0.958295198918412,-10.5));
#18998=CARTESIAN_POINT('Ctrl Pts',(4.07816926754758,-1.04735428871592,-10.2615635160918));
#18999=CARTESIAN_POINT('Ctrl Pts',(4.07189768950143,-1.05057973679272,-10.2620425082136));
#19000=CARTESIAN_POINT('Ctrl Pts',(4.06559906735751,-1.05374785987524,-10.2625215003355));
#19001=CARTESIAN_POINT('Ctrl Pts',(4.0592745442172,-1.05685821621007,-10.2630004924573));
#19002=CARTESIAN_POINT('Ctrl Pts',(4.01581207835197,-1.0782327535518,-10.2662921522843));
#19003=CARTESIAN_POINT('Ctrl Pts',(3.97093229426151,-1.09696933473833,-10.2695838121113));
#19004=CARTESIAN_POINT('Ctrl Pts',(3.92498877417435,-1.11288281259576,-10.2728754719383));
#19005=CARTESIAN_POINT('Ctrl Pts',(3.88064510817398,-1.12824214826868,-10.2760525089541));
#19006=CARTESIAN_POINT('Ctrl Pts',(3.83531115241496,-1.14097157503757,-10.2792295459699));
#19007=CARTESIAN_POINT('Ctrl Pts',(3.7893282018029,-1.1509519757083,-10.2824065829858));
#19008=CARTESIAN_POINT('Ctrl Pts',(3.74338991283836,-1.16092268276149,-10.2855805342556));
#19009=CARTESIAN_POINT('Ctrl Pts',(3.69680441740098,-1.16814953187371,-10.2887544855254));
#19010=CARTESIAN_POINT('Ctrl Pts',(3.64992723619355,-1.17256347163591,-10.2919284367952));
#19011=CARTESIAN_POINT('Ctrl Pts',(3.60307513846398,-1.17697504954619,-10.2951006897176));
#19012=CARTESIAN_POINT('Ctrl Pts',(3.55593221637032,-1.17857664819459,-10.2982729426401));
#19013=CARTESIAN_POINT('Ctrl Pts',(3.50886054014208,-1.17735089002699,-10.3014451955625));
#19014=CARTESIAN_POINT('Ctrl Pts',(3.46179352166238,-1.17612525314832,-10.3046171345901));
#19015=CARTESIAN_POINT('Ctrl Pts',(3.41479828999723,-1.17207283170602,-10.3077890736177));
#19016=CARTESIAN_POINT('Ctrl Pts',(3.36823563163836,-1.16522832653066,-10.3109610126454));
#19017=CARTESIAN_POINT('Ctrl Pts',(3.321625526321,-1.15837684686192,-10.3141361838522));
#19018=CARTESIAN_POINT('Ctrl Pts',(3.27544942398851,-1.14872768936456,-10.3173113550591));
#19019=CARTESIAN_POINT('Ctrl Pts',(3.2300597421721,-1.13636701775301,-10.320486526266));
#19020=CARTESIAN_POINT('Ctrl Pts',(3.18464214351442,-1.12399874373287,-10.3236636503562));
#19021=CARTESIAN_POINT('Ctrl Pts',(3.14001245434683,-1.10891581454595,-10.3268407744463));
#19022=CARTESIAN_POINT('Ctrl Pts',(3.09650622236022,-1.09125372699104,-10.3300178985365));
#19023=CARTESIAN_POINT('Ctrl Pts',(3.05292222210614,-1.07356006809826,-10.3332007018001));
#19024=CARTESIAN_POINT('Ctrl Pts',(3.01046618442413,-1.05327829596091,-10.3363835050637));
#19025=CARTESIAN_POINT('Ctrl Pts',(2.96945029737604,-1.0305904517797,-10.3395663083272));
#19026=CARTESIAN_POINT('Ctrl Pts',(2.95899478795995,-1.02480701064166,-10.3403776483198));
#19027=CARTESIAN_POINT('Ctrl Pts',(2.94863271329714,-1.01886743979341,-10.3411889883123));
#19028=CARTESIAN_POINT('Ctrl Pts',(2.93836892723928,-1.01277519316787,-10.3420003283049));
#19029=CARTESIAN_POINT('Ctrl Pts',(2.8967280706936,-0.988058547054513,-10.3452919881319));
#19030=CARTESIAN_POINT('Ctrl Pts',(2.85650517515445,-0.960704585188008,
-10.3485836479588));
#19031=CARTESIAN_POINT('Ctrl Pts',(2.81805680175141,-0.930906701147725,
-10.3518753077858));
#19032=CARTESIAN_POINT('Ctrl Pts',(2.78140908255892,-0.902504342603417,
-10.3550128091764));
#19033=CARTESIAN_POINT('Ctrl Pts',(2.74637389179197,-0.871882272761917,
-10.3581503105669));
#19034=CARTESIAN_POINT('Ctrl Pts',(2.71323359960642,-0.83925408326016,-10.3612878119575));
#19035=CARTESIAN_POINT('Ctrl Pts',(2.68012580534745,-0.806657889508507,
-10.3644222366615));
#19036=CARTESIAN_POINT('Ctrl Pts',(2.64890964063671,-0.772059864136999,
-10.3675566613655));
#19037=CARTESIAN_POINT('Ctrl Pts',(2.61983368595614,-0.735713186564894,
-10.3706910860696));
#19038=CARTESIAN_POINT('Ctrl Pts',(2.5907727637071,-0.699385300428803,-10.3738238902585));
#19039=CARTESIAN_POINT('Ctrl Pts',(2.56385021773247,-0.661310996241715,
-10.3769566944474));
#19040=CARTESIAN_POINT('Ctrl Pts',(2.53927510798554,-0.62177738630251,-10.3800894986363));
#19041=CARTESIAN_POINT('Ctrl Pts',(2.51470131136347,-0.582245888767549,
-10.3832221354297));
#19042=CARTESIAN_POINT('Ctrl Pts',(2.4924750007092,-0.541255726359354,-10.3863547722231));
#19043=CARTESIAN_POINT('Ctrl Pts',(2.47276095243106,-0.499121451020331,
-10.3894874090164));
#19044=CARTESIAN_POINT('Ctrl Pts',(2.45302344007767,-0.456937026579845,
-10.3926237743401));
#19045=CARTESIAN_POINT('Ctrl Pts',(2.43580439438563,-0.413606292013472,
-10.3957601396637));
#19046=CARTESIAN_POINT('Ctrl Pts',(2.42122088960644,-0.369464864384054,
-10.3988965049874));
#19047=CARTESIAN_POINT('Ctrl Pts',(2.40662720568347,-0.325292626469616,
-10.4020350594634));
#19048=CARTESIAN_POINT('Ctrl Pts',(2.39467286227741,-0.280309123097656,
-10.4051736139393));
#19049=CARTESIAN_POINT('Ctrl Pts',(2.38542429928129,-0.234862444607861,
-10.4083121684153));
#19050=CARTESIAN_POINT('Ctrl Pts',(2.37615682954507,-0.18932285995102,-10.4114571390052));
#19051=CARTESIAN_POINT('Ctrl Pts',(2.36960624399691,-0.14331877673319,-10.4146021095951));
#19052=CARTESIAN_POINT('Ctrl Pts',(2.36578718165589,-0.0972037177298007,
-10.417747080185));
#19053=CARTESIAN_POINT('Ctrl Pts',(2.36447039875689,-0.0813036051734252,
-10.4188314415075));
#19054=CARTESIAN_POINT('Ctrl Pts',(2.36347788782083,-0.0653902887482771,
-10.4199158028299));
#19055=CARTESIAN_POINT('Ctrl Pts',(2.36280881668566,-0.0494781600085864,
-10.4210001641524));
#19056=CARTESIAN_POINT('Ctrl Pts',(2.36211632627601,-0.0330090643176043,
-10.4221224810136));
#19057=CARTESIAN_POINT('Ctrl Pts',(2.36176969458343,-0.0165285106694148,
-10.4232447978749));
#19058=CARTESIAN_POINT('Ctrl Pts',(2.36176905131991,-4.59639904046127E-5,
-10.4243671147362));
#19059=CARTESIAN_POINT('Ctrl Pts',(3.03016972909157,-1.05969203810452,0.166133550473327));
#19060=CARTESIAN_POINT('Ctrl Pts',(2.67950307502106,-0.891141349940568,
0.139800271857472));
#19061=CARTESIAN_POINT('Ctrl Pts',(2.16444303486989,-0.1817253130263,0.0871337146257638));
#19062=CARTESIAN_POINT('Ctrl Pts',(2.63688451788926,1.05482934048912,0.00813387877820125));
#19063=CARTESIAN_POINT('Ctrl Pts',(3.92934827499653,1.33109899959936,-0.0708659570693613));
#19064=CARTESIAN_POINT('Ctrl Pts',(4.86756771448359,0.401458164283287,-0.149865792916923));
#19065=CARTESIAN_POINT('Ctrl Pts',(4.60127863509294,-0.893258821518505,
-0.228865628764486));
#19066=CARTESIAN_POINT('Ctrl Pts',(3.37159135201681,-1.37714798759902,-0.307865464612048));
#19067=CARTESIAN_POINT('Ctrl Pts',(2.29433432465055,-0.611917524973032,
-0.386865300459611));
#19068=CARTESIAN_POINT('Ctrl Pts',(2.34667400544937,0.708575406788336,-0.465865136307173));
#19069=CARTESIAN_POINT('Ctrl Pts',(3.48119555264166,1.38617687493562,-0.544864972154736));
#19070=CARTESIAN_POINT('Ctrl Pts',(4.66861629168543,0.806262653193108,-0.623864808002299));
#19071=CARTESIAN_POINT('Ctrl Pts',(4.83171763843987,-0.505117703190085,
-0.702864643849861));
#19072=CARTESIAN_POINT('Ctrl Pts',(3.82252286862625,-1.35824167832699,-0.781864479697424));
#19073=CARTESIAN_POINT('Ctrl Pts',(2.55658660705165,-0.979163204938215,
-0.860864315544985));
#19074=CARTESIAN_POINT('Ctrl Pts',(2.18237343206576,0.288222479142872,-0.93986415139255));
#19075=CARTESIAN_POINT('Ctrl Pts',(3.03937391325844,1.29412906681933,-1.01886398724011));
#19076=CARTESIAN_POINT('Ctrl Pts',(4.35010972888344,1.12599234088644,-1.09786382308768));
#19077=CARTESIAN_POINT('Ctrl Pts',(4.92547145397695,-0.0636538642554802,
-1.17686365893524));
#19078=CARTESIAN_POINT('Ctrl Pts',(4.24348620505496,-1.19555258043752,-1.2558634947828));
#19079=CARTESIAN_POINT('Ctrl Pts',(2.9228564643445,-1.24283671611121,-1.33486333063036));
#19080=CARTESIAN_POINT('Ctrl Pts',(2.16166784335581,-0.16260956886651,-1.41386316647793));
#19081=CARTESIAN_POINT('Ctrl Pts',(2.65047666571883,1.06513822635395,-1.49286300232549));
#19082=CARTESIAN_POINT('Ctrl Pts',(3.94583171405088,1.3265842755385,-1.57186283817305));
#19083=CARTESIAN_POINT('Ctrl Pts',(4.87257672678285,0.384542646461178,-1.65086267402061));
#19084=CARTESIAN_POINT('Ctrl Pts',(4.58996134785928,-0.90635908631751,-1.72986250986818));
#19085=CARTESIAN_POINT('Ctrl Pts',(3.35437647024072,-1.37500474221842,-1.80886234571574));
#19086=CARTESIAN_POINT('Ctrl Pts',(2.28675439453907,-0.596235299315049,
-1.8878621815633));
#19087=CARTESIAN_POINT('Ctrl Pts',(2.35565025061696,0.723443487680916,-1.96686201741086));
#19088=CARTESIAN_POINT('Ctrl Pts',(3.49856117658577,1.38680866306196,-2.04586185325842));
#19089=CARTESIAN_POINT('Ctrl Pts',(4.67862940733048,0.792050130990127,-2.12486168910599));
#19090=CARTESIAN_POINT('Ctrl Pts',(4.825287778842,-0.521262498390872,-2.20386152495355));
#19091=CARTESIAN_POINT('Ctrl Pts',(3.80548666508593,-1.36168169672898,-2.28286136080111));
#19092=CARTESIAN_POINT('Ctrl Pts',(2.5443976431265,-0.966772568896671,-2.36186119664867));
#19093=CARTESIAN_POINT('Ctrl Pts',(2.18609057479567,0.305200223776868,-2.44086103249624));
#19094=CARTESIAN_POINT('Ctrl Pts',(3.05562444562635,1.30029297725059,-2.5198608683438));
#19095=CARTESIAN_POINT('Ctrl Pts',(4.36415130109645,1.11574973286296,-2.59886070419136));
#19096=CARTESIAN_POINT('Ctrl Pts',(4.92456530437952,-0.0810104291810054,
-2.67786054003893));
#19097=CARTESIAN_POINT('Ctrl Pts',(4.22845447176036,-1.20427729384166,-2.75686037588648));
#19098=CARTESIAN_POINT('Ctrl Pts',(2.90733601591503,-1.23501434247363,-2.83586021173405));
#19099=CARTESIAN_POINT('Ctrl Pts',(2.15973897238825,-0.14533668323525,-2.91486004758161));
#19100=CARTESIAN_POINT('Ctrl Pts',(2.66388924862181,1.07619155610565,-2.99385988342918));
#19101=CARTESIAN_POINT('Ctrl Pts',(3.9624177558182,1.32139036632271,-3.07285971927674));
#19102=CARTESIAN_POINT('Ctrl Pts',(4.87728923720612,0.36781346167547,-3.1518595551243));
#19103=CARTESIAN_POINT('Ctrl Pts',(4.57852510200631,-0.919446703190933,
-3.23085939097186));
#19104=CARTESIAN_POINT('Ctrl Pts',(3.33716651933725,-1.37257760013728,-3.30985922681943));
#19105=CARTESIAN_POINT('Ctrl Pts',(2.27938374158492,-0.5804953218201,-3.38885906266698));
#19106=CARTESIAN_POINT('Ctrl Pts',(2.36480560961949,0.73821687005311,-3.46785889851455));
#19107=CARTESIAN_POINT('Ctrl Pts',(3.51593673409344,1.38721292150555,-3.54685873436211));
#19108=CARTESIAN_POINT('Ctrl Pts',(4.6884619210917,0.777718519243937,-3.62585857020968));
#19109=CARTESIAN_POINT('Ctrl Pts',(4.81865711520746,-0.537328229720796,
-3.70485840605724));
#19110=CARTESIAN_POINT('Ctrl Pts',(3.78840821414682,-1.36490658999665,-3.7838582419048));
#19111=CARTESIAN_POINT('Ctrl Pts',(2.53236510967047,-0.954230975635406,
-3.86285807775236));
#19112=CARTESIAN_POINT('Ctrl Pts',(2.19001996763953,0.322130471706748,-3.94185791359992));
#19113=CARTESIAN_POINT('Ctrl Pts',(3.07195098873404,1.30625262599693,-4.02085774944749));
#19114=CARTESIAN_POINT('Ctrl Pts',(4.37806342637599,1.10533214229617,-4.09985758529504));
#19115=CARTESIAN_POINT('Ctrl Pts',(4.92344182255072,-0.0983543391097721,
-4.17885742114262));
#19116=CARTESIAN_POINT('Ctrl Pts',(4.21331461435868,-1.21281299187304,-4.25785725699017));
#19117=CARTESIAN_POINT('Ctrl Pts',(2.89191478044192,-1.22699817633838,-4.33685709283774));
#19118=CARTESIAN_POINT('Ctrl Pts',(2.15802662474044,-0.128040981787732,
-4.41585692868529));
#19119=CARTESIAN_POINT('Ctrl Pts',(2.67743924402949,1.08707599671962,-4.49485676453287));
#19120=CARTESIAN_POINT('Ctrl Pts',(3.9789374320634,1.31598909612198,-4.57385660038042));
#19121=CARTESIAN_POINT('Ctrl Pts',(4.88179181429946,0.351026555392716,-4.65285643622799));
#19122=CARTESIAN_POINT('Ctrl Pts',(4.56692580665797,-0.93239003237817,-4.73185627207555));
#19123=CARTESIAN_POINT('Ctrl Pts',(3.31998832335595,-1.36993506236933,-4.81085610792312));
#19124=CARTESIAN_POINT('Ctrl Pts',(2.27221083923482,-0.564664248107207,
-4.88985594377067));
#19125=CARTESIAN_POINT('Ctrl Pts',(2.37414531422868,0.752874405345241,-4.96885577961824));
#19126=CARTESIAN_POINT('Ctrl Pts',(3.53331599231234,1.38739948728025,-5.0478556154658));
#19127=CARTESIAN_POINT('Ctrl Pts',(4.6981141334156,0.763264861565624,-5.12685545131336));
#19128=CARTESIAN_POINT('Ctrl Pts',(4.8118257188344,-0.553309639127398,-5.20585528716093));
#19129=CARTESIAN_POINT('Ctrl Pts',(3.77129070550129,-1.3679172910442,-5.28485512300849));
#19130=CARTESIAN_POINT('Ctrl Pts',(2.52049062698915,-0.941539636695861,
-5.36385495885605));
#19131=CARTESIAN_POINT('Ctrl Pts',(2.19416113484018,0.339010168304841,-5.44285479470361));
#19132=CARTESIAN_POINT('Ctrl Pts',(3.08835090641897,1.31200728697343,-5.52185463055117));
#19133=CARTESIAN_POINT('Ctrl Pts',(4.39184396046197,1.09474109403205,-5.60085446639874));
#19134=CARTESIAN_POINT('Ctrl Pts',(4.92210116432083,-0.115682814476576,
-5.6798543022463));
#19135=CARTESIAN_POINT('Ctrl Pts',(4.19806901948488,-1.22115836543997,-5.75885413809386));
#19136=CARTESIAN_POINT('Ctrl Pts',(2.87659517229037,-1.21878945968409,-5.83785397394143));
#19137=CARTESIAN_POINT('Ctrl Pts',(2.15653107210394,-0.110725187109488,
-5.91685380978898));
#19138=CARTESIAN_POINT('Ctrl Pts',(2.69112452400181,1.09778984453947,-5.99585364563655));
#19139=CARTESIAN_POINT('Ctrl Pts',(3.99538815120739,1.31038131022442,-6.07485348148411));
#19140=CARTESIAN_POINT('Ctrl Pts',(4.88608375104936,0.334184563172007,-6.15385331733167));
#19141=CARTESIAN_POINT('Ctrl Pts',(4.55516528229729,-0.945187043349074,
-6.23285315317924));
#19142=CARTESIAN_POINT('Ctrl Pts',(3.30284457791926,-1.36707754326538,-6.3118529890268));
#19143=CARTESIAN_POINT('Ctrl Pts',(2.26523681318173,-0.548744562694544,
-6.39085282487436));
#19144=CARTESIAN_POINT('Ctrl Pts',(2.38366789874921,0.76741379347118,-6.46985266072193));
#19145=CARTESIAN_POINT('Ctrl Pts',(3.55069622396548,1.38736833105958,-6.54885249656949));
#19146=CARTESIAN_POINT('Ctrl Pts',(4.70758452958949,0.748691426166348,-6.62785233241704));
#19147=CARTESIAN_POINT('Ctrl Pts',(4.80479466176584,-0.569204218691696,
-6.70685216826462));
#19148=CARTESIAN_POINT('Ctrl Pts',(3.7541368253653,-1.37071332740082,-6.78585200411217));
#19149=CARTESIAN_POINT('Ctrl Pts',(2.50877605852413,-0.928700543709767,
-6.86485183995974));
#19150=CARTESIAN_POINT('Ctrl Pts',(2.19851342653132,0.355836664674037,-6.9438516758073));
#19151=CARTESIAN_POINT('Ctrl Pts',(3.10482162507327,1.31755605711095,-7.02285151165486));
#19152=CARTESIAN_POINT('Ctrl Pts',(4.40549074080085,1.08397825010448,-7.10185134750243));
#19153=CARTESIAN_POINT('Ctrl Pts',(4.92054354007692,-0.132993135956621,
-7.18085118334998));
#19154=CARTESIAN_POINT('Ctrl Pts',(4.1827200796015,-1.22931210491848,-7.25985101919756));
#19155=CARTESIAN_POINT('Ctrl Pts',(2.86137959553775,-1.21038948068935,-7.3388508550451));
#19156=CARTESIAN_POINT('Ctrl Pts',(2.15525254917303,-0.0933920165355914,
-7.41785069089267));
#19157=CARTESIAN_POINT('Ctrl Pts',(2.70494294093347,1.10833141826107,-7.49685052674024));
#19158=CARTESIAN_POINT('Ctrl Pts',(4.01176733166974,1.30456788864948,-7.5758503625878));
#19159=CARTESIAN_POINT('Ctrl Pts',(4.89016437393018,0.31729012799526,-7.65485019843536));
#19160=CARTESIAN_POINT('Ctrl Pts',(4.5432453744814,-0.957835727892178,-7.73385003428293));
#19161=CARTESIAN_POINT('Ctrl Pts',(3.28573797336276,-1.36400549125164,-7.81284987013048));
#19162=CARTESIAN_POINT('Ctrl Pts',(2.25846275784679,-0.532738763826387,
-7.89184970597805));
#19163=CARTESIAN_POINT('Ctrl Pts',(2.39337186881909,0.781832752788139,-7.97084954182562));
#19164=CARTESIAN_POINT('Ctrl Pts',(3.56807470160707,1.38711945774027,-8.04984937767317));
#19165=CARTESIAN_POINT('Ctrl Pts',(4.71687162343945,0.734000500013747,-8.12884921352074));
#19166=CARTESIAN_POINT('Ctrl Pts',(4.79756504737693,-0.585009474080196,
-8.2078490493683));
#19167=CARTESIAN_POINT('Ctrl Pts',(3.73694926565633,-1.37329426034113,-8.28684888521586));
#19168=CARTESIAN_POINT('Ctrl Pts',(2.49722324263719,-0.915715711394235,
-8.36584872106343));
#19169=CARTESIAN_POINT('Ctrl Pts',(2.20307615968452,0.372607320078181,-8.44484855691098));
#19170=CARTESIAN_POINT('Ctrl Pts',(3.12136056003786,1.32289806600452,-8.52384839275855));
#19171=CARTESIAN_POINT('Ctrl Pts',(4.4190016257151,1.07304529883463,-8.60284822860612));
#19172=CARTESIAN_POINT('Ctrl Pts',(4.91876919447073,-0.150282585796148,
-8.68184806445366));
#19173=CARTESIAN_POINT('Ctrl Pts',(4.16727020297665,-1.23727293318732,-8.76084790030125));
#19174=CARTESIAN_POINT('Ctrl Pts',(2.84627043871991,-1.2017995529258,-8.83984773614879));
#19175=CARTESIAN_POINT('Ctrl Pts',(2.15419125509278,-0.0760441989173671,
-8.91884757199636));
#19176=CARTESIAN_POINT('Ctrl Pts',(2.71889232916227,1.11869908033215,-8.99784740784393));
#19177=CARTESIAN_POINT('Ctrl Pts',(4.02807239770252,1.29854971189147,-9.07684724369149));
#19178=CARTESIAN_POINT('Ctrl Pts',(4.89403305283643,0.300345961546974,-9.15584707953904));
#19179=CARTESIAN_POINT('Ctrl Pts',(4.53116793426698,-0.970334216088902,
-9.23484691538663));
#19180=CARTESIAN_POINT('Ctrl Pts',(3.2686712313047,-1.36071916966539,-9.31384675123416));
#19181=CARTESIAN_POINT('Ctrl Pts',(2.25188966568679,-0.516649779321854,
-9.39284658708175));
#19182=CARTESIAN_POINT('Ctrl Pts',(2.4032558358579,0.796129811879359,-9.4718464229293));
#19183=CARTESIAN_POINT('Ctrl Pts',(3.58544844273731,1.38665140132039,-9.55084625877686));
#19184=CARTESIAN_POINT('Ctrl Pts',(4.72597444318006,0.719197251069897,-9.62984609462442));
#19185=CARTESIAN_POINT('Ctrl Pts',(4.79013708657144,-0.600728369415522,
-9.70884593047199));
#19186=CARTESIAN_POINT('Ctrl Pts',(3.71973248027576,-1.37564932984407,-9.78784576631954));
#19187=CARTESIAN_POINT('Ctrl Pts',(2.48583065115498,-0.902606872160507,
-9.86684560216712));
#19188=CARTESIAN_POINT('Ctrl Pts',(2.20785497294659,0.389356961444151,-9.94584543801465));
#19189=CARTESIAN_POINT('Ctrl Pts',(3.13795302964717,1.32796122782191,-10.0248452738622));
#19190=CARTESIAN_POINT('Ctrl Pts',(4.43239748225584,1.06207949035224,-10.1038451097098));
#19191=CARTESIAN_POINT('Ctrl Pts',(4.91673468640922,-0.167806447366913,
-10.1828449455574));
#19192=CARTESIAN_POINT('Ctrl Pts',(4.15180495687604,-1.24454704202974,-10.2618447814049));
#19193=CARTESIAN_POINT('Ctrl Pts',(2.83111201811591,-1.1939738328192,-10.3408446172525));
#19194=CARTESIAN_POINT('Ctrl Pts',(2.15359519437813,-0.0566474417221517,
-10.4198505843376));
#19195=CARTESIAN_POINT('Ctrl Pts',(2.53953407659744,0.730669948020605,-10.4725232728068));
#19196=CARTESIAN_POINT('Ctrl Pts',(2.85623945459991,0.956824401315803,-10.4988626826603));
#19197=CARTESIAN_POINT('Ctrl Pts',(2.98834871728712,-1.14669989573515,0.110397971418231));
#19198=CARTESIAN_POINT('Ctrl Pts',(2.60888996776239,-0.964310060203871,
0.0840646928023764));
#19199=CARTESIAN_POINT('Ctrl Pts',(2.05154002730692,-0.196646185879096,
0.0313981355706681));
#19200=CARTESIAN_POINT('Ctrl Pts',(2.56277213988209,1.14143793787563,-0.0476017002768946));
#19201=CARTESIAN_POINT('Ctrl Pts',(3.961355881407,1.44039119778986,-0.126601536124457));
#19202=CARTESIAN_POINT('Ctrl Pts',(4.97660945957003,0.434420585011763,-0.205601371972019));
#19203=CARTESIAN_POINT('Ctrl Pts',(4.68845625222988,-0.966601390468067,
-0.284601207819581));
#19204=CARTESIAN_POINT('Ctrl Pts',(3.35780335630695,-1.49022111803005,-0.363601043667145));
#19205=CARTESIAN_POINT('Ctrl Pts',(2.19209626732059,-0.662160077507238,
-0.442600879514707));
#19206=CARTESIAN_POINT('Ctrl Pts',(2.24873338863196,0.766754222800465,-0.521600715362269));
#19207=CARTESIAN_POINT('Ctrl Pts',(3.47640680042968,1.49999133786299,-0.600600551209832));
#19208=CARTESIAN_POINT('Ctrl Pts',(4.76132278421946,0.872462250452896,-0.679600387057394));
#19209=CARTESIAN_POINT('Ctrl Pts',(4.9378158506882,-0.546591270628113,-0.758600222904958));
#19210=CARTESIAN_POINT('Ctrl Pts',(3.8457593892735,-1.4697624733565,-0.837600058752518));
#19211=CARTESIAN_POINT('Ctrl Pts',(2.47588122943425,-1.05955910267923,-0.916599894600083));
#19212=CARTESIAN_POINT('Ctrl Pts',(2.07094263094616,0.31188748702201,-0.995599730447643));
#19213=CARTESIAN_POINT('Ctrl Pts',(2.99830862700141,1.4003857843869,-1.0745995662952));
#19214=CARTESIAN_POINT('Ctrl Pts',(4.41666468618437,1.21844390017556,-1.15359940214277));
#19215=CARTESIAN_POINT('Ctrl Pts',(5.03926748629117,-0.0688802754764985,
-1.23259923799033));
#19216=CARTESIAN_POINT('Ctrl Pts',(4.30128665250989,-1.29371550416271,-1.31159907383789));
#19217=CARTESIAN_POINT('Ctrl Pts',(2.87222431031641,-1.34488198602467,-1.39059890968545));
#19218=CARTESIAN_POINT('Ctrl Pts',(2.04853697386742,-0.175960910302112,
-1.46959874553302));
#19219=CARTESIAN_POINT('Ctrl Pts',(2.57748029464644,1.15259325274191,-1.54859858138058));
#19220=CARTESIAN_POINT('Ctrl Pts',(3.97919272189017,1.43550578445872,-1.62759841722814));
#19221=CARTESIAN_POINT('Ctrl Pts',(4.98202974553497,0.416116189182186,-1.70659825307571));
#19222=CARTESIAN_POINT('Ctrl Pts',(4.67620973944672,-0.980777275290219,
-1.78559808892326));
#19223=CARTESIAN_POINT('Ctrl Pts',(3.33917501672534,-1.4879018977603,-1.86459792477083));
#19224=CARTESIAN_POINT('Ctrl Pts',(2.18389397386554,-0.645190235439661,
-1.94359776061839));
#19225=CARTESIAN_POINT('Ctrl Pts',(2.25844664401903,0.782843073330851,-2.02259759646596));
#19226=CARTESIAN_POINT('Ctrl Pts',(3.49519825912716,1.50067500005214,-2.10159743231351));
#19227=CARTESIAN_POINT('Ctrl Pts',(4.7721580441377,0.857082784398361,-2.18059726816108));
#19228=CARTESIAN_POINT('Ctrl Pts',(4.9308580562863,-0.564061662315234,-2.25959710400864));
#19229=CARTESIAN_POINT('Ctrl Pts',(3.82732439861496,-1.47348494045169,-2.3385969398562));
#19230=CARTESIAN_POINT('Ctrl Pts',(2.46269146942899,-1.04615111191774,-2.41759677570377));
#19231=CARTESIAN_POINT('Ctrl Pts',(2.07496497614415,0.330259218904082,-2.49659661155133));
#19232=CARTESIAN_POINT('Ctrl Pts',(3.01589343758964,1.40705579340337,-2.5755964473989));
#19233=CARTESIAN_POINT('Ctrl Pts',(4.43185916610274,1.20736030500805,-2.65459628324645));
#19234=CARTESIAN_POINT('Ctrl Pts',(5.03828693570521,-0.0876619313489172,
-2.73359611909402));
#19235=CARTESIAN_POINT('Ctrl Pts',(4.28502071261241,-1.30315657533346,-2.81259595494158));
#19236=CARTESIAN_POINT('Ctrl Pts',(2.85542952847803,-1.3364173427962,-2.89159579078914));
#19237=CARTESIAN_POINT('Ctrl Pts',(2.04644972959469,-0.157269804357935,
-2.9705956266367));
#19238=CARTESIAN_POINT('Ctrl Pts',(2.59199414099363,1.16455413535502,-3.04959546248426));
#19239=CARTESIAN_POINT('Ctrl Pts',(3.99714058946054,1.42988542029437,-3.12859529833183));
#19240=CARTESIAN_POINT('Ctrl Pts',(4.98712918482176,0.398013425587001,-3.20759513417939));
#19241=CARTESIAN_POINT('Ctrl Pts',(4.66383450073996,-0.994939473706866,
-3.28659497002696));
#19242=CARTESIAN_POINT('Ctrl Pts',(3.32055201287423,-1.4852754709577,-3.36559480587451));
#19243=CARTESIAN_POINT('Ctrl Pts',(2.17591814063276,-0.628157899720108,
-3.44459464172208));
#19244=CARTESIAN_POINT('Ctrl Pts',(2.26835371969396,0.798829449954148,-3.52359447756964));
#19245=CARTESIAN_POINT('Ctrl Pts',(3.51400046700072,1.50111245083826,-3.6025943134172));
#19246=CARTESIAN_POINT('Ctrl Pts',(4.78279787354038,0.841574450746565,-3.68159414926477));
#19247=CARTESIAN_POINT('Ctrl Pts',(4.92368297048308,-0.581446498454876,
-3.76059398511233));
#19248=CARTESIAN_POINT('Ctrl Pts',(3.80884369176145,-1.47697461918932,-3.83959382095989));
#19249=CARTESIAN_POINT('Ctrl Pts',(2.44967098388855,-1.03257976933148,-3.91859365680745));
#19250=CARTESIAN_POINT('Ctrl Pts',(2.0792169986208,0.348579554282547,-3.99759349265502));
#19251=CARTESIAN_POINT('Ctrl Pts',(3.03356049991161,1.41350476947407,-4.07659332850258));
#19252=CARTESIAN_POINT('Ctrl Pts',(4.44691357062203,1.19608736005122,-4.15559316435014));
#19253=CARTESIAN_POINT('Ctrl Pts',(5.03707120844708,-0.106429893164062,
-4.2345930001977));
#19254=CARTESIAN_POINT('Ctrl Pts',(4.26863777089002,-1.3123931116956,-4.31359283604526));
#19255=CARTESIAN_POINT('Ctrl Pts',(2.83874210564833,-1.32774299540001,-4.39259267189283));
#19256=CARTESIAN_POINT('Ctrl Pts',(2.04459678666542,-0.13855400926523,-4.47159250774039));
#19257=CARTESIAN_POINT('Ctrl Pts',(2.60665668233817,1.17633226189402,-4.55059234358796));
#19258=CARTESIAN_POINT('Ctrl Pts',(4.01501664245213,1.42404066941082,-4.62959217943551));
#19259=CARTESIAN_POINT('Ctrl Pts',(4.9920014538375,0.379848201170875,-4.70859201528308));
#19260=CARTESIAN_POINT('Ctrl Pts',(4.65128282507545,-1.00894553744593,-4.78759185113064));
#19261=CARTESIAN_POINT('Ctrl Pts',(3.30196337123839,-1.48241596303085,-4.8665916869782));
#19262=CARTESIAN_POINT('Ctrl Pts',(2.16815629466128,-0.611026988169218,
-4.94559152282576));
#19263=CARTESIAN_POINT('Ctrl Pts',(2.27846027699217,0.814690467671415,-5.02459135867333));
#19264=CARTESIAN_POINT('Ctrl Pts',(3.53280667943882,1.50131433492034,-5.1035911945209));
#19265=CARTESIAN_POINT('Ctrl Pts',(4.79324259754267,0.825934050369154,-5.18259103036845));
#19266=CARTESIAN_POINT('Ctrl Pts',(4.91629067043077,-0.598740089273046,
-5.26159086621601));
#19267=CARTESIAN_POINT('Ctrl Pts',(3.79032072030063,-1.48023251908209,-5.34059070206358));
#19268=CARTESIAN_POINT('Ctrl Pts',(2.43682152615653,-1.01884638593762,-5.41959053791113));
#19269=CARTESIAN_POINT('Ctrl Pts',(2.08369818355609,0.366845187724217,-5.49859037375871));
#19270=CARTESIAN_POINT('Ctrl Pts',(3.05130696135811,1.41973192689762,-5.57759020960626));
#19271=CARTESIAN_POINT('Ctrl Pts',(4.46182557942397,1.18462671535117,-5.65659004545384));
#19272=CARTESIAN_POINT('Ctrl Pts',(5.03562047314177,-0.125181153135692,
-5.73558988130139));
#19273=CARTESIAN_POINT('Ctrl Pts',(4.25214040993648,-1.32142369667214,-5.81458971714896));
#19274=CARTESIAN_POINT('Ctrl Pts',(2.82216465442814,-1.31886028778958,-5.89358955299651));
#19275=CARTESIAN_POINT('Ctrl Pts',(2.0429784390789,-0.119816471152147,-5.97258938884408));
#19276=CARTESIAN_POINT('Ctrl Pts',(2.6214656160218,1.18792578882087,-6.05158922469164));
#19277=CARTESIAN_POINT('Ctrl Pts',(4.03281807649984,1.41797244649999,-6.1305890605392));
#19278=CARTESIAN_POINT('Ctrl Pts',(4.99664578751808,0.361623367890064,-6.20958889638677));
#19279=CARTESIAN_POINT('Ctrl Pts',(4.63855668241017,-1.02279326925705,-6.28858873223433));
#19280=CARTESIAN_POINT('Ctrl Pts',(3.28341200876903,-1.47932382235155,-6.36758856808189));
#19281=CARTESIAN_POINT('Ctrl Pts',(2.16060965407101,-0.593800189300851,
-6.44658840392945));
#19282=CARTESIAN_POINT('Ctrl Pts',(2.28876472987488,0.830423637543947,-6.52558823977702));
#19283=CARTESIAN_POINT('Ctrl Pts',(3.55161394523668,1.50128062056398,-6.60458807562458));
#19284=CARTESIAN_POINT('Ctrl Pts',(4.80349057706377,0.810164037712699,-6.68358791147214));
#19285=CARTESIAN_POINT('Ctrl Pts',(4.90868231619433,-0.615939720933709,
-6.7625877473197));
#19286=CARTESIAN_POINT('Ctrl Pts',(3.77175839100488,-1.48325812886618,-6.84158758316727));
#19287=CARTESIAN_POINT('Ctrl Pts',(2.42414511267564,-1.00495311689426,-6.92058741901482));
#19288=CARTESIAN_POINT('Ctrl Pts',(2.08840782772533,0.385053252839684,-6.9995872548624));
#19289=CARTESIAN_POINT('Ctrl Pts',(3.06913003701067,1.42573628845678,-7.07858709070995));
#19290=CARTESIAN_POINT('Ctrl Pts',(4.47659285239482,1.17298016940594,-7.15758692655752));
#19291=CARTESIAN_POINT('Ctrl Pts',(5.03393495745053,-0.143912768664118,
-7.23658676240507));
#19292=CARTESIAN_POINT('Ctrl Pts',(4.23553121865162,-1.33024691311019,-7.31558659825265));
#19293=CARTESIAN_POINT('Ctrl Pts',(2.80569977628582,-1.3097706139116,-7.39458643410019));
#19294=CARTESIAN_POINT('Ctrl Pts',(2.04159494079934,-0.101060130465283,
-7.47358626994778));
#19295=CARTESIAN_POINT('Ctrl Pts',(2.63641861810635,1.19933289678506,-7.55258610579532));
#19296=CARTESIAN_POINT('Ctrl Pts',(4.05054209805801,1.4116817038369,-7.6315859416429));
#19297=CARTESIAN_POINT('Ctrl Pts',(5.0010614570369,0.343341785733108,-7.71058577749045));
#19298=CARTESIAN_POINT('Ctrl Pts',(4.6256580698339,-1.03648049604108,-7.78958561333802));
#19299=CARTESIAN_POINT('Ctrl Pts',(3.26490083669646,-1.47599953416481,-7.86858544918558));
#19300=CARTESIAN_POINT('Ctrl Pts',(2.15327940314247,-0.576480206481971,
-7.94758528503314));
#19301=CARTESIAN_POINT('Ctrl Pts',(2.2992654612829,0.846026490590706,-8.02658512088071));
#19302=CARTESIAN_POINT('Ctrl Pts',(3.57041931300681,1.50101131306799,-8.10558495672826));
#19303=CARTESIAN_POINT('Ctrl Pts',(4.81354020390489,0.794266887520294,-8.18458479257583));
#19304=CARTESIAN_POINT('Ctrl Pts',(4.90085910174346,-0.633042694301782,
-8.26358462842339));
#19305=CARTESIAN_POINT('Ctrl Pts',(3.75315961681622,-1.48605097379388,-8.34258446427096));
#19306=CARTESIAN_POINT('Ctrl Pts',(2.41164373274955,-0.990902142340378,
-8.4215843001185));
#19307=CARTESIAN_POINT('Ctrl Pts',(2.09334519201882,0.403200892070548,-8.5005841359661));
#19308=CARTESIAN_POINT('Ctrl Pts',(3.08702692999233,1.4315169122805,-8.57958397181362));
#19309=CARTESIAN_POINT('Ctrl Pts',(4.49121307201085,1.1611495491593,-8.65858380766123));
#19310=CARTESIAN_POINT('Ctrl Pts',(5.03201492611272,-0.162621798849685,
-8.73758364350875));
#19311=CARTESIAN_POINT('Ctrl Pts',(4.2188128030386,-1.3388613790282,-8.81658347935634));
#19312=CARTESIAN_POINT('Ctrl Pts',(2.7893500558721,-1.30047539519085,-8.89558331520388));
#19313=CARTESIAN_POINT('Ctrl Pts',(2.04044650732301,-0.0822879401130431,
-8.97458315105147));
#19314=CARTESIAN_POINT('Ctrl Pts',(2.65151334511416,1.21055181378021,-9.053582986899));
#19315=CARTESIAN_POINT('Ctrl Pts',(4.06818591989252,1.40516939421034,-9.13258282274659));
#19316=CARTESIAN_POINT('Ctrl Pts',(5.00524778055251,0.325006389032079,-9.21158265859414));
#19317=CARTESIAN_POINT('Ctrl Pts',(4.61258899038759,-1.05000519434651,-9.2905824944417));
#19318=CARTESIAN_POINT('Ctrl Pts',(3.24643280010204,-1.4724433834297,-9.36958233028927));
#19319=CARTESIAN_POINT('Ctrl Pts',(2.14616661581982,-0.559070207925378,
-9.44858216613683));
#19320=CARTESIAN_POINT('Ctrl Pts',(2.30996096862398,0.861497434581703,-9.52758200198439));
#19321=CARTESIAN_POINT('Ctrl Pts',(3.58921955536611,1.50050482606178,-9.60658183783196));
#19322=CARTESIAN_POINT('Ctrl Pts',(4.82339042649041,0.778248192078537,-9.68558167367951));
#19323=CARTESIAN_POINT('Ctrl Pts',(4.89282125529856,-0.650052216874333,
-9.76458150952707));
#19324=CARTESIAN_POINT('Ctrl Pts',(3.73452921733139,-1.48859941037392,-9.84358134537464));
#19325=CARTESIAN_POINT('Ctrl Pts',(2.39931573273156,-0.976716979064629,
-9.9225811812222));
#19326=CARTESIAN_POINT('Ctrl Pts',(2.0985163780543,0.421325791869091,-10.0015810170698));
#19327=CARTESIAN_POINT('Ctrl Pts',(3.10498175317381,1.43699579380393,-10.0805808529173));
#19328=CARTESIAN_POINT('Ctrl Pts',(4.50570881864875,1.14928337390154,-10.1595806887649));
#19329=CARTESIAN_POINT('Ctrl Pts',(5.02981337122874,-0.181584487549335,
-10.2385805246125));
#19330=CARTESIAN_POINT('Ctrl Pts',(4.20207775601229,-1.34673274122706,-10.31758036046));
#19331=CARTESIAN_POINT('Ctrl Pts',(2.77294702678338,-1.29200713072568,-10.3965801963076));
#19332=CARTESIAN_POINT('Ctrl Pts',(2.03980150600681,-0.0612985784366647,
-10.4755861633928));
#19333=CARTESIAN_POINT('Ctrl Pts',(2.45742857131213,0.790662874763801,-10.528258851862));
#19334=CARTESIAN_POINT('Ctrl Pts',(2.80013759513739,1.03538613273742,-10.5545982617154));
#19335=CARTESIAN_POINT('Ctrl Pts',(2.94652770548266,-1.23370775336577,0.0546623923631346));
#19336=CARTESIAN_POINT('Ctrl Pts',(2.53827686050373,-1.03747877046718,0.0283291137472804));
#19337=CARTESIAN_POINT('Ctrl Pts',(1.93863701974394,-0.211567058731892,
-0.0243374434844277));
#19338=CARTESIAN_POINT('Ctrl Pts',(2.48865976187493,1.22804653526214,-0.10333727933199));
#19339=CARTESIAN_POINT('Ctrl Pts',(3.99336348781746,1.54968339598036,-0.182337115179553));
#19340=CARTESIAN_POINT('Ctrl Pts',(5.08565120465648,0.467383005740241,-0.261336951027115));
#19341=CARTESIAN_POINT('Ctrl Pts',(4.7756338693668,-1.03994395941763,-0.340336786874677));
#19342=CARTESIAN_POINT('Ctrl Pts',(3.34401536059709,-1.60329424846109,-0.41933662272224));
#19343=CARTESIAN_POINT('Ctrl Pts',(2.08985820999061,-0.712402630041443,
-0.498336458569803));
#19344=CARTESIAN_POINT('Ctrl Pts',(2.15079277181453,0.824933038812594,-0.577336294417365));
#19345=CARTESIAN_POINT('Ctrl Pts',(3.47161804821771,1.61380580079035,-0.656336130264928));
#19346=CARTESIAN_POINT('Ctrl Pts',(4.85402927675347,0.938661847712682,-0.73533596611249));
#19347=CARTESIAN_POINT('Ctrl Pts',(5.04391406293652,-0.58806483806614,-0.814335801960053));
#19348=CARTESIAN_POINT('Ctrl Pts',(3.86899590992078,-1.58128326838601,-0.893335637807615));
#19349=CARTESIAN_POINT('Ctrl Pts',(2.39517585181685,-1.13995500042024,-0.972335473655178));
#19350=CARTESIAN_POINT('Ctrl Pts',(1.95951182982654,0.33555249490115,-1.05133530950274));
#19351=CARTESIAN_POINT('Ctrl Pts',(2.95724334074437,1.50664250195448,-1.1303351453503));
#19352=CARTESIAN_POINT('Ctrl Pts',(4.48321964348532,1.31089545946468,-1.20933498119787));
#19353=CARTESIAN_POINT('Ctrl Pts',(5.15306351860538,-0.0741066866975193,
-1.28833481704543));
#19354=CARTESIAN_POINT('Ctrl Pts',(4.35908709996481,-1.39187842788788,-1.36733465289299));
#19355=CARTESIAN_POINT('Ctrl Pts',(2.82159215628832,-1.44692725593814,-1.44633448874055));
#19356=CARTESIAN_POINT('Ctrl Pts',(1.93540610437903,-0.18931225173771,-1.52533432458812));
#19357=CARTESIAN_POINT('Ctrl Pts',(2.50448392357404,1.24004827912987,-1.60433416043568));
#19358=CARTESIAN_POINT('Ctrl Pts',(4.01255372972948,1.54442729337894,-1.68333399628324));
#19359=CARTESIAN_POINT('Ctrl Pts',(5.0914827642871,0.447689731903192,-1.76233383213081));
#19360=CARTESIAN_POINT('Ctrl Pts',(4.76245813103416,-1.05519546426293,-1.84133366797837));
#19361=CARTESIAN_POINT('Ctrl Pts',(3.32397356320997,-1.60079905330219,-1.92033350382593));
#19362=CARTESIAN_POINT('Ctrl Pts',(2.081033553192,-0.694145171564268,-1.99933333967349));
#19363=CARTESIAN_POINT('Ctrl Pts',(2.1612430374211,0.842242658980785,-2.07833317552106));
#19364=CARTESIAN_POINT('Ctrl Pts',(3.49183534166855,1.61454133704232,-2.15733301136862));
#19365=CARTESIAN_POINT('Ctrl Pts',(4.86568668094492,0.922115437806592,-2.23633284721618));
#19366=CARTESIAN_POINT('Ctrl Pts',(5.03642833373058,-0.606860826239594,
-2.31533268306374));
#19367=CARTESIAN_POINT('Ctrl Pts',(3.84916213214399,-1.58528818417442,-2.3943325189113));
#19368=CARTESIAN_POINT('Ctrl Pts',(2.38098529573147,-1.12552965493881,-2.47333235475887));
#19369=CARTESIAN_POINT('Ctrl Pts',(1.96383937749262,0.355318214031296,-2.55233219060643));
#19370=CARTESIAN_POINT('Ctrl Pts',(2.97616242955291,1.51381860955616,-2.63133202645399));
#19371=CARTESIAN_POINT('Ctrl Pts',(4.49956703110903,1.29897087715313,-2.71033186230156));
#19372=CARTESIAN_POINT('Ctrl Pts',(5.1520085670309,-0.0943134335168294,
-2.78933169814912));
#19373=CARTESIAN_POINT('Ctrl Pts',(4.34158695346446,-1.40203585682528,-2.86833153399668));
#19374=CARTESIAN_POINT('Ctrl Pts',(2.80352304104103,-1.43782034311876,-2.94733136984424));
#19375=CARTESIAN_POINT('Ctrl Pts',(1.93316048680112,-0.16920292548062,-3.0263312056918));
#19376=CARTESIAN_POINT('Ctrl Pts',(2.52009903336545,1.25291671460437,-3.10533104153937));
#19377=CARTESIAN_POINT('Ctrl Pts',(4.03186342310285,1.53838047426604,-3.18433087738693));
#19378=CARTESIAN_POINT('Ctrl Pts',(5.09696913243742,0.428213389498532,-3.2633307132345));
#19379=CARTESIAN_POINT('Ctrl Pts',(4.74914389947359,-1.0704322442228,-3.34233054908206));
#19380=CARTESIAN_POINT('Ctrl Pts',(3.30393750641121,-1.59797334177813,-3.42133038492961));
#19381=CARTESIAN_POINT('Ctrl Pts',(2.07245253968059,-0.675820477620115,
-3.50033022077719));
#19382=CARTESIAN_POINT('Ctrl Pts',(2.17190182976842,0.859442029855187,-3.57933005662473));
#19383=CARTESIAN_POINT('Ctrl Pts',(3.51206419990799,1.61501198017097,-3.65832989247232));
#19384=CARTESIAN_POINT('Ctrl Pts',(4.87713382598905,0.905430382249195,-3.73732972831986));
#19385=CARTESIAN_POINT('Ctrl Pts',(5.0287088257587,-0.625564767188955,-3.81632956416744));
#19386=CARTESIAN_POINT('Ctrl Pts',(3.82927916937608,-1.58904264838199,-3.89532940001498));
#19387=CARTESIAN_POINT('Ctrl Pts',(2.36697685810663,-1.11092856302756,-3.97432923586257));
#19388=CARTESIAN_POINT('Ctrl Pts',(1.96841402960207,0.375028636858347,-4.05332907171011));
#19389=CARTESIAN_POINT('Ctrl Pts',(2.99517001108918,1.52075691295122,-4.13232890755768));
#19390=CARTESIAN_POINT('Ctrl Pts',(4.51576371486808,1.28684257780627,-4.21132874340524));
#19391=CARTESIAN_POINT('Ctrl Pts',(5.15070059434344,-0.114505447218352,
-4.2903285792528));
#19392=CARTESIAN_POINT('Ctrl Pts',(4.32396092742136,-1.41197323151816,-4.36932841510037));
#19393=CARTESIAN_POINT('Ctrl Pts',(2.78556943085473,-1.42848781446165,-4.44832825094793));
#19394=CARTESIAN_POINT('Ctrl Pts',(1.93116694859041,-0.149067036742727,
-4.52732808679549));
#19395=CARTESIAN_POINT('Ctrl Pts',(2.53587412064685,1.26558852706842,-4.60632792264306));
#19396=CARTESIAN_POINT('Ctrl Pts',(4.05109585284088,1.53209224269965,-4.68532775849062));
#19397=CARTESIAN_POINT('Ctrl Pts',(5.10221109337554,0.408669846949035,-4.76432759433818));
#19398=CARTESIAN_POINT('Ctrl Pts',(4.73563984349293,-1.08550104251369,-4.84332743018574));
#19399=CARTESIAN_POINT('Ctrl Pts',(3.28393841912083,-1.59489686369236,-4.92232726603331));
#19400=CARTESIAN_POINT('Ctrl Pts',(2.06410175008772,-0.65738972823123,-5.00132710188086));
#19401=CARTESIAN_POINT('Ctrl Pts',(2.18277523975565,0.876506529997589,-5.08032693772843));
#19402=CARTESIAN_POINT('Ctrl Pts',(3.5322973665653,1.61522918256043,-5.15932677357599));
#19403=CARTESIAN_POINT('Ctrl Pts',(4.88837106166974,0.88860323917268,-5.23832660942356));
#19404=CARTESIAN_POINT('Ctrl Pts',(5.02075562202712,-0.644170539418693,
-5.31732644527111));
#19405=CARTESIAN_POINT('Ctrl Pts',(3.80935073509997,-1.59254774711999,-5.39632628111868));
#19406=CARTESIAN_POINT('Ctrl Pts',(2.35315242532392,-1.09615313517937,-5.47532611696624));
#19407=CARTESIAN_POINT('Ctrl Pts',(1.97323523227201,0.394680207143594,-5.55432595281381));
#19408=CARTESIAN_POINT('Ctrl Pts',(3.01426301629724,1.5274565668218,-5.63332578866137));
#19409=CARTESIAN_POINT('Ctrl Pts',(4.53180719838599,1.27451233667028,-5.71232562450893));
#19410=CARTESIAN_POINT('Ctrl Pts',(5.14913978196271,-0.134679491794805,
-5.79132546035649));
#19411=CARTESIAN_POINT('Ctrl Pts',(4.30621180038808,-1.42168902790432,-5.87032529620406));
#19412=CARTESIAN_POINT('Ctrl Pts',(2.76773413656592,-1.41893111589506,-5.94932513205162));
#19413=CARTESIAN_POINT('Ctrl Pts',(1.92942580605385,-0.128907755194804,
-6.02832496789918));
#19414=CARTESIAN_POINT('Ctrl Pts',(2.55180670804179,1.27806173310228,-6.10732480374674));
#19415=CARTESIAN_POINT('Ctrl Pts',(4.07024800179228,1.52556358277557,-6.1863246395943));
#19416=CARTESIAN_POINT('Ctrl Pts',(5.1072078239868,0.389062172608119,-6.26532447544188));
#19417=CARTESIAN_POINT('Ctrl Pts',(4.72194808252306,-1.10039949516504,-6.34432431128942));
#19418=CARTESIAN_POINT('Ctrl Pts',(3.26397943961881,-1.59157010143771,-6.42332414713699));
#19419=CARTESIAN_POINT('Ctrl Pts',(2.05598249496029,-0.638855815907156,
-6.50232398298456));
#19420=CARTESIAN_POINT('Ctrl Pts',(2.19386156100051,0.893433481616711,-6.58132381883211));
#19421=CARTESIAN_POINT('Ctrl Pts',(3.5525316665079,1.61519291006839,-6.66032365467969));
#19422=CARTESIAN_POINT('Ctrl Pts',(4.89939662453803,0.871636649259046,-6.73932349052724));
#19423=CARTESIAN_POINT('Ctrl Pts',(5.01256997062284,-0.66267522317572,-6.81832332637481));
#19424=CARTESIAN_POINT('Ctrl Pts',(3.78937995664444,-1.59580293033154,-6.89732316222237));
#19425=CARTESIAN_POINT('Ctrl Pts',(2.33951416682715,-1.08120569007876,-6.97632299806993));
#19426=CARTESIAN_POINT('Ctrl Pts',(1.97830222891934,0.414269841005327,-7.05532283391749));
#19427=CARTESIAN_POINT('Ctrl Pts',(3.03343844894807,1.53391651980261,-7.13432266976506));
#19428=CARTESIAN_POINT('Ctrl Pts',(4.54769496398879,1.26198208870742,-7.21332250561261));
#19429=CARTESIAN_POINT('Ctrl Pts',(5.14732637482417,-0.154832401371615,
-7.29232234146019));
#19430=CARTESIAN_POINT('Ctrl Pts',(4.28834235770175,-1.43118172130189,-7.37132217730774));
#19431=CARTESIAN_POINT('Ctrl Pts',(2.75001995703389,-1.40915174713386,-7.45032201315531));
#19432=CARTESIAN_POINT('Ctrl Pts',(1.92793733242564,-0.108728244394972,
-7.52932184900287));
#19433=CARTESIAN_POINT('Ctrl Pts',(2.56789429527925,1.29033437530905,-7.60832168485043));
#19434=CARTESIAN_POINT('Ctrl Pts',(4.08931686444629,1.51879551902432,-7.68732152069799));
#19435=CARTESIAN_POINT('Ctrl Pts',(5.1119585401436,0.369393443470953,-7.76632135654555));
#19436=CARTESIAN_POINT('Ctrl Pts',(4.70807076518642,-1.11512526418998,-7.84532119239312));
#19437=CARTESIAN_POINT('Ctrl Pts',(3.24406370003013,-1.58799357707798,-7.92432102824068));
#19438=CARTESIAN_POINT('Ctrl Pts',(2.04809604843815,-0.620221649137555,
-8.00332086408824));
#19439=CARTESIAN_POINT('Ctrl Pts',(2.20515905374669,0.910220228393272,-8.08232069993581));
#19440=CARTESIAN_POINT('Ctrl Pts',(3.57276392440657,1.61490316839571,-8.16132053578336));
#19441=CARTESIAN_POINT('Ctrl Pts',(4.9102087843703,0.854533275026842,-8.24032037163093));
#19442=CARTESIAN_POINT('Ctrl Pts',(5.00415315610998,-0.681075914523366,
-8.31932020747849));
#19443=CARTESIAN_POINT('Ctrl Pts',(3.76936996797612,-1.59880768724664,-8.39832004332606));
#19444=CARTESIAN_POINT('Ctrl Pts',(2.3260642228619,-1.06608857328652,-8.47731987917361));
#19445=CARTESIAN_POINT('Ctrl Pts',(1.98361422435313,0.433794464062913,-8.55631971502118));
#19446=CARTESIAN_POINT('Ctrl Pts',(3.05269329994679,1.54013575855648,-8.63531955086874));
#19447=CARTESIAN_POINT('Ctrl Pts',(4.56342451830662,1.24925379948397,-8.71431938671631));
#19448=CARTESIAN_POINT('Ctrl Pts',(5.1452606577547,-0.174961011903223,-8.79331922256386));
#19449=CARTESIAN_POINT('Ctrl Pts',(4.27035540310055,-1.44044982486908,-8.87231905841144));
#19450=CARTESIAN_POINT('Ctrl Pts',(2.73242967302428,-1.39915123745589,-8.95131889425898));
#19451=CARTESIAN_POINT('Ctrl Pts',(1.92670175955322,-0.0885316813087181,
-9.03031873010657));
#19452=CARTESIAN_POINT('Ctrl Pts',(2.58413436106606,1.30240454722827,-9.10931856595411));
#19453=CARTESIAN_POINT('Ctrl Pts',(4.1082994420825,1.51178907652922,-9.18831840180168));
#19454=CARTESIAN_POINT('Ctrl Pts',(5.11646250826858,0.349666816517182,-9.26731823764924));
#19455=CARTESIAN_POINT('Ctrl Pts',(4.6940100465082,-1.12967617260413,-9.34631807349681));
#19456=CARTESIAN_POINT('Ctrl Pts',(3.22419436889937,-1.58416759719399,-9.42531790934437));
#19457=CARTESIAN_POINT('Ctrl Pts',(2.04044356595287,-0.601490636528902,
-9.50431774519193));
#19458=CARTESIAN_POINT('Ctrl Pts',(2.21666610139006,0.926865057284047,-9.58331758103949));
#19459=CARTESIAN_POINT('Ctrl Pts',(3.59299066799492,1.61435825080319,-9.66231741688706));
#19460=CARTESIAN_POINT('Ctrl Pts',(4.92080640980075,0.837299133087174,-9.74131725273461));
#19461=CARTESIAN_POINT('Ctrl Pts',(4.99550542402567,-0.699376064333139,
-9.82031708858218));
#19462=CARTESIAN_POINT('Ctrl Pts',(3.749325954387,-1.60154949090376,-9.89931692442974));
#19463=CARTESIAN_POINT('Ctrl Pts',(2.31280081430815,-1.05082708596875,-9.97831676027731));
#19464=CARTESIAN_POINT('Ctrl Pts',(1.98917778316202,0.45329462229403,-10.0573165961249));
#19465=CARTESIAN_POINT('Ctrl Pts',(3.07201047670045,1.54603035978594,-10.1363164319724));
#19466=CARTESIAN_POINT('Ctrl Pts',(4.57902015504166,1.23648725745083,-10.21531626782));
#19467=CARTESIAN_POINT('Ctrl Pts',(5.14289205604824,-0.195362527731759,
-10.2943161036676));
#19468=CARTESIAN_POINT('Ctrl Pts',(4.25235055514854,-1.44891844042438,-10.3733159395151));
#19469=CARTESIAN_POINT('Ctrl Pts',(2.71478203545085,-1.39004042863217,-10.4523157753627));
#19470=CARTESIAN_POINT('Ctrl Pts',(1.92600781763548,-0.0659497151511775,
-10.5313217424478));
#19471=CARTESIAN_POINT('Ctrl Pts',(2.37532306602683,0.850655801506997,-10.5839944309171));
#19472=CARTESIAN_POINT('Ctrl Pts',(2.74403573567487,1.11394786415904,-10.6103338407705));
#19473=CARTESIAN_POINT('Ctrl Pts',(2.90470669367821,-1.32071561099641,-0.00107318669196121));
#19474=CARTESIAN_POINT('Ctrl Pts',(2.46766375324505,-1.11064748073047,-0.0274064653078154));
#19475=CARTESIAN_POINT('Ctrl Pts',(1.82573401218097,-0.226487931584689,
-0.0800730225395237));
#19476=CARTESIAN_POINT('Ctrl Pts',(2.41454738386776,1.31465513264865,-0.159072858387086));
#19477=CARTESIAN_POINT('Ctrl Pts',(4.02537109422792,1.65897559417085,-0.238072694234649));
#19478=CARTESIAN_POINT('Ctrl Pts',(5.19469294974294,0.500345426468717,-0.317072530082211));
#19479=CARTESIAN_POINT('Ctrl Pts',(4.86281148650372,-1.11328652836719,-0.396072365929774));
#19480=CARTESIAN_POINT('Ctrl Pts',(3.33022736488723,-1.71636737889213,-0.475072201777336));
#19481=CARTESIAN_POINT('Ctrl Pts',(1.98762015266065,-0.762645182575647,
-0.554072037624899));
#19482=CARTESIAN_POINT('Ctrl Pts',(2.05285215499711,0.883111854824721,-0.63307187347246));
#19483=CARTESIAN_POINT('Ctrl Pts',(3.46682929600573,1.72762026371771,-0.712071709320024));
#19484=CARTESIAN_POINT('Ctrl Pts',(4.94673576928749,1.00486144497247,-0.791071545167586));
#19485=CARTESIAN_POINT('Ctrl Pts',(5.15001227518484,-0.629538405504167,
-0.870071381015148));
#19486=CARTESIAN_POINT('Ctrl Pts',(3.89223243056803,-1.69280406341553,-0.949071216862711));
#19487=CARTESIAN_POINT('Ctrl Pts',(2.31447047419945,-1.22035089816125,-1.02807105271027));
#19488=CARTESIAN_POINT('Ctrl Pts',(1.84808102870693,0.35921750278029,-1.10707088855784));
#19489=CARTESIAN_POINT('Ctrl Pts',(2.91617805448732,1.61289921952204,-1.1860707244054));
#19490=CARTESIAN_POINT('Ctrl Pts',(4.54977460078626,1.4033470187538,-1.26507056025296));
#19491=CARTESIAN_POINT('Ctrl Pts',(5.26685955091959,-0.0793330979185393,
-1.34407039610052));
#19492=CARTESIAN_POINT('Ctrl Pts',(4.41688754741972,-1.49004135161307,-1.42307023194808));
#19493=CARTESIAN_POINT('Ctrl Pts',(2.77096000226024,-1.5489725258516,-1.50207006779565));
#19494=CARTESIAN_POINT('Ctrl Pts',(1.82227523489064,-0.202663593173311,
-1.58106990364321));
#19495=CARTESIAN_POINT('Ctrl Pts',(2.43148755250165,1.32750330551783,-1.66006973949077));
#19496=CARTESIAN_POINT('Ctrl Pts',(4.04591473756878,1.65334880229916,-1.73906957533833));
#19497=CARTESIAN_POINT('Ctrl Pts',(5.20093578303924,0.479263274624201,-1.8180694111859));
#19498=CARTESIAN_POINT('Ctrl Pts',(4.84870652262159,-1.12961365323564,-1.89706924703346));
#19499=CARTESIAN_POINT('Ctrl Pts',(3.3087721096946,-1.71369620884407,-1.97606908288102));
#19500=CARTESIAN_POINT('Ctrl Pts',(1.97817313251846,-0.743100107688879,
-2.05506891872859));
#19501=CARTESIAN_POINT('Ctrl Pts',(2.06403943082317,0.90164224463072,-2.13406875457615));
#19502=CARTESIAN_POINT('Ctrl Pts',(3.48847242420994,1.7284076740325,-2.21306859042371));
#19503=CARTESIAN_POINT('Ctrl Pts',(4.95921531775214,0.987148091214824,-2.29206842627127));
#19504=CARTESIAN_POINT('Ctrl Pts',(5.14199861117487,-0.649659990163954,
-2.37106826211884));
#19505=CARTESIAN_POINT('Ctrl Pts',(3.870999865673,-1.69709142789714,-2.4500680979664));
#19506=CARTESIAN_POINT('Ctrl Pts',(2.29927912203395,-1.20490819795988,-2.52906793381396));
#19507=CARTESIAN_POINT('Ctrl Pts',(1.85271377884109,0.38037720915851,-2.60806776966152));
#19508=CARTESIAN_POINT('Ctrl Pts',(2.93643142151619,1.62058142570894,-2.68706760550909));
#19509=CARTESIAN_POINT('Ctrl Pts',(4.56727489611532,1.39058144929823,-2.76606744135665));
#19510=CARTESIAN_POINT('Ctrl Pts',(5.26573019835659,-0.100964935684744,
-2.84506727720421));
#19511=CARTESIAN_POINT('Ctrl Pts',(4.39815319431651,-1.5009151383171,-2.92406711305178));
#19512=CARTESIAN_POINT('Ctrl Pts',(2.75161655360403,-1.53922334344132,-3.00306694889933));
#19513=CARTESIAN_POINT('Ctrl Pts',(1.81987124400756,-0.181136046603304,
-3.0820667847469));
#19514=CARTESIAN_POINT('Ctrl Pts',(2.44820392573725,1.34127929385372,-3.16106662059446));
#19515=CARTESIAN_POINT('Ctrl Pts',(4.06658625674519,1.6468755282377,-3.24006645644202));
#19516=CARTESIAN_POINT('Ctrl Pts',(5.20680908005306,0.458413353410064,-3.31906629228959));
#19517=CARTESIAN_POINT('Ctrl Pts',(4.83445329820725,-1.14592501473873,-3.39806612813715));
#19518=CARTESIAN_POINT('Ctrl Pts',(3.28732299994818,-1.71067121259855,-3.47706596398471));
#19519=CARTESIAN_POINT('Ctrl Pts',(1.96898693872843,-0.723483055520123,
-3.55606579983227));
#19520=CARTESIAN_POINT('Ctrl Pts',(2.07544993984288,0.920054609756227,-3.63506563567983));
#19521=CARTESIAN_POINT('Ctrl Pts',(3.51012793281527,1.72891150950368,-3.7140654715274));
#19522=CARTESIAN_POINT('Ctrl Pts',(4.97146977843772,0.969286313751825,-3.79306530737496));
#19523=CARTESIAN_POINT('Ctrl Pts',(5.1337346810343,-0.669683035923036,-3.87206514322252));
#19524=CARTESIAN_POINT('Ctrl Pts',(3.84971464699072,-1.70111067757465,-3.95106497907008));
#19525=CARTESIAN_POINT('Ctrl Pts',(2.2842827323247,-1.18927735672363,-4.03006481491765));
#19526=CARTESIAN_POINT('Ctrl Pts',(1.85761106058333,0.401477719434146,-4.10906465076521));
#19527=CARTESIAN_POINT('Ctrl Pts',(2.95677952226676,1.62800905642836,-4.18806448661277));
#19528=CARTESIAN_POINT('Ctrl Pts',(4.58461385911411,1.37759779556131,-4.26706432246033));
#19529=CARTESIAN_POINT('Ctrl Pts',(5.26432998023981,-0.122581001272642,
-4.3460641583079));
#19530=CARTESIAN_POINT('Ctrl Pts',(4.37928408395269,-1.51155335134072,-4.42506399415546));
#19531=CARTESIAN_POINT('Ctrl Pts',(2.73239675606114,-1.52923263352329,-4.50406383000302));
#19532=CARTESIAN_POINT('Ctrl Pts',(1.81773711051539,-0.159580064220224,
-4.58306366585058));
#19533=CARTESIAN_POINT('Ctrl Pts',(2.46509155895553,1.35484479224281,-4.66206350169815));
#19534=CARTESIAN_POINT('Ctrl Pts',(4.08717506322962,1.64014381598848,-4.74106333754571));
#19535=CARTESIAN_POINT('Ctrl Pts',(5.21242073291358,0.437491492727194,-4.82006317339327));
#19536=CARTESIAN_POINT('Ctrl Pts',(4.81999686191041,-1.16205654758144,-4.89906300924083));
#19537=CARTESIAN_POINT('Ctrl Pts',(3.26591346700327,-1.70737776435388,-4.9780628450884));
#19538=CARTESIAN_POINT('Ctrl Pts',(1.96004720551417,-0.70375246829324,-5.05706268093596));
#19539=CARTESIAN_POINT('Ctrl Pts',(2.08709020251914,0.938322592323762,-5.13606251678353));
#19540=CARTESIAN_POINT('Ctrl Pts',(3.53178805369179,1.72914403020051,-5.21506235263108));
#19541=CARTESIAN_POINT('Ctrl Pts',(4.9834995257968,0.95127242797621,-5.29406218847865));
#19542=CARTESIAN_POINT('Ctrl Pts',(5.1252205736235,-0.689600989564341,-5.37306202432621));
#19543=CARTESIAN_POINT('Ctrl Pts',(3.82838074989931,-1.70486297515788,-5.45206186017377));
#19544=CARTESIAN_POINT('Ctrl Pts',(2.2694833244913,-1.17345988442113,-5.53106169602134));
#19545=CARTESIAN_POINT('Ctrl Pts',(1.86277228098792,0.422515226562972,-5.6100615318689));
#19546=CARTESIAN_POINT('Ctrl Pts',(2.97721907123637,1.63518120674598,-5.68906136771646));
#19547=CARTESIAN_POINT('Ctrl Pts',(4.60178881734799,1.3643979579894,-5.76806120356402));
#19548=CARTESIAN_POINT('Ctrl Pts',(5.26265909078364,-0.144177830453919,
-5.84706103941159));
#19549=CARTESIAN_POINT('Ctrl Pts',(4.36028319083968,-1.5219543591365,-5.92606087525914));
#19550=CARTESIAN_POINT('Ctrl Pts',(2.71330361870369,-1.51900194400053,-6.00506071110672));
#19551=CARTESIAN_POINT('Ctrl Pts',(1.81587317302879,-0.137999039237464,
-6.08406054695427));
#19552=CARTESIAN_POINT('Ctrl Pts',(2.4821478000618,1.36819767738369,-6.16306038280184));
#19553=CARTESIAN_POINT('Ctrl Pts',(4.10767792708472,1.63315471905114,-6.24206021864939));
#19554=CARTESIAN_POINT('Ctrl Pts',(5.21776986045553,0.416500977326176,-6.32106005449696));
#19555=CARTESIAN_POINT('Ctrl Pts',(4.80533948263594,-1.17800572107301,-6.40005989034452));
#19556=CARTESIAN_POINT('Ctrl Pts',(3.24454687046858,-1.70381638052387,-6.47905972619209));
#19557=CARTESIAN_POINT('Ctrl Pts',(1.95135533584957,-0.683911442513464,
-6.55805956203965));
#19558=CARTESIAN_POINT('Ctrl Pts',(2.09895839212617,0.956443325689477,-6.63705939788721));
#19559=CARTESIAN_POINT('Ctrl Pts',(3.55344938777911,1.72910519957279,-6.71605923373477));
#19560=CARTESIAN_POINT('Ctrl Pts',(4.99530267201232,0.933109260805396,-6.79505906958234));
#19561=CARTESIAN_POINT('Ctrl Pts',(5.11645762505132,-0.709410725417731,
-6.87405890542989));
#19562=CARTESIAN_POINT('Ctrl Pts',(3.80700152228402,-1.70834773179691,-6.95305874127746));
#19563=CARTESIAN_POINT('Ctrl Pts',(2.25488322097866,-1.15745826326325,-7.03205857712502));
#19564=CARTESIAN_POINT('Ctrl Pts',(1.86819663011334,0.443486429170971,-7.11105841297258));
#19565=CARTESIAN_POINT('Ctrl Pts',(2.99774686088548,1.64209675114843,-7.19005824882015));
#19566=CARTESIAN_POINT('Ctrl Pts',(4.61879707558276,1.35098400800889,-7.26905808466771));
#19567=CARTESIAN_POINT('Ctrl Pts',(5.26071779219779,-0.165752034079112,
-7.34805792051527));
#19568=CARTESIAN_POINT('Ctrl Pts',(4.34115349675186,-1.53211652949359,-7.42705775636284));
#19569=CARTESIAN_POINT('Ctrl Pts',(2.69434013778197,-1.50853288035613,-7.5060575922104));
#19570=CARTESIAN_POINT('Ctrl Pts',(1.81427972405195,-0.116396358324663,
-7.58505742805796));
#19571=CARTESIAN_POINT('Ctrl Pts',(2.49936997245213,1.38133585383303,-7.66405726390553));
#19572=CARTESIAN_POINT('Ctrl Pts',(4.12809163083458,1.62590933421174,-7.74305709975308));
#19573=CARTESIAN_POINT('Ctrl Pts',(5.22285562325029,0.395445101208801,-7.82205693560065));
#19574=CARTESIAN_POINT('Ctrl Pts',(4.79048346053894,-1.19377003233889,-7.90105677144821));
#19575=CARTESIAN_POINT('Ctrl Pts',(3.22322656336381,-1.69998761999115,-7.98005660729577));
#19576=CARTESIAN_POINT('Ctrl Pts',(1.94291269373384,-0.66396309179314,-8.05905644314334));
#19577=CARTESIAN_POINT('Ctrl Pts',(2.11105264621048,0.974413966195839,-8.13805627899089));
#19578=CARTESIAN_POINT('Ctrl Pts',(3.57510853580632,1.72879502372344,-8.21705611483847));
#19579=CARTESIAN_POINT('Ctrl Pts',(5.00687736483572,0.914799662533391,-8.29605595068602));
#19580=CARTESIAN_POINT('Ctrl Pts',(5.10744721047652,-0.729109134744952,
-8.37505578653359));
#19581=CARTESIAN_POINT('Ctrl Pts',(3.785580319136,-1.7115644006994,-8.45405562238115));
#19582=CARTESIAN_POINT('Ctrl Pts',(2.24048471297425,-1.14127500423266,-8.53305545822871));
#19583=CARTESIAN_POINT('Ctrl Pts',(1.87388325668743,0.464388036055279,-8.61205529407627));
#19584=CARTESIAN_POINT('Ctrl Pts',(3.01835966990126,1.64875460483247,-8.69105512992383));
#19585=CARTESIAN_POINT('Ctrl Pts',(4.63563596460239,1.33735804980865,-8.77005496577141));
#19586=CARTESIAN_POINT('Ctrl Pts',(5.25850638939668,-0.187300224956761,
-8.84905480161895));
#19587=CARTESIAN_POINT('Ctrl Pts',(4.3218980031625,-1.54203827070995,-8.92805463746653));
#19588=CARTESIAN_POINT('Ctrl Pts',(2.67550929017646,-1.49782707972093,-9.00705447331408));
#19589=CARTESIAN_POINT('Ctrl Pts',(1.81295701178344,-0.0947754225043939,
-9.08605430916166));
#19590=CARTESIAN_POINT('Ctrl Pts',(2.51675537701794,1.39425728067634,-9.1650541450092));
#19591=CARTESIAN_POINT('Ctrl Pts',(4.14841296427251,1.6184087588481,-9.24405398085678));
#19592=CARTESIAN_POINT('Ctrl Pts',(5.22767723598463,0.374327244002286,-9.32305381670433));
#19593=CARTESIAN_POINT('Ctrl Pts',(4.77543110262881,-1.20934715086173,-9.4020536525519));
#19594=CARTESIAN_POINT('Ctrl Pts',(3.20195593769669,-1.69589181095829,-9.48105348839945));
#19595=CARTESIAN_POINT('Ctrl Pts',(1.93472051608591,-0.643911065132426,
-9.56005332424703));
#19596=CARTESIAN_POINT('Ctrl Pts',(2.12337123415615,0.992232679986391,-9.63905316009459));
#19597=CARTESIAN_POINT('Ctrl Pts',(3.59676178062372,1.72821167554459,-9.71805299594214));
#19598=CARTESIAN_POINT('Ctrl Pts',(5.0182223931111,0.896350074095812,-9.79705283178971));
#19599=CARTESIAN_POINT('Ctrl Pts',(5.09818959275277,-0.748699911791949,
-9.87605266763726));
#19600=CARTESIAN_POINT('Ctrl Pts',(3.76412269144261,-1.71449957143361,-9.95505250348484));
#19601=CARTESIAN_POINT('Ctrl Pts',(2.22628589588474,-1.12493719287287,-10.0340523393324));
#19602=CARTESIAN_POINT('Ctrl Pts',(1.87983918826973,0.48526345271897,-10.11305217518));
#19603=CARTESIAN_POINT('Ctrl Pts',(3.03903920022708,1.65506492576796,-10.1920520110275));
#19604=CARTESIAN_POINT('Ctrl Pts',(4.65233149143457,1.32369114100012,-10.2710518468751));
#19605=CARTESIAN_POINT('Ctrl Pts',(5.25597074086776,-0.209140567914182,
-10.3500516827227));
#19606=CARTESIAN_POINT('Ctrl Pts',(4.30262335428479,-1.5511041396217,-10.4290515185703));
#19607=CARTESIAN_POINT('Ctrl Pts',(2.65661704411831,-1.48807372653865,-10.5080513544178));
#19608=CARTESIAN_POINT('Ctrl Pts',(1.81221412926416,-0.0706008518656905,
-10.5870573215029));
#19609=CARTESIAN_POINT('Ctrl Pts',(2.29321756074153,0.910648728250192,-10.6397300099722));
#19610=CARTESIAN_POINT('Ctrl Pts',(2.68793387621235,1.19250959558065,-10.6660694198255));
#19611=CARTESIAN_POINT('Ctrl Pts',(2.90397937668593,-1.32076737590681,-10.5));
#19612=CARTESIAN_POINT('Ctrl Pts',(2.86727944188692,-1.29893471207351,-10.5));
#19613=CARTESIAN_POINT('Ctrl Pts',(2.83169802649736,-1.27545802809138,-10.5));
#19614=CARTESIAN_POINT('Ctrl Pts',(2.79735929175741,-1.25033824989213,-10.5));
#19615=CARTESIAN_POINT('Ctrl Pts',(2.75114791045458,-1.21653328714673,-10.5));
#19616=CARTESIAN_POINT('Ctrl Pts',(2.70718528420868,-1.17975351331922,-10.5));
#19617=CARTESIAN_POINT('Ctrl Pts',(2.66560257997516,-1.1403158632289,-10.5));
#19618=CARTESIAN_POINT('Ctrl Pts',(2.62355743994437,-1.10043963220698,-10.5));
#19619=CARTESIAN_POINT('Ctrl Pts',(2.58394493340546,-1.05784496331721,-10.5));
#19620=CARTESIAN_POINT('Ctrl Pts',(2.5469462583716,-1.01283383699425,-10.5));
#19621=CARTESIAN_POINT('Ctrl Pts',(2.5370259142128,-1.00076513821813,-10.5));
#19622=CARTESIAN_POINT('Ctrl Pts',(2.52729375930872,-0.988522626584723,
-10.5));
#19623=CARTESIAN_POINT('Ctrl Pts',(2.51775390963644,-0.976111975007932,
-10.5));
#19624=CARTESIAN_POINT('Ctrl Pts',(2.511245118406,-0.967644510328506,-10.5));
#19625=CARTESIAN_POINT('Ctrl Pts',(2.5048258504571,-0.959098775995798,-10.5));
#19626=CARTESIAN_POINT('Ctrl Pts',(2.49849748762295,-0.9504765680643,-10.5));
#19627=CARTESIAN_POINT('Ctrl Pts',(2.49201582400825,-0.941645492335477,
-10.5));
#19628=CARTESIAN_POINT('Ctrl Pts',(2.4856340766425,-0.932740308072392,-10.5));
#19629=CARTESIAN_POINT('Ctrl Pts',(2.47935728107968,-0.923769104127284,
-10.5));
#19630=CARTESIAN_POINT('Ctrl Pts',(2.4467581478561,-0.877176305356714,-10.5));
#19631=CARTESIAN_POINT('Ctrl Pts',(2.41695002133948,-0.82875554916227,-10.5));
#19632=CARTESIAN_POINT('Ctrl Pts',(2.39006706139692,-0.778810652111408,
-10.5));
#19633=CARTESIAN_POINT('Ctrl Pts',(2.36362934736646,-0.729692961636386,
-10.5));
#19634=CARTESIAN_POINT('Ctrl Pts',(2.34002048016728,-0.679100081706049,
-10.5));
#19635=CARTESIAN_POINT('Ctrl Pts',(2.31941557933448,-0.62730817924926,-10.5));
#19636=CARTESIAN_POINT('Ctrl Pts',(2.30117769346663,-0.581465939407855,
-10.5));
#19637=CARTESIAN_POINT('Ctrl Pts',(2.28529375648752,-0.534683695016422,
-10.5));
#19638=CARTESIAN_POINT('Ctrl Pts',(2.27191932854041,-0.487154532944957,
-10.5));
#19639=CARTESIAN_POINT('Ctrl Pts',(2.26791530106224,-0.472925283536962,
-10.5));
#19640=CARTESIAN_POINT('Ctrl Pts',(2.26413503174816,-0.458622787410054,
-10.5));
#19641=CARTESIAN_POINT('Ctrl Pts',(2.26059128056392,-0.444286805968637,
-10.5));
#19642=CARTESIAN_POINT('Ctrl Pts',(2.24768137294169,-0.392060736343278,
-10.5));
#19643=CARTESIAN_POINT('Ctrl Pts',(2.23788480709244,-0.339323391333285,
-10.5));
#19644=CARTESIAN_POINT('Ctrl Pts',(2.23134948683768,-0.286330333482162,
-10.5));
#19645=CARTESIAN_POINT('Ctrl Pts',(2.22490254378003,-0.234053901249509,
-10.5));
#19646=CARTESIAN_POINT('Ctrl Pts',(2.22162908761336,-0.18152772715788,-10.5));
#19647=CARTESIAN_POINT('Ctrl Pts',(2.22172052929498,-0.129002563547201,
-10.5));
#19648=CARTESIAN_POINT('Ctrl Pts',(2.22176330894542,-0.104429435641195,
-10.5));
#19649=CARTESIAN_POINT('Ctrl Pts',(2.2225432872073,-0.0798566892928238,
-10.5));
#19650=CARTESIAN_POINT('Ctrl Pts',(2.22408399749618,-0.0553112432975004,
-10.5));
#19651=CARTESIAN_POINT('Ctrl Pts',(2.22555857229785,-0.0318194185062761,
-10.5));
#19652=CARTESIAN_POINT('Ctrl Pts',(2.22773004647856,-0.00835259134640754,
-10.5));
#19653=CARTESIAN_POINT('Ctrl Pts',(2.23058759941273,0.0150644752044568,
-10.5));
#19654=CARTESIAN_POINT('Ctrl Pts',(2.23213148334798,0.0277162908283425,
-10.5));
#19655=CARTESIAN_POINT('Ctrl Pts',(2.23387629223041,0.0403574166494886,
-10.5));
#19656=CARTESIAN_POINT('Ctrl Pts',(2.23581806955776,0.0529688042131,-10.5));
#19657=CARTESIAN_POINT('Ctrl Pts',(2.23897614296403,0.0734797490674775,
-10.5));
#19658=CARTESIAN_POINT('Ctrl Pts',(2.24265154618475,0.0938916833615652,
-10.5));
#19659=CARTESIAN_POINT('Ctrl Pts',(2.24683171282339,0.114191366177429,-10.5));
#19660=CARTESIAN_POINT('Ctrl Pts',(2.25746540461127,0.16583059234145,-10.5));
#19661=CARTESIAN_POINT('Ctrl Pts',(2.27136188653188,0.216742631762888,-10.5));
#19662=CARTESIAN_POINT('Ctrl Pts',(2.28834566774239,0.266665394582686,-10.5));
#19663=CARTESIAN_POINT('Ctrl Pts',(2.30534672793287,0.316638947883617,-10.5));
#19664=CARTESIAN_POINT('Ctrl Pts',(2.3254421275876,0.365622165690229,-10.5));
#19665=CARTESIAN_POINT('Ctrl Pts',(2.34849751348331,0.41332218547471,-10.5));
#19666=CARTESIAN_POINT('Ctrl Pts',(2.35585489053263,0.42854409641569,-10.5));
#19667=CARTESIAN_POINT('Ctrl Pts',(2.36351397167454,0.443635044630669,-10.5));
#19668=CARTESIAN_POINT('Ctrl Pts',(2.37147109168874,0.458584629107004,-10.5));
#19669=CARTESIAN_POINT('Ctrl Pts',(2.37981195901927,0.47425518585883,-10.5));
#19670=CARTESIAN_POINT('Ctrl Pts',(2.3884803057648,0.489770423174206,-10.5));
#19671=CARTESIAN_POINT('Ctrl Pts',(2.39747223867455,0.505117767236418,-10.5));
#19672=CARTESIAN_POINT('Ctrl Pts',(2.40328124679998,0.515032526082609,-10.5));
#19673=CARTESIAN_POINT('Ctrl Pts',(2.409220878025,0.524869543178701,-10.5));
#19674=CARTESIAN_POINT('Ctrl Pts',(2.41528654831792,0.534621100868321,-10.5));
#19675=CARTESIAN_POINT('Ctrl Pts',(2.44252213382478,0.578406761884308,-10.5));
#19676=CARTESIAN_POINT('Ctrl Pts',(2.47231467151112,0.620504165307216,-10.5));
#19677=CARTESIAN_POINT('Ctrl Pts',(2.50453063857843,0.660637211715554,-10.5));
#19678=CARTESIAN_POINT('Ctrl Pts',(2.52964140926431,0.691918958533218,-10.5));
#19679=CARTESIAN_POINT('Ctrl Pts',(2.556225371933,0.722006721374281,-10.5));
#19680=CARTESIAN_POINT('Ctrl Pts',(2.58423075837921,0.750750430600732,-10.5));
#19681=CARTESIAN_POINT('Ctrl Pts',(2.59504794536868,0.761852797571121,-10.5));
#19682=CARTESIAN_POINT('Ctrl Pts',(2.60608091248154,0.772757625787352,-10.5));
#19683=CARTESIAN_POINT('Ctrl Pts',(2.61730509025834,0.783435451842213,-10.5));
#19684=CARTESIAN_POINT('Ctrl Pts',(2.65308565292733,0.817474348224813,-10.5));
#19685=CARTESIAN_POINT('Ctrl Pts',(2.69084286268129,0.849248709423217,-10.5));
#19686=CARTESIAN_POINT('Ctrl Pts',(2.73046767024449,0.878489839539784,-10.5));
#19687=CARTESIAN_POINT('Ctrl Pts',(2.7700924778077,0.907730969656352,-10.5));
#19688=CARTESIAN_POINT('Ctrl Pts',(2.8115855332062,0.934439564031336,-10.5));
#19689=CARTESIAN_POINT('Ctrl Pts',(2.85485462588355,0.95829519891841,-10.5));
#19690=CARTESIAN_POINT('',(2.85417850162344,0.958898071501409,0.000498685380349388));
#19691=CARTESIAN_POINT('Ctrl Pts',(2.85340124062148,0.959453028700747,1.346579098227E-16));
#19692=CARTESIAN_POINT('Ctrl Pts',(2.82282123135218,0.942844416454162,2.85745455358478E-16));
#19693=CARTESIAN_POINT('Ctrl Pts',(2.79311110010296,0.924851703347499,1.79905765899949E-15));
#19694=CARTESIAN_POINT('Ctrl Pts',(2.76437680446153,0.905503479527772,1.65145674912992E-15));
#19695=CARTESIAN_POINT('Ctrl Pts',(2.72398476848259,0.878305521992729,1.46763134221225E-15));
#19696=CARTESIAN_POINT('Ctrl Pts',(2.68551952020721,0.848431625036211,-6.61741344488266E-17));
#19697=CARTESIAN_POINT('Ctrl Pts',(2.64904553316328,0.816198607929121,-9.40220123979429E-16));
#19698=CARTESIAN_POINT('Ctrl Pts',(2.61505513991653,0.786160407672056,-1.75475040453543E-15));
#19699=CARTESIAN_POINT('Ctrl Pts',(2.58279383214052,0.75407239651815,1.19466269310647E-15));
#19700=CARTESIAN_POINT('Ctrl Pts',(2.55233048054817,0.720153874898648,1.35655375821386E-15));
#19701=CARTESIAN_POINT('Ctrl Pts',(2.53991532102457,0.706330581180162,1.44941899268915E-15));
#19702=CARTESIAN_POINT('Ctrl Pts',(2.52779900822753,0.692202886525742,6.75371079343568E-16));
#19703=CARTESIAN_POINT('Ctrl Pts',(2.51598720874143,0.677784246701662,5.55111512312578E-17));
#19704=CARTESIAN_POINT('Ctrl Pts',(2.50622350289069,0.665865710650002,-4.56868864520839E-16));
#19705=CARTESIAN_POINT('Ctrl Pts',(2.49666446159073,0.653743392170785,-9.49057168119929E-16));
#19706=CARTESIAN_POINT('Ctrl Pts',(2.48733805546213,0.641458137644336,-7.35522753814166E-16));
#19707=CARTESIAN_POINT('Ctrl Pts',(2.46849049126708,0.616631090639603,-3.03994947069626E-16));
#19708=CARTESIAN_POINT('Ctrl Pts',(2.45057636777883,0.591120920027303,-3.48031265324085E-16));
#19709=CARTESIAN_POINT('Ctrl Pts',(2.43360906387558,0.565001421693496,5.55111512312578E-17));
#19710=CARTESIAN_POINT('Ctrl Pts',(2.40527139199654,0.521378358321186,7.29481079207401E-16));
#19711=CARTESIAN_POINT('Ctrl Pts',(2.37957461447215,0.476059956151351,7.91024143821084E-16));
#19712=CARTESIAN_POINT('Ctrl Pts',(2.35661191998427,0.429363332514691,1.06165076729781E-15));
#19713=CARTESIAN_POINT('Ctrl Pts',(2.33337865186161,0.382116474009215,1.33546623384434E-15));
#19714=CARTESIAN_POINT('Ctrl Pts',(2.31294353384136,0.333457798512449,1.04920881821834E-15));
#19715=CARTESIAN_POINT('Ctrl Pts',(2.29544081289486,0.283679223188047,1.02001740387436E-15));
#19716=CARTESIAN_POINT('Ctrl Pts',(2.28937407302452,0.266425124894886,1.00989916466954E-15));
#19717=CARTESIAN_POINT('Ctrl Pts',(2.28366002281829,0.249036224651675,6.65784231122416E-16));
#19718=CARTESIAN_POINT('Ctrl Pts',(2.27830555103768,0.231523994364829,9.36750677027476E-16));
#19719=CARTESIAN_POINT('Ctrl Pts',(2.27541733157404,0.222077840488457,1.12794527297599E-15));
#19720=CARTESIAN_POINT('Ctrl Pts',(2.27263638189792,0.212604328404696,7.26586891309585E-16));
#19721=CARTESIAN_POINT('Ctrl Pts',(2.26996417256006,0.203108804611541,7.49400541621981E-16));
#19722=CARTESIAN_POINT('Ctrl Pts',(2.2552174363151,0.150707227047437,8.66263172620935E-16));
#19723=CARTESIAN_POINT('Ctrl Pts',(2.24376949101641,0.0976065262008687,
4.08534101287946E-17));
#19724=CARTESIAN_POINT('Ctrl Pts',(2.23572379087075,0.0441418535747884,
-4.30211422042248E-16));
#19725=CARTESIAN_POINT('Ctrl Pts',(2.22776565223313,-0.00874096199995714,
-8.96149646665323E-16));
#19726=CARTESIAN_POINT('Ctrl Pts',(2.22313553231218,-0.0619809771007474,
-2.8965713559225E-15));
#19727=CARTESIAN_POINT('Ctrl Pts',(2.22197643437771,-0.11527988813662,-3.05311331771918E-16));
#19728=CARTESIAN_POINT('Ctrl Pts',(2.22156081320029,-0.134391436437367,
6.84947814620585E-16));
#19729=CARTESIAN_POINT('Ctrl Pts',(2.22159192280362,-0.153510722380135,
-2.249679686016E-15));
#19730=CARTESIAN_POINT('Ctrl Pts',(2.22207794087312,-0.172624402843412,
-1.95676808090184E-15));
#19731=CARTESIAN_POINT('Ctrl Pts',(2.22254868025268,-0.19113721676339,-1.69646123182782E-15));
#19732=CARTESIAN_POINT('Ctrl Pts',(2.22344617954617,-0.209644777811353,
-7.8653483386481E-16));
#19733=CARTESIAN_POINT('Ctrl Pts',(2.22476297375739,-0.228137688022508,
-8.46545056276682E-16));
#19734=CARTESIAN_POINT('Ctrl Pts',(2.22566358113939,-0.240785717083357,
-9.08251614191495E-16));
#19735=CARTESIAN_POINT('Ctrl Pts',(2.22676034036135,-0.253426894133299,
1.47785297643783E-15));
#19736=CARTESIAN_POINT('Ctrl Pts',(2.22805107762706,-0.266058211650706,
1.2490009027033E-15));
#19737=CARTESIAN_POINT('Ctrl Pts',(2.229054816298,-0.275880924757348,1.05749732675775E-15));
#19738=CARTESIAN_POINT('Ctrl Pts',(2.23017537077975,-0.285692245157826,
-1.19694993143268E-15));
#19739=CARTESIAN_POINT('Ctrl Pts',(2.23141023118955,-0.295482958015865,
-1.11022302462516E-15));
#19740=CARTESIAN_POINT('Ctrl Pts',(2.23807405618757,-0.348317753409599,
-1.00747358571781E-15));
#19741=CARTESIAN_POINT('Ctrl Pts',(2.24806925032871,-0.400620352965406,
-1.83995180019013E-15));
#19742=CARTESIAN_POINT('Ctrl Pts',(2.26115510042849,-0.452165650093407,
-6.80011602582908E-16));
#19743=CARTESIAN_POINT('Ctrl Pts',(2.27469329060466,-0.505492719399986,
5.20024380441516E-16));
#19744=CARTESIAN_POINT('Ctrl Pts',(2.29153956097441,-0.558010093520958,
1.70050696717714E-15));
#19745=CARTESIAN_POINT('Ctrl Pts',(2.31148387864684,-0.609475073754277,
1.0547118733939E-15));
#19746=CARTESIAN_POINT('Ctrl Pts',(2.33139955447925,-0.660866145631631,
4.09844199643771E-16));
#19747=CARTESIAN_POINT('Ctrl Pts',(2.35440479749347,-0.711208818186421,
1.40927671219343E-15));
#19748=CARTESIAN_POINT('Ctrl Pts',(2.38034178509477,-0.760253836071474,
-1.37390099297363E-15));
#19749=CARTESIAN_POINT('Ctrl Pts',(2.38536182807648,-0.769746383995935,
-1.94096119465944E-15));
#19750=CARTESIAN_POINT('Ctrl Pts',(2.39049176520819,-0.779189910459008,
-1.05786827234693E-15));
#19751=CARTESIAN_POINT('Ctrl Pts',(2.39572358819186,-0.788570541648585,
-1.09634523681734E-15));
#19752=CARTESIAN_POINT('Ctrl Pts',(2.42367023236854,-0.838678728188221,
-1.88936709962824E-15));
#19753=CARTESIAN_POINT('Ctrl Pts',(2.45456608382348,-0.887081973696992,
3.65232473515907E-16));
#19754=CARTESIAN_POINT('Ctrl Pts',(2.48819247431748,-0.933519435542038,
2.77555756156289E-17));
#19755=CARTESIAN_POINT('Ctrl Pts',(2.51600207204131,-0.971924007494446,
-2.51343567462733E-16));
#19756=CARTESIAN_POINT('Ctrl Pts',(2.54568038471531,-1.00898433996931,-4.3693060571794E-16));
#19757=CARTESIAN_POINT('Ctrl Pts',(2.57712943690931,-1.04454500585365,2.4980018054066E-16));
#19758=CARTESIAN_POINT('Ctrl Pts',(2.58576841395081,-1.05431343303106,3.77772073805713E-16));
#19759=CARTESIAN_POINT('Ctrl Pts',(2.5945411341515,-1.06396863366007,-8.59691604797718E-16));
#19760=CARTESIAN_POINT('Ctrl Pts',(2.60344584338375,-1.07350722294854,1.66533453693773E-16));
#19761=CARTESIAN_POINT('Ctrl Pts',(2.61835241085208,-1.0894749116257,2.03691117354429E-15));
#19762=CARTESIAN_POINT('Ctrl Pts',(2.6336097141709,-1.10509519388837,4.91596122024362E-17));
#19763=CARTESIAN_POINT('Ctrl Pts',(2.64920051209182,-1.12034810033449,-6.66133814775094E-16));
#19764=CARTESIAN_POINT('Ctrl Pts',(2.69083818446211,-1.16108338049909,-2.5764371560264E-15));
#19765=CARTESIAN_POINT('Ctrl Pts',(2.73486472145526,-1.19921459067702,2.67919633695607E-16));
#19766=CARTESIAN_POINT('Ctrl Pts',(2.78109411133917,-1.23446584252596,-5.55111512312578E-17));
#19767=CARTESIAN_POINT('Ctrl Pts',(2.82095928310699,-1.26486419330493,-3.34416493233204E-16));
#19768=CARTESIAN_POINT('Ctrl Pts',(2.8624634969724,-1.29312108144354,-1.56006819163429E-15));
#19769=CARTESIAN_POINT('Ctrl Pts',(2.90551195584779,-1.31904027763685,-2.77555756156289E-17));
#19770=CARTESIAN_POINT('Ctrl Pts',(2.8546922928873,0.958179197573794,0.000498685380349445));
#19771=CARTESIAN_POINT('Ctrl Pts',(2.85850481197628,0.960904068967743,0.000332456920233391));
#19772=CARTESIAN_POINT('Ctrl Pts',(2.86233359432805,0.963606185523634,0.000166228460117303));
#19773=CARTESIAN_POINT('Ctrl Pts',(2.86617836717395,0.966285354738298,1.2490009027033E-15));
#19774=CARTESIAN_POINT('Ctrl Pts',(4.39104028268295,1.19243523336309,0.166013505999356));
#19775=CARTESIAN_POINT('Ctrl Pts',(4.78573455009837,0.910593977022875,0.139673936462541));
#19776=CARTESIAN_POINT('Ctrl Pts',(5.26671040851744,-0.0705935126856522,
0.0870010883098722));
#19777=CARTESIAN_POINT('Ctrl Pts',(4.42236229737626,-1.48797440454215,0.00799496154134886));
#19778=CARTESIAN_POINT('Ctrl Pts',(2.77646556351823,-1.55100085572438,-0.0710048743062135));
#19779=CARTESIAN_POINT('Ctrl Pts',(1.8231817769065,-0.209126570759914,-0.150004710153776));
#19780=CARTESIAN_POINT('Ctrl Pts',(2.4267807654254,1.3236028845817,-0.229004546001338));
#19781=CARTESIAN_POINT('Ctrl Pts',(4.03996554970546,1.65495464231977,-0.308004381848901));
#19782=CARTESIAN_POINT('Ctrl Pts',(5.19908829746563,0.485231098250064,-0.387004217696463));
#19783=CARTESIAN_POINT('Ctrl Pts',(4.85266468272742,-1.12486221135666,-0.466004053544026));
#19784=CARTESIAN_POINT('Ctrl Pts',(3.31493037813578,-1.71438530937678,-0.545003889391588));
#19785=CARTESIAN_POINT('Ctrl Pts',(1.98095238924354,-0.748650010516562,
-0.624003725239151));
#19786=CARTESIAN_POINT('Ctrl Pts',(2.06091425900795,0.896290333456293,-0.703003561086713));
#19787=CARTESIAN_POINT('Ctrl Pts',(3.48228013532258,1.7280964959961,-0.782003396934276));
#19788=CARTESIAN_POINT('Ctrl Pts',(4.95557248446353,0.992166550039036,-0.861003232781839));
#19789=CARTESIAN_POINT('Ctrl Pts',(5.14421062951873,-0.643868150032796,
-0.9400030686294));
#19790=CARTESIAN_POINT('Ctrl Pts',(3.87705966552992,-1.6957787847533,-1.01900290447696));
#19791=CARTESIAN_POINT('Ctrl Pts',(2.30368936823014,-1.20926655124093,-1.09800274032452));
#19792=CARTESIAN_POINT('Ctrl Pts',(1.85147337579044,0.374302296113376,-1.17700257617209));
#19793=CARTESIAN_POINT('Ctrl Pts',(2.93066571761574,1.61830089654537,-1.25600241201965));
#19794=CARTESIAN_POINT('Ctrl Pts',(4.56221455954657,1.394164357391,-1.33500224786721));
#19795=CARTESIAN_POINT('Ctrl Pts',(5.26596601862656,-0.0947691059850859,
-1.41400208371477));
#19796=CARTESIAN_POINT('Ctrl Pts',(4.40347122688333,-1.49772725382214,-1.49300191956234));
#19797=CARTESIAN_POINT('Ctrl Pts',(2.75719224100921,-1.54193549825478,-1.5720017554099));
#19798=CARTESIAN_POINT('Ctrl Pts',(1.82064627705295,-0.187287741932202,
-1.65100159125746));
#19799=CARTESIAN_POINT('Ctrl Pts',(2.44347518930979,1.33726891870949,-1.73000142710503));
#19800=CARTESIAN_POINT('Ctrl Pts',(4.06064369715841,1.64864472003992,-1.80900126295258));
#19801=CARTESIAN_POINT('Ctrl Pts',(5.20504383428331,0.464357085917297,-1.88800109880015));
#19802=CARTESIAN_POINT('Ctrl Pts',(4.83846681093798,-1.14119894150869,-1.96700093464771));
#19803=CARTESIAN_POINT('Ctrl Pts',(3.29347418099175,-1.71145032981342,-2.04600077049527));
#19804=CARTESIAN_POINT('Ctrl Pts',(1.97169538830959,-0.729060541700552,
-2.12500060634284));
#19805=CARTESIAN_POINT('Ctrl Pts',(2.07225853125702,0.914738693744935,-2.2040004421904));
#19806=CARTESIAN_POINT('Ctrl Pts',(3.50393193697739,1.72867980446563,-2.28300027803796));
#19807=CARTESIAN_POINT('Ctrl Pts',(4.96789025142369,0.974349024284007,-2.36200011388552));
#19808=CARTESIAN_POINT('Ctrl Pts',(5.13601899785199,-0.663918840546727,
-2.44099994973308));
#19809=CARTESIAN_POINT('Ctrl Pts',(3.85579045748996,-1.69987432066465,-2.51999978558065));
#19810=CARTESIAN_POINT('Ctrl Pts',(2.28863801351722,-1.19369047097085,-2.59899962142821));
#19811=CARTESIAN_POINT('Ctrl Pts',(1.85629466717739,0.395418745920643,-2.67799945727578));
#19812=CARTESIAN_POINT('Ctrl Pts',(2.95098569669531,1.62580097199172,-2.75699929312333));
#19813=CARTESIAN_POINT('Ctrl Pts',(4.57959880542434,1.38124379173793,-2.8359991289709));
#19814=CARTESIAN_POINT('Ctrl Pts',(5.26464339451333,-0.11638860083937,-2.91499896481845));
#19815=CARTESIAN_POINT('Ctrl Pts',(4.38464163429993,-1.508432340942,-2.99399880066603));
#19816=CARTESIAN_POINT('Ctrl Pts',(2.73793803074369,-1.53201441829649,-3.07299863651358));
#19817=CARTESIAN_POINT('Ctrl Pts',(1.81843502163546,-0.165740987178738,
-3.15199847236115));
#19818=CARTESIAN_POINT('Ctrl Pts',(2.46031295606552,1.35089396877779,-3.23099830820871));
#19819=CARTESIAN_POINT('Ctrl Pts',(4.08125513238924,1.64198731008323,-3.30999814405628));
#19820=CARTESIAN_POINT('Ctrl Pts',(5.21073008185995,0.443456872065259,-3.38899797990383));
#19821=CARTESIAN_POINT('Ctrl Pts',(4.82406926255307,-1.1573811219711,-3.4679978157514));
#19822=CARTESIAN_POINT('Ctrl Pts',(3.27205440550583,-1.7082338752928,-3.54699765159896));
#19823=CARTESIAN_POINT('Ctrl Pts',(1.96268557425322,-0.709363445216102,
-3.62599748744653));
#19824=CARTESIAN_POINT('Ctrl Pts',(2.08383245266016,0.933047071734419,-3.70499732329408));
#19825=CARTESIAN_POINT('Ctrl Pts',(3.52558964148418,1.72898995964266,-3.78399715914165));
#19826=CARTESIAN_POINT('Ctrl Pts',(4.97998369946044,0.956379581469577,-3.86299699498921));
#19827=CARTESIAN_POINT('Ctrl Pts',(5.12757691841429,-0.683865861766359,
-3.94199683083677));
#19828=CARTESIAN_POINT('Ctrl Pts',(3.83447157132285,-1.7037028260214,-4.02099666668433));
#19829=CARTESIAN_POINT('Ctrl Pts',(2.27378298153172,-1.17792721035138,-4.0999965025319));
#19830=CARTESIAN_POINT('Ctrl Pts',(1.86138009102058,0.416473218723921,-4.17899633837946));
#19831=CARTESIAN_POINT('Ctrl Pts',(2.97139803993003,1.63304587394689,-4.25799617422703));
#19832=CARTESIAN_POINT('Ctrl Pts',(4.59681983000601,1.36810649091058,-4.33699601007458));
#19833=CARTESIAN_POINT('Ctrl Pts',(5.26305005173533,-0.137989841995099,
-4.41599584592215));
#19834=CARTESIAN_POINT('Ctrl Pts',(4.36567941724011,-1.51890070685318,-4.49499568176971));
#19835=CARTESIAN_POINT('Ctrl Pts',(2.71880961159543,-1.52185292521907,-4.57399551761728));
#19836=CARTESIAN_POINT('Ctrl Pts',(1.81649385243162,-0.144168221412696,
-4.65299535346484));
#19837=CARTESIAN_POINT('Ctrl Pts',(2.47732008074839,1.36430702475679,-4.7319951893124));
#19838=CARTESIAN_POINT('Ctrl Pts',(4.1017815539197,1.63507222658209,-4.81099502515996));
#19839=CARTESIAN_POINT('Ctrl Pts',(5.21615406946798,0.422487067128113,-4.88999486100753));
#19840=CARTESIAN_POINT('Ctrl Pts',(4.8094701320957,-1.17338167666657,-4.96899469685509));
#19841=CARTESIAN_POINT('Ctrl Pts',(3.25067660275509,-1.70474935090286,-5.04799453270265));
#19842=CARTESIAN_POINT('Ctrl Pts',(1.95392320970657,-0.689555029625102,
-5.12699436855021));
#19843=CARTESIAN_POINT('Ctrl Pts',(2.09563481222965,0.951209028381946,-5.20599420439778));
#19844=CARTESIAN_POINT('Ctrl Pts',(3.54724953190536,1.72902878768242,-5.28499404024534));
#19845=CARTESIAN_POINT('Ctrl Pts',(4.9918510980865,0.938260055799061,-5.3639938760929));
#19846=CARTESIAN_POINT('Ctrl Pts',(5.11888562803801,-0.703705565198355,
-5.44299371194047));
#19847=CARTESIAN_POINT('Ctrl Pts',(3.81310639881089,-1.70726397249534,-5.52199354778801));
#19848=CARTESIAN_POINT('Ctrl Pts',(2.25912657912977,-1.16197909982672,-5.60099338363559));
#19849=CARTESIAN_POINT('Ctrl Pts',(1.86672886205842,0.43746233516695,-5.67999321948314));
#19850=CARTESIAN_POINT('Ctrl Pts',(2.99189953732774,1.64003450508086,-5.75899305533072));
#19851=CARTESIAN_POINT('Ctrl Pts',(4.61387493436243,1.35475449570142,-5.83799289117827));
#19852=CARTESIAN_POINT('Ctrl Pts',(5.26118623847484,-0.159569428664093,
-5.91699272702583));
#19853=CARTESIAN_POINT('Ctrl Pts',(4.34658755238584,-1.52913071452965,-5.99599256287339));
#19854=CARTESIAN_POINT('Ctrl Pts',(2.69980998483775,-1.5114526106208,-6.07499239872097));
#19855=CARTESIAN_POINT('Ctrl Pts',(1.81482307433549,-0.122572831598478,
-6.15399223456852));
#19856=CARTESIAN_POINT('Ctrl Pts',(2.49449389432028,1.37750598259717,-6.23299207041608));
#19857=CARTESIAN_POINT('Ctrl Pts',(4.12221974065168,1.62790055426783,-6.31199190626365));
#19858=CARTESIAN_POINT('Ctrl Pts',(5.22131494589194,0.401450962089136,-6.39099174211121));
#19859=CARTESIAN_POINT('Ctrl Pts',(4.79467171060061,-1.18919809477965,-6.46999157795877));
#19860=CARTESIAN_POINT('Ctrl Pts',(3.22934412750707,-1.70099730339957,-6.54899141380633));
#19861=CARTESIAN_POINT('Ctrl Pts',(1.94540966973674,-0.669638403458603,
-6.62799124965391));
#19862=CARTESIAN_POINT('Ctrl Pts',(2.10766375784038,0.969221713583442,-6.70699108550145));
#19863=CARTESIAN_POINT('Ctrl Pts',(3.56890820919659,1.72879628248244,-6.78599092134903));
#19864=CARTESIAN_POINT('Ctrl Pts',(5.00349058497245,0.919993290740459,-6.86499075719659));
#19865=CARTESIAN_POINT('Ctrl Pts',(5.10994649063147,-0.723434837437879,
-6.94399059304415));
#19866=CARTESIAN_POINT('Ctrl Pts',(3.79169829275028,-1.71055720124108,-7.02299042889171));
#19867=CARTESIAN_POINT('Ctrl Pts',(2.24467110631318,-1.14584864210466,-7.10199026473928));
#19868=CARTESIAN_POINT('Ctrl Pts',(1.87234014091828,0.458382801467482,-7.18099010058684));
#19869=CARTESIAN_POINT('Ctrl Pts',(3.01248697162693,1.64676576868065,-7.2599899364344));
#19870=CARTESIAN_POINT('Ctrl Pts',(4.63076144206815,1.34118990141411,-7.33898977228196));
#19871=CARTESIAN_POINT('Ctrl Pts',(5.25905224721656,-0.181123974402424,
-7.41798960812953));
#19872=CARTESIAN_POINT('Ctrl Pts',(4.32736903578763,-1.53912075859537,-7.49698944397708));
#19873=CARTESIAN_POINT('Ctrl Pts',(2.68094213204631,-1.50081510660373,-7.57598927982465));
#19874=CARTESIAN_POINT('Ctrl Pts',(1.81342294953926,-0.100958206659705,
-7.6549891156722));
#19875=CARTESIAN_POINT('Ctrl Pts',(2.51183170172664,1.3904887710106,-7.73398895151979));
#19876=CARTESIAN_POINT('Ctrl Pts',(4.14256648525937,1.62047341857881,-7.81298878736733));
#19877=CARTESIAN_POINT('Ctrl Pts',(5.22621190124433,0.380351858102332,-7.89198862321491));
#19878=CARTESIAN_POINT('Ctrl Pts',(4.77967632035796,-1.20482789426491,-7.97098845906245));
#19879=CARTESIAN_POINT('Ctrl Pts',(3.20806032742391,-1.69697832159357,-8.04998829491003));
#19880=CARTESIAN_POINT('Ctrl Pts',(1.93714629036355,-0.649616692178436,
-8.12898813075759));
#19881=CARTESIAN_POINT('Ctrl Pts',(2.11991740180112,0.987082300609951,-8.20798796660515));
#19882=CARTESIAN_POINT('Ctrl Pts',(3.590562274524,1.72829248059039,-8.28698780245271));
#19883=CARTESIAN_POINT('Ctrl Pts',(5.01490033351429,0.901582152746688,-8.36598763830028));
#19884=CARTESIAN_POINT('Ctrl Pts',(5.100760909075,-0.743050582186251,-8.44498747414783));
#19885=CARTESIAN_POINT('Ctrl Pts',(3.77025061252596,-1.71358199587885,-8.52398730999541));
#19886=CARTESIAN_POINT('Ctrl Pts',(2.23041883183543,-1.12953836770797,-8.60298714584296));
#19887=CARTESIAN_POINT('Ctrl Pts',(1.87821304649392,0.479231333095078,-8.68198698169053));
#19888=CARTESIAN_POINT('Ctrl Pts',(3.03315711310502,1.65323861131456,-8.76098681753808));
#19889=CARTESIAN_POINT('Ctrl Pts',(4.64747670120603,1.32741483121271,-8.83998665338566));
#19890=CARTESIAN_POINT('Ctrl Pts',(5.25664841655105,-0.202650086230401,
-8.9189864892332));
#19891=CARTESIAN_POINT('Ctrl Pts',(4.30802687631991,-1.54886929123672,-8.99798632508078));
#19892=CARTESIAN_POINT('Ctrl Pts',(2.6622090275294,-1.48994204463143,-9.07698616092833));
#19893=CARTESIAN_POINT('Ctrl Pts',(1.81229367225287,-0.0793278105488914,
-9.15598599677591));
#19894=CARTESIAN_POINT('Ctrl Pts',(2.52933083069636,1.40325348959643,-9.23498583262345));
#19895=CARTESIAN_POINT('Ctrl Pts',(4.16281850248374,1.61279172453447,-9.31398566847103));
#19896=CARTESIAN_POINT('Ctrl Pts',(5.23084434257772,0.359193561697825,-9.39298550431858));
#19897=CARTESIAN_POINT('Ctrl Pts',(4.76448598072016,-1.22026956478995,-9.47198534016615));
#19898=CARTESIAN_POINT('Ctrl Pts',(3.18682917751138,-1.69269124367719,-9.55098517601371));
#19899=CARTESIAN_POINT('Ctrl Pts',(1.92913316060619,-0.629496447108055,
-9.62998501186127));
#19900=CARTESIAN_POINT('Ctrl Pts',(2.13239611830123,1.00479447126442,-9.70898484770884));
#19901=CARTESIAN_POINT('Ctrl Pts',(3.61220396058553,1.7275051272171,-9.7879846835564));
#19902=CARTESIAN_POINT('Ctrl Pts',(5.02608686342242,0.883052990217761,-9.86698451940395));
#19903=CARTESIAN_POINT('Ctrl Pts',(5.09131451863736,-0.762594341224724,
-9.94598435525153));
#19904=CARTESIAN_POINT('Ctrl Pts',(3.7487967880808,-1.71625301028161,-10.0249841910991));
#19905=CARTESIAN_POINT('Ctrl Pts',(2.21631480459542,-1.11321229367821,-10.1039840269467));
#19906=CARTESIAN_POINT('Ctrl Pts',(1.88445547370457,0.500312018724167,-10.1829838627942));
#19907=CARTESIAN_POINT('Ctrl Pts',(3.05369936202752,1.65886512673652,-10.2619836986418));
#19908=CARTESIAN_POINT('Ctrl Pts',(4.66441579808227,1.31456735634548,-10.3409835344894));
#19909=CARTESIAN_POINT('Ctrl Pts',(5.25318976192693,-0.226472583690619,
-10.4199833703369));
#19910=CARTESIAN_POINT('Ctrl Pts',(4.61130290174357,-1.11057344913152,-10.4726499275686));
#19911=CARTESIAN_POINT('Ctrl Pts',(4.17428909295502,-1.32062757704312,-10.4989832061845));
#19912=CARTESIAN_POINT('Ctrl Pts',(4.33494771810971,1.113885518109,0.110286691365708));
#19913=CARTESIAN_POINT('Ctrl Pts',(4.70364214800736,0.850610092275097,0.083947121828893));
#19914=CARTESIAN_POINT('Ctrl Pts',(5.15293451061394,-0.065943280819724,
0.0312742736762238));
#19915=CARTESIAN_POINT('Ctrl Pts',(4.36420644645715,-1.38995653110804,-0.0477318530922994));
#19916=CARTESIAN_POINT('Ctrl Pts',(2.82673046046441,-1.44883121818993,-0.126731688939862));
#19917=CARTESIAN_POINT('Ctrl Pts',(1.9362426797905,-0.195350700904968,-0.205731524787425));
#19918=CARTESIAN_POINT('Ctrl Pts',(2.50008057491893,1.23641271543502,-0.284731360634987));
#19919=CARTESIAN_POINT('Ctrl Pts',(4.00699945736041,1.54593721959065,-0.363731196482549));
#19920=CARTESIAN_POINT('Ctrl Pts',(5.0897668952189,0.453267295492844,-0.442731032330112));
#19921=CARTESIAN_POINT('Ctrl Pts',(4.76616336792331,-1.050763758099,-0.521730868177675));
#19922=CARTESIAN_POINT('Ctrl Pts',(3.32972478856904,-1.60145298892903,-0.600730704025237));
#19923=CARTESIAN_POINT('Ctrl Pts',(2.08362041180346,-0.69933391895392,-0.6797305398728));
#19924=CARTESIAN_POINT('Ctrl Pts',(2.15831492454466,0.837248677768694,-0.758730375720361));
#19925=CARTESIAN_POINT('Ctrl Pts',(3.4860506549758,1.61426097361787,-0.837730211567926));
#19926=CARTESIAN_POINT('Ctrl Pts',(4.86229228700177,0.926809205833092,-0.916730047415487));
#19927=CARTESIAN_POINT('Ctrl Pts',(5.03850420364174,-0.601454391674104,
-0.99572988326305));
#19928=CARTESIAN_POINT('Ctrl Pts',(3.85482473111879,-1.58407213859808,-1.07472971911061));
#19929=CARTESIAN_POINT('Ctrl Pts',(2.38509762162855,-1.12960810052711,-1.15372955495818));
#19930=CARTESIAN_POINT('Ctrl Pts',(1.96267061599973,0.349645746259735,-1.23272939080574));
#19931=CARTESIAN_POINT('Ctrl Pts',(2.97077293231841,1.51169797920237,-1.3117292266533));
#19932=CARTESIAN_POINT('Ctrl Pts',(4.49484617023228,1.30232606695269,-1.39072906250087));
#19933=CARTESIAN_POINT('Ctrl Pts',(5.15223915618622,-0.08852634656157,-1.46972889834842));
#19934=CARTESIAN_POINT('Ctrl Pts',(4.3465597942492,-1.3990669274376,-1.54872873419599));
#19935=CARTESIAN_POINT('Ctrl Pts',(2.80872673646503,-1.44036302627531,-1.62772857004355));
#19936=CARTESIAN_POINT('Ctrl Pts',(1.93387420183125,-0.174950469107858,
-1.70672840589111));
#19937=CARTESIAN_POINT('Ctrl Pts',(2.5156752810109,1.24917852197866,-1.78572824173868));
#19938=CARTESIAN_POINT('Ctrl Pts',(4.02631546576466,1.5400429530919,-1.86472807758624));
#19939=CARTESIAN_POINT('Ctrl Pts',(5.09533012081654,0.433768324486494,-1.9437279134338));
#19940=CARTESIAN_POINT('Ctrl Pts',(4.75290075765169,-1.06602433294655,-2.02272774928136));
#19941=CARTESIAN_POINT('Ctrl Pts',(3.30968198322101,-1.59871134633068,-2.10172758512893));
#19942=CARTESIAN_POINT('Ctrl Pts',(2.07497320062339,-0.681034874266973,
-2.18072742097649));
#19943=CARTESIAN_POINT('Ctrl Pts',(2.16891191146536,0.854481782580953,-2.25972725682405));
#19944=CARTESIAN_POINT('Ctrl Pts',(3.50627617970828,1.61480585759867,-2.33872709267161));
#19945=CARTESIAN_POINT('Ctrl Pts',(4.87379864126613,0.910165380364193,-2.41772692851917));
#19946=CARTESIAN_POINT('Ctrl Pts',(5.03085218227572,-0.620184275836084,
-2.49672676436674));
#19947=CARTESIAN_POINT('Ctrl Pts',(3.8349565972743,-1.58789788779847,-2.5757266002143));
#19948=CARTESIAN_POINT('Ctrl Pts',(2.37103775022121,-1.1150580689981,-2.65472643606186));
#19949=CARTESIAN_POINT('Ctrl Pts',(1.96717431272409,0.369371184569583,-2.73372627190943));
#19950=CARTESIAN_POINT('Ctrl Pts',(2.98975436610342,1.51870399947977,-2.81272610775699));
#19951=CARTESIAN_POINT('Ctrl Pts',(4.51108525742519,1.29025662237067,-2.89172594360455));
#19952=CARTESIAN_POINT('Ctrl Pts',(5.15100365776719,-0.108721692651017,
-2.97072577945211));
#19953=CARTESIAN_POINT('Ctrl Pts',(4.32897057019432,-1.40906683450114,-3.04972561529968));
#19954=CARTESIAN_POINT('Ctrl Pts',(2.79074086572141,-1.43109548118747,-3.12872545114724));
#19955=CARTESIAN_POINT('Ctrl Pts',(1.93180860923765,-0.154823071484393,
-3.2077252869948));
#19956=CARTESIAN_POINT('Ctrl Pts',(2.53140388749766,1.2619060442205,-3.28672512284236));
#19957=CARTESIAN_POINT('Ctrl Pts',(4.045569156505,1.53382408909712,-3.36572495868993));
#19958=CARTESIAN_POINT('Ctrl Pts',(5.10064179616025,0.41424487794298,-3.44472479453749));
#19959=CARTESIAN_POINT('Ctrl Pts',(4.73945162415284,-1.08114053881181,-3.52372463038505));
#19960=CARTESIAN_POINT('Ctrl Pts',(3.28967320031411,-1.59570677047621,-3.60272446623261));
#19961=CARTESIAN_POINT('Ctrl Pts',(2.06655689329076,-0.662635291707721,
-3.68172430208018));
#19962=CARTESIAN_POINT('Ctrl Pts',(2.17972341977875,0.871584126198421,-3.76072413792774));
#19963=CARTESIAN_POINT('Ctrl Pts',(3.52650721845205,1.6150955818121,-3.8397239737753));
#19964=CARTESIAN_POINT('Ctrl Pts',(4.88509545324823,0.893379645123019,-3.91872380962286));
#19965=CARTESIAN_POINT('Ctrl Pts',(5.02296621097492,-0.638817319748494,
-3.99772364547043));
#19966=CARTESIAN_POINT('Ctrl Pts',(3.81504205776779,-1.59147419664407,-4.07672348131799));
#19967=CARTESIAN_POINT('Ctrl Pts',(2.35716126910365,-1.10033318731819,-4.15572331716555));
#19968=CARTESIAN_POINT('Ctrl Pts',(1.97192474261234,0.389038728508927,-4.23472315301311));
#19969=CARTESIAN_POINT('Ctrl Pts',(3.00882207970637,1.52547165540118,-4.31372298886068));
#19970=CARTESIAN_POINT('Ctrl Pts',(4.52717187525719,1.2779847196885,-4.39272282470824));
#19971=CARTESIAN_POINT('Ctrl Pts',(5.1495152738314,-0.128899987474363,-4.4717226605558));
#19972=CARTESIAN_POINT('Ctrl Pts',(4.31125745808291,-1.41884561397736,-4.55072249640336));
#19973=CARTESIAN_POINT('Ctrl Pts',(2.77287249981153,-1.42160335980039,-4.62972233225093));
#19974=CARTESIAN_POINT('Ctrl Pts',(1.92999531137135,-0.13467137628114,-4.70872216809848));
#19975=CARTESIAN_POINT('Ctrl Pts',(2.54729069573586,1.27443553713597,-4.78772200394605));
#19976=CARTESIAN_POINT('Ctrl Pts',(4.06474343368305,1.52736452538001,-4.86672183979361));
#19977=CARTESIAN_POINT('Ctrl Pts',(5.10570848748063,0.394656424512951,-4.94572167564119));
#19978=CARTESIAN_POINT('Ctrl Pts',(4.72581418746994,-1.09608708320963,-5.02472151148873));
#19979=CARTESIAN_POINT('Ctrl Pts',(3.26970362525728,-1.59245178341539,-5.10372134733631));
#19980=CARTESIAN_POINT('Ctrl Pts',(2.05837173513724,-0.644131723005486,
-5.18272118318386));
#19981=CARTESIAN_POINT('Ctrl Pts',(2.19074831826896,0.888549693739684,-5.26172101903143));
#19982=CARTESIAN_POINT('Ctrl Pts',(3.54674029911668,1.61513185211844,-5.34072085487899));
#19983=CARTESIAN_POINT('Ctrl Pts',(4.89618110645381,0.876453713487748,-5.41972069072655));
#19984=CARTESIAN_POINT('Ctrl Pts',(5.01484744509737,-0.657350115256517,
-5.49872052657412));
#19985=CARTESIAN_POINT('Ctrl Pts',(3.79508428095349,-1.59480075843476,-5.57772036242167));
#19986=CARTESIAN_POINT('Ctrl Pts',(2.34347033317158,-1.08543563241745,-5.65672019826925));
#19987=CARTESIAN_POINT('Ctrl Pts',(1.97692117213072,0.408645221331059,-5.73572003411679));
#19988=CARTESIAN_POINT('Ctrl Pts',(3.02797307458803,1.53199992192143,-5.81471986996437));
#19989=CARTESIAN_POINT('Ctrl Pts',(4.54310350258665,1.26551226526479,-5.89371970581192));
#19990=CARTESIAN_POINT('Ctrl Pts',(5.14777423621256,-0.149058054264775,
-5.97271954165949));
#19991=CARTESIAN_POINT('Ctrl Pts',(4.29342323851284,-1.42840173667663,-6.05171937750705));
#19992=CARTESIAN_POINT('Ctrl Pts',(2.75512444230473,-1.41188814886847,-6.13071921335461));
#19993=CARTESIAN_POINT('Ctrl Pts',(1.92843459304201,-0.114498547351779,
-6.20971904920218));
#19994=CARTESIAN_POINT('Ctrl Pts',(2.56333321250591,1.28676503527658,-6.28871888504973));
#19995=CARTESIAN_POINT('Ctrl Pts',(4.08383528838526,1.52066527521701,-6.3677187208973));
#19996=CARTESIAN_POINT('Ctrl Pts',(5.11052939963465,0.37500603839156,-6.44671855674487));
#19997=CARTESIAN_POINT('Ctrl Pts',(4.71199058771956,-1.11086162072043,-6.52571839259242));
#19998=CARTESIAN_POINT('Ctrl Pts',(3.24977639182829,-1.58894689588755,-6.60471822843999));
#19999=CARTESIAN_POINT('Ctrl Pts',(2.05041901064964,-0.625527071921937,
-6.68371806428756));
#20000=CARTESIAN_POINT('Ctrl Pts',(2.20198487681655,0.905375822846601,-6.7627179001351));
#20001=CARTESIAN_POINT('Ctrl Pts',(3.5669722465643,1.61491466281716,-6.84171773598269));
#20002=CARTESIAN_POINT('Ctrl Pts',(4.90705386123136,0.859390241617592,-6.92071757183023));
#20003=CARTESIAN_POINT('Ctrl Pts',(5.00649715870617,-0.675779754045749,
-6.99971740767781));
#20004=CARTESIAN_POINT('Ctrl Pts',(3.77508639876763,-1.59787705113819,-7.07871724352536));
#20005=CARTESIAN_POINT('Ctrl Pts',(2.32996709091799,-1.07036774214185,-7.15771707937293));
#20006=CARTESIAN_POINT('Ctrl Pts',(1.98216281719889,0.428187586226241,-7.23671691522048));
#20007=CARTESIAN_POINT('Ctrl Pts',(3.04720434541876,1.53828777457171,-7.31571675106806));
#20008=CARTESIAN_POINT('Ctrl Pts',(4.55887763929323,1.25284121637851,-7.3947165869156));
#20009=CARTESIAN_POINT('Ctrl Pts',(5.14578081812842,-0.169192729654759,
-7.47371642276319));
#20010=CARTESIAN_POINT('Ctrl Pts',(4.27547071017476,-1.43773370297445,-7.55271625861073));
#20011=CARTESIAN_POINT('Ctrl Pts',(2.73749947837029,-1.40195137298167,-7.6317160944583));
#20012=CARTESIAN_POINT('Ctrl Pts',(1.92712669917035,-0.0943077503801438,
-7.71071593030587));
#20013=CARTESIAN_POINT('Ctrl Pts',(2.57952892028556,1.29889260379668,-7.78971576615342));
#20014=CARTESIAN_POINT('Ctrl Pts',(4.10284172456313,1.51372738991008,-7.868715602001));
#20015=CARTESIAN_POINT('Ctrl Pts',(5.11510377608481,0.355296803274704,-7.94771543784854));
#20016=CARTESIAN_POINT('Ctrl Pts',(4.69798299421482,-1.12546183279944,-8.02671527369611));
#20017=CARTESIAN_POINT('Ctrl Pts',(3.2298946271675,-1.58519265791639,-8.10571510954367));
#20018=CARTESIAN_POINT('Ctrl Pts',(2.04269996783968,-0.606824258034226,
-8.18471494539124));
#20019=CARTESIAN_POINT('Ctrl Pts',(2.21343133207891,0.922059872996347,-8.2637147812388));
#20020=CARTESIAN_POINT('Ctrl Pts',(3.58719988585365,1.61444404804845,-8.34271461708637));
#20021=CARTESIAN_POINT('Ctrl Pts',(4.91771201130145,0.842191907142578,-8.42171445293392));
#20022=CARTESIAN_POINT('Ctrl Pts',(4.99791666226923,-0.69410334378111,-8.50071428878149));
#20023=CARTESIAN_POINT('Ctrl Pts',(3.75505154930119,-1.60070259239024,-8.57971412462905));
#20024=CARTESIAN_POINT('Ctrl Pts',(2.31665366164594,-1.05513188032014,-8.65871396047662));
#20025=CARTESIAN_POINT('Ctrl Pts',(1.98764885475204,0.44766275502708,-8.73771379632417));
#20026=CARTESIAN_POINT('Ctrl Pts',(3.06651287522861,1.5443342293134,-8.81671363217174));
#20027=CARTESIAN_POINT('Ctrl Pts',(4.57449180815055,1.23997355633378,-8.8957134680193));
#20028=CARTESIAN_POINT('Ctrl Pts',(5.1435353358654,-0.189300844171595,-8.97471330386686));
#20029=CARTESIAN_POINT('Ctrl Pts',(4.2574026837384,-1.44684006701688,-9.05371313971443));
#20030=CARTESIAN_POINT('Ctrl Pts',(2.72000038638879,-1.3917945561336,-9.13271297556199));
#20031=CARTESIAN_POINT('Ctrl Pts',(1.92607181117305,-0.0741022211365624,
-9.21171281140954));
#20032=CARTESIAN_POINT('Ctrl Pts',(2.59587532283516,1.31081646748141,-9.29071264725712));
#20033=CARTESIAN_POINT('Ctrl Pts',(4.12175967336872,1.50655171486196,-9.36971248310467));
#20034=CARTESIAN_POINT('Ctrl Pts',(5.11943106294313,0.335532274943578,-9.44871231895224));
#20035=CARTESIAN_POINT('Ctrl Pts',(4.68379329328662,-1.13988630860492,-9.52771215479979));
#20036=CARTESIAN_POINT('Ctrl Pts',(3.21006204443369,-1.58118798422641,-9.60671199064737));
#20037=CARTESIAN_POINT('Ctrl Pts',(2.03521468986255,-0.588029401108125,
-9.68571182649492));
#20038=CARTESIAN_POINT('Ctrl Pts',(2.22508803359624,0.938605283459143,-9.76471166234249));
#20039=CARTESIAN_POINT('Ctrl Pts',(3.60741596134095,1.61370856028727,-9.84371149819005));
#20040=CARTESIAN_POINT('Ctrl Pts',(4.92816164689921,0.824883322805087,-9.92271133403761));
#20041=CARTESIAN_POINT('Ctrl Pts',(4.9890925373084,-0.712359689747145,-10.0017111698852));
#20042=CARTESIAN_POINT('Ctrl Pts',(3.7350109603544,-1.60319765810002,-10.0807110057327));
#20043=CARTESIAN_POINT('Ctrl Pts',(2.30347871406799,-1.03988125964027,-10.1597108415803));
#20044=CARTESIAN_POINT('Ctrl Pts',(1.99348007230855,0.467354785065328,-10.2387106774279));
#20045=CARTESIAN_POINT('Ctrl Pts',(3.0857019371952,1.54959010726013,-10.3177105132754));
#20046=CARTESIAN_POINT('Ctrl Pts',(4.59031506980232,1.22797238780195,-10.396710349123));
#20047=CARTESIAN_POINT('Ctrl Pts',(5.14030451444203,-0.211554073683514,
-10.4757101849706));
#20048=CARTESIAN_POINT('Ctrl Pts',(4.54070089839809,-1.03741624465007,-10.5283767422023));
#20049=CARTESIAN_POINT('Ctrl Pts',(4.1324746575059,-1.23363340140067,-10.5547100208181));
#20050=CARTESIAN_POINT('Ctrl Pts',(4.27885515353647,1.0353358028549,0.0545598767320594));
#20051=CARTESIAN_POINT('Ctrl Pts',(4.62154974591635,0.790626207527318,0.0282203071952445));
#20052=CARTESIAN_POINT('Ctrl Pts',(5.03915861271046,-0.0612930489537958,
-0.0244525409574245));
#20053=CARTESIAN_POINT('Ctrl Pts',(4.30605059553801,-1.29193865767393,-0.103458667725947));
#20054=CARTESIAN_POINT('Ctrl Pts',(2.87699535741062,-1.34666158065549,-0.18245850357351));
#20055=CARTESIAN_POINT('Ctrl Pts',(2.04930358267447,-0.181574831050025,
-0.261458339421073));
#20056=CARTESIAN_POINT('Ctrl Pts',(2.57338038441246,1.14922254628835,-0.340458175268635));
#20057=CARTESIAN_POINT('Ctrl Pts',(3.97403336501536,1.4369197968615,-0.419458011116198));
#20058=CARTESIAN_POINT('Ctrl Pts',(4.9804454929722,0.421303492735624,-0.498457846963761));
#20059=CARTESIAN_POINT('Ctrl Pts',(4.67966205311918,-0.976665304841327,
-0.577457682811322));
#20060=CARTESIAN_POINT('Ctrl Pts',(3.3445191990023,-1.48852066848128,-0.656457518658885));
#20061=CARTESIAN_POINT('Ctrl Pts',(2.18628843436339,-0.650017827391278,
-0.735457354506447));
#20062=CARTESIAN_POINT('Ctrl Pts',(2.25571559008138,0.778207022081096,-0.814457190354011));
#20063=CARTESIAN_POINT('Ctrl Pts',(3.48982117462903,1.50042545123965,-0.893457026201572));
#20064=CARTESIAN_POINT('Ctrl Pts',(4.76901208954002,0.861451861627147,-0.972456862049136));
#20065=CARTESIAN_POINT('Ctrl Pts',(4.93279777776475,-0.559040633315412,
-1.0514566978967));
#20066=CARTESIAN_POINT('Ctrl Pts',(3.83258979670766,-1.47236549244286,-1.13045653374427));
#20067=CARTESIAN_POINT('Ctrl Pts',(2.46650587502695,-1.04994964981329,-1.20945636959183));
#20068=CARTESIAN_POINT('Ctrl Pts',(2.07386785620901,0.324989196406094,-1.28845620543939));
#20069=CARTESIAN_POINT('Ctrl Pts',(3.01088014702108,1.40509506185938,-1.36745604128694));
#20070=CARTESIAN_POINT('Ctrl Pts',(4.42747778091797,1.21048777651438,-1.44645587713451));
#20071=CARTESIAN_POINT('Ctrl Pts',(5.0385122937459,-0.0822835871380551,
-1.52545571298208));
#20072=CARTESIAN_POINT('Ctrl Pts',(4.28964836161505,-1.30040660105306,-1.60445554882964));
#20073=CARTESIAN_POINT('Ctrl Pts',(2.86026123192082,-1.33879055429585,-1.68345538467719));
#20074=CARTESIAN_POINT('Ctrl Pts',(2.04710212660955,-0.162613196283514,
-1.76245522052476));
#20075=CARTESIAN_POINT('Ctrl Pts',(2.58787537271199,1.16108812524782,-1.84145505637233));
#20076=CARTESIAN_POINT('Ctrl Pts',(3.99198723437091,1.43144118614388,-1.92045489221988));
#20077=CARTESIAN_POINT('Ctrl Pts',(4.98561640734979,0.40317956305569,-1.99945472806744));
#20078=CARTESIAN_POINT('Ctrl Pts',(4.6673347043654,-0.990849724384406,-2.078454563915));
#20079=CARTESIAN_POINT('Ctrl Pts',(3.32588978545028,-1.48597236284793,-2.15745439976257));
#20080=CARTESIAN_POINT('Ctrl Pts',(2.17825101293718,-0.633009206833395,
-2.23645423561013));
#20081=CARTESIAN_POINT('Ctrl Pts',(2.26556529167371,0.79422487141697,-2.31545407145769));
#20082=CARTESIAN_POINT('Ctrl Pts',(3.50862042243917,1.50093191073172,-2.39445390730526));
#20083=CARTESIAN_POINT('Ctrl Pts',(4.77970703110856,0.84598173644438,-2.47345374315282));
#20084=CARTESIAN_POINT('Ctrl Pts',(4.92568536669948,-0.576449711125441,
-2.55245357900038));
#20085=CARTESIAN_POINT('Ctrl Pts',(3.81412273705863,-1.47592145493228,-2.63145341484794));
#20086=CARTESIAN_POINT('Ctrl Pts',(2.4534374869252,-1.03642566702533,-2.71045325069551));
#20087=CARTESIAN_POINT('Ctrl Pts',(2.07805395827079,0.343323623218521,-2.78945308654307));
#20088=CARTESIAN_POINT('Ctrl Pts',(3.02852303551155,1.4116070269678,-2.86845292239064));
#20089=CARTESIAN_POINT('Ctrl Pts',(4.44257170942605,1.1992694530034,-2.9474527582382));
#20090=CARTESIAN_POINT('Ctrl Pts',(5.03736392102105,-0.101054784462667,
-3.02645259408576));
#20091=CARTESIAN_POINT('Ctrl Pts',(4.27329950608871,-1.30970132806027,-3.10545242993333));
#20092=CARTESIAN_POINT('Ctrl Pts',(2.84354370069912,-1.33017654407844,-3.18445226578088));
#20093=CARTESIAN_POINT('Ctrl Pts',(2.04518219683984,-0.143905155790045,
-3.26345210162845));
#20094=CARTESIAN_POINT('Ctrl Pts',(2.60249481892977,1.17291811966321,-3.34245193747601));
#20095=CARTESIAN_POINT('Ctrl Pts',(4.00988318062076,1.42566086811101,-3.42145177332358));
#20096=CARTESIAN_POINT('Ctrl Pts',(4.99055351046055,0.385032883820701,-3.50045160917113));
#20097=CARTESIAN_POINT('Ctrl Pts',(4.65483398575262,-1.00489995565251,-3.5794514450187));
#20098=CARTESIAN_POINT('Ctrl Pts',(3.30729199512237,-1.48317966565961,-3.65845128086626));
#20099=CARTESIAN_POINT('Ctrl Pts',(2.1704282123283,-0.615907138199342,-3.73745111671383));
#20100=CARTESIAN_POINT('Ctrl Pts',(2.27561438689736,0.810121180662424,-3.81645095256139));
#20101=CARTESIAN_POINT('Ctrl Pts',(3.52742479541991,1.50120120398156,-3.89545078840895));
#20102=CARTESIAN_POINT('Ctrl Pts',(4.79020720703601,0.830379708776461,-3.97445062425652));
#20103=CARTESIAN_POINT('Ctrl Pts',(4.91835550353555,-0.59376877773063,-4.05345046010407));
#20104=CARTESIAN_POINT('Ctrl Pts',(3.79561254421272,-1.47924556726675,-4.13245029595163));
#20105=CARTESIAN_POINT('Ctrl Pts',(2.44053955667557,-1.02273916428501,-4.21145013179919));
#20106=CARTESIAN_POINT('Ctrl Pts',(2.08246939420409,0.361604238293931,-4.29044996764677));
#20107=CARTESIAN_POINT('Ctrl Pts',(3.04624611948272,1.41789743685548,-4.36944980349431));
#20108=CARTESIAN_POINT('Ctrl Pts',(4.45752392050836,1.18786294846641,-4.4484496393419));
#20109=CARTESIAN_POINT('Ctrl Pts',(5.03598049592748,-0.11981013295363,-4.52744947518944));
#20110=CARTESIAN_POINT('Ctrl Pts',(4.25683549892569,-1.31879052110152,-4.60644931103702));
#20111=CARTESIAN_POINT('Ctrl Pts',(2.82693538802763,-1.32135379438171,-4.68544914688457));
#20112=CARTESIAN_POINT('Ctrl Pts',(2.04349677031109,-0.125174531149584,
-4.76444898273215));
#20113=CARTESIAN_POINT('Ctrl Pts',(2.61726131072331,1.18456404951518,-4.84344881857968));
#20114=CARTESIAN_POINT('Ctrl Pts',(4.02770531344641,1.41965682417793,-4.92244865442727));
#20115=CARTESIAN_POINT('Ctrl Pts',(4.99526290549326,0.366825781897791,-5.00144849027483));
#20116=CARTESIAN_POINT('Ctrl Pts',(4.64215824284418,-1.0187924897527,-5.08044832612239));
#20117=CARTESIAN_POINT('Ctrl Pts',(3.28873064775948,-1.48015421592793,-5.15944816196995));
#20118=CARTESIAN_POINT('Ctrl Pts',(2.1628202605679,-0.598708416385872,-5.23844799781751));
#20119=CARTESIAN_POINT('Ctrl Pts',(2.28586182430827,0.825890359097424,-5.31744783366508));
#20120=CARTESIAN_POINT('Ctrl Pts',(3.54623106632798,1.50123491655445,-5.39644766951263));
#20121=CARTESIAN_POINT('Ctrl Pts',(4.80051111482114,0.814647371176435,-5.47544750536019));
#20122=CARTESIAN_POINT('Ctrl Pts',(4.91080926215673,-0.610994665314678,
-5.55444734120777));
#20123=CARTESIAN_POINT('Ctrl Pts',(3.77706216309608,-1.4823375443742,-5.63344717705533));
#20124=CARTESIAN_POINT('Ctrl Pts',(2.42781408721338,-1.00889216500817,-5.71244701290288));
#20125=CARTESIAN_POINT('Ctrl Pts',(2.08711348220302,0.37982810749517,-5.79144684875045));
#20126=CARTESIAN_POINT('Ctrl Pts',(3.06404661184834,1.42396533876201,-5.87044668459801));
#20127=CARTESIAN_POINT('Ctrl Pts',(4.47233207081086,1.17627003482815,-5.94944652044556));
#20128=CARTESIAN_POINT('Ctrl Pts',(5.03436223395028,-0.138546679865455,
-6.02844635629314));
#20129=CARTESIAN_POINT('Ctrl Pts',(4.24025892463984,-1.32767275882361,-6.1074461921407));
#20130=CARTESIAN_POINT('Ctrl Pts',(2.81043889977172,-1.31232368711613,-6.18644602798827));
#20131=CARTESIAN_POINT('Ctrl Pts',(2.04204611174854,-0.106424263105081,
-6.26544586383582));
#20132=CARTESIAN_POINT('Ctrl Pts',(2.63217253069154,1.19602408795599,-6.34444569968339));
#20133=CARTESIAN_POINT('Ctrl Pts',(4.04545083611885,1.41342999616619,-6.42344553553094));
#20134=CARTESIAN_POINT('Ctrl Pts',(4.99974385337733,0.348561114693986,-6.5024453713785));
#20135=CARTESIAN_POINT('Ctrl Pts',(4.62930946483854,-1.03252514666121,-6.58144520722607));
#20136=CARTESIAN_POINT('Ctrl Pts',(3.2702086561495,-1.47689648837554,-6.66044504307363));
#20137=CARTESIAN_POINT('Ctrl Pts',(2.15542835156255,-0.581415740385269,
-6.7394448789212));
#20138=CARTESIAN_POINT('Ctrl Pts',(2.29630599579274,0.84152993210976,-6.81844471476877));
#20139=CARTESIAN_POINT('Ctrl Pts',(3.56503628393201,1.50103304315188,-6.89744455061633));
#20140=CARTESIAN_POINT('Ctrl Pts',(4.8106171374903,0.798787192494724,-6.97644438646388));
#20141=CARTESIAN_POINT('Ctrl Pts',(4.90304782678089,-0.62812467065362,-7.05544422231144));
#20142=CARTESIAN_POINT('Ctrl Pts',(3.75847450478497,-1.48519690103531,-7.134444058159));
#20143=CARTESIAN_POINT('Ctrl Pts',(2.4152630755228,-0.994886842179035,-7.21344389400658));
#20144=CARTESIAN_POINT('Ctrl Pts',(2.0919854934795,0.397992370984998,-7.29244372985414));
#20145=CARTESIAN_POINT('Ctrl Pts',(3.08192171921059,1.42980978046278,-7.3714435657017));
#20146=CARTESIAN_POINT('Ctrl Pts',(4.48699383651834,1.16449253134292,-7.45044340154927));
#20147=CARTESIAN_POINT('Ctrl Pts',(5.03250938904027,-0.157261484907092,
-7.5294432373968));
#20148=CARTESIAN_POINT('Ctrl Pts',(4.22357238456189,-1.33634664735353,-7.60844307324441));
#20149=CARTESIAN_POINT('Ctrl Pts',(2.79405682469425,-1.30308763935961,-7.68744290909193));
#20150=CARTESIAN_POINT('Ctrl Pts',(2.04083044880146,-0.087657294100584,
-7.76644274493952));
#20151=CARTESIAN_POINT('Ctrl Pts',(2.64722613884448,1.20729643658276,-7.84544258078706));
#20152=CARTESIAN_POINT('Ctrl Pts',(4.06311696386691,1.40698136124133,-7.92444241663464));
#20153=CARTESIAN_POINT('Ctrl Pts',(5.00399565092529,0.330241748447076,-8.00344225248219));
#20154=CARTESIAN_POINT('Ctrl Pts',(4.61628966807169,-1.04609577133396,-8.08244208832976));
#20155=CARTESIAN_POINT('Ctrl Pts',(3.25172892691107,-1.47340699423921,-8.16144192417732));
#20156=CARTESIAN_POINT('Ctrl Pts',(2.14825364531581,-0.564031823890016,
-8.24044176002488));
#20157=CARTESIAN_POINT('Ctrl Pts',(2.3069452623567,0.857037445382742,-8.31944159587245));
#20158=CARTESIAN_POINT('Ctrl Pts',(3.58383749718331,1.50059561550652,-8.39844143172001));
#20159=CARTESIAN_POINT('Ctrl Pts',(4.82052368908861,0.782801661538469,-8.47744126756757));
#20160=CARTESIAN_POINT('Ctrl Pts',(4.89507241546346,-0.645156105375968,
-8.55644110341514));
#20161=CARTESIAN_POINT('Ctrl Pts',(3.73985248607643,-1.48782318890163,-8.6354409392627));
#20162=CARTESIAN_POINT('Ctrl Pts',(2.40288849145644,-0.980725392932309,
-8.71444077511025));
#20163=CARTESIAN_POINT('Ctrl Pts',(2.09708466301015,0.416094176959081,-8.79344061095783));
#20164=CARTESIAN_POINT('Ctrl Pts',(3.09986863735219,1.43542984731223,-8.87244044680538));
#20165=CARTESIAN_POINT('Ctrl Pts',(4.50150691509507,1.15253228145486,-8.95144028265294));
#20166=CARTESIAN_POINT('Ctrl Pts',(5.03042225517976,-0.17595160211279,-9.0304401185005));
#20167=CARTESIAN_POINT('Ctrl Pts',(4.20677849115691,-1.34481084279703,-9.10943995434808));
#20168=CARTESIAN_POINT('Ctrl Pts',(2.77779174524815,-1.29364706763578,-9.18843979019563));
#20169=CARTESIAN_POINT('Ctrl Pts',(2.03984995009324,-0.0688766317242347,
-9.2674396260432));
#20170=CARTESIAN_POINT('Ctrl Pts',(2.66241981497398,1.21837944536639,-9.34643946189075));
#20171=CARTESIAN_POINT('Ctrl Pts',(4.08070084425368,1.40031170518944,-9.42543929773831));
#20172=CARTESIAN_POINT('Ctrl Pts',(5.00801778330857,0.311870988189331,-9.50443913358589));
#20173=CARTESIAN_POINT('Ctrl Pts',(4.60310060585307,-1.05950305241988,-9.58343896943344));
#20174=CARTESIAN_POINT('Ctrl Pts',(3.233294911356,-1.46968472477563,-9.662438805281));
#20175=CARTESIAN_POINT('Ctrl Pts',(2.1412962191189,-0.546562355108196,-9.74143864112856));
#20176=CARTESIAN_POINT('Ctrl Pts',(2.31777994889124,0.872416095653864,-9.82043847697613));
#20177=CARTESIAN_POINT('Ctrl Pts',(3.6026279620964,1.49991199335744,-9.89943831282369));
#20178=CARTESIAN_POINT('Ctrl Pts',(4.83023643037598,0.766713655392416,-9.97843814867126));
#20179=CARTESIAN_POINT('Ctrl Pts',(4.88687055597945,-0.662125038269567,
-10.0574379845188));
#20180=CARTESIAN_POINT('Ctrl Pts',(3.72122513262798,-1.49014230591843,-10.1364378203663));
#20181=CARTESIAN_POINT('Ctrl Pts',(2.39064262354056,-0.966550225602336,
-10.2154376562139));
#20182=CARTESIAN_POINT('Ctrl Pts',(2.10250467091252,0.434397551406489,-10.2944374920615));
#20183=CARTESIAN_POINT('Ctrl Pts',(3.11770451236289,1.44031508778373,-10.373437327909));
#20184=CARTESIAN_POINT('Ctrl Pts',(4.51621434152236,1.14137741925843,-10.4524371637566));
#20185=CARTESIAN_POINT('Ctrl Pts',(5.02741926695713,-0.196635563676407,
-10.5314369996042));
#20186=CARTESIAN_POINT('Ctrl Pts',(4.47009889505261,-0.964259040168617,
-10.5841035568359));
#20187=CARTESIAN_POINT('Ctrl Pts',(4.09066022205677,-1.14663922575821,-10.6104368354517));
#20188=CARTESIAN_POINT('Ctrl Pts',(4.22276258896322,0.956786087600807,-0.00116693790158886));
#20189=CARTESIAN_POINT('Ctrl Pts',(4.53945734382533,0.730642322779539,-0.0275065074384037));
#20190=CARTESIAN_POINT('Ctrl Pts',(4.92538271480697,-0.0566428170878688,
-0.0801793555910728));
#20191=CARTESIAN_POINT('Ctrl Pts',(4.24789474461888,-1.19392078423981,-0.159185482359595));
#20192=CARTESIAN_POINT('Ctrl Pts',(2.92726025435682,-1.24449194312104,-0.238185318207158));
#20193=CARTESIAN_POINT('Ctrl Pts',(2.16236448555846,-0.167798961195079,
-0.317185154054721));
#20194=CARTESIAN_POINT('Ctrl Pts',(2.64668019390599,1.06203237714166,-0.396184989902284));
#20195=CARTESIAN_POINT('Ctrl Pts',(3.94106727267031,1.32790237413237,-0.475184825749846));
#20196=CARTESIAN_POINT('Ctrl Pts',(4.87112409072546,0.389339689978404,-0.554184661597408));
#20197=CARTESIAN_POINT('Ctrl Pts',(4.59316073831506,-0.902566851583658,
-0.633184497444971));
#20198=CARTESIAN_POINT('Ctrl Pts',(3.35931360943555,-1.37558834803353,-0.712184333292533));
#20199=CARTESIAN_POINT('Ctrl Pts',(2.28895645692331,-0.600701735828637,
-0.791184169140097));
#20200=CARTESIAN_POINT('Ctrl Pts',(2.35311625561809,0.719165366393499,-0.870184004987657));
#20201=CARTESIAN_POINT('Ctrl Pts',(3.49359169428227,1.38658992886142,-0.949183840835221));
#20202=CARTESIAN_POINT('Ctrl Pts',(4.67573189207826,0.796094517421205,-1.02818367668278));
#20203=CARTESIAN_POINT('Ctrl Pts',(4.82709135188776,-0.516626874956721,
-1.10718351253034));
#20204=CARTESIAN_POINT('Ctrl Pts',(3.81035486229653,-1.36065884628765,-1.18618334837791));
#20205=CARTESIAN_POINT('Ctrl Pts',(2.54791412842535,-0.970291199099466,
-1.26518318422547));
#20206=CARTESIAN_POINT('Ctrl Pts',(2.1850650964183,0.300332646552455,-1.34418302007303));
#20207=CARTESIAN_POINT('Ctrl Pts',(3.05098736172375,1.29849214451639,-1.42318285592059));
#20208=CARTESIAN_POINT('Ctrl Pts',(4.36010939160367,1.11864948607607,-1.50218269176816));
#20209=CARTESIAN_POINT('Ctrl Pts',(4.92478543130558,-0.0760408277145407,
-1.58118252761572));
#20210=CARTESIAN_POINT('Ctrl Pts',(4.23273692898091,-1.20174627466853,-1.66018236346328));
#20211=CARTESIAN_POINT('Ctrl Pts',(2.91179572737664,-1.2372180823164,-1.73918219931084));
#20212=CARTESIAN_POINT('Ctrl Pts',(2.16033005138785,-0.15027592345917,-1.81818203515841));
#20213=CARTESIAN_POINT('Ctrl Pts',(2.6600754644131,1.072997728517,-1.89718187100597));
#20214=CARTESIAN_POINT('Ctrl Pts',(3.95765900297715,1.32283941919587,-1.97618170685353));
#20215=CARTESIAN_POINT('Ctrl Pts',(4.87590269388304,0.372590801624887,-2.0551815427011));
#20216=CARTESIAN_POINT('Ctrl Pts',(4.5817686510791,-0.915675115822265,-2.13418137854866));
#20217=CARTESIAN_POINT('Ctrl Pts',(3.34209758767953,-1.37323337936518,-2.21318121439622));
#20218=CARTESIAN_POINT('Ctrl Pts',(2.28152882525099,-0.584983539399816,
-2.29218105024378));
#20219=CARTESIAN_POINT('Ctrl Pts',(2.36221867188204,0.733967960252988,-2.37118088609134));
#20220=CARTESIAN_POINT('Ctrl Pts',(3.51096466517007,1.38705796386476,-2.45018072193891));
#20221=CARTESIAN_POINT('Ctrl Pts',(4.68561542095099,0.781798092524566,-2.52918055778647));
#20222=CARTESIAN_POINT('Ctrl Pts',(4.82051855112322,-0.532715146414797,
-2.60818039363403));
#20223=CARTESIAN_POINT('Ctrl Pts',(3.79328887684296,-1.3639450220661,-2.6871802294816));
#20224=CARTESIAN_POINT('Ctrl Pts',(2.5358372236292,-0.957793265052575,-2.76618006532916));
#20225=CARTESIAN_POINT('Ctrl Pts',(2.18893360381748,0.317276061867459,-2.84517990117672));
#20226=CARTESIAN_POINT('Ctrl Pts',(3.06729170491967,1.30451005445585,-2.92417973702428));
#20227=CARTESIAN_POINT('Ctrl Pts',(4.3740581614269,1.10828228363614,-3.00317957287185));
#20228=CARTESIAN_POINT('Ctrl Pts',(4.92372418427492,-0.093387876274314,
-3.0821794087194));
#20229=CARTESIAN_POINT('Ctrl Pts',(4.21762844198311,-1.21033582161941,-3.16117924456697));
#20230=CARTESIAN_POINT('Ctrl Pts',(2.89634653567684,-1.22925760696942,-3.24017908041453));
#20231=CARTESIAN_POINT('Ctrl Pts',(2.15855578444204,-0.132987240095699,
-3.31917891626209));
#20232=CARTESIAN_POINT('Ctrl Pts',(2.6735857503619,1.08393019510593,-3.39817875210966));
#20233=CARTESIAN_POINT('Ctrl Pts',(3.97419720473653,1.31749764712491,-3.47717858795722));
#20234=CARTESIAN_POINT('Ctrl Pts',(4.88046522476084,0.355820889698422,-3.55617842380478));
#20235=CARTESIAN_POINT('Ctrl Pts',(4.57021634735239,-0.928659372493224,
-3.63517825965234));
#20236=CARTESIAN_POINT('Ctrl Pts',(3.32491078993065,-1.37065256084301,-3.71417809549991));
#20237=CARTESIAN_POINT('Ctrl Pts',(2.27429953136583,-0.569178984690962,
-3.79317793134746));
#20238=CARTESIAN_POINT('Ctrl Pts',(2.37150535401595,0.748658235126427,-3.87217776719504));
#20239=CARTESIAN_POINT('Ctrl Pts',(3.52834237238777,1.38730682615101,-3.95117760304259));
#20240=CARTESIAN_POINT('Ctrl Pts',(4.6953189608238,0.767379772429904,-4.03017743889016));
#20241=CARTESIAN_POINT('Ctrl Pts',(4.81374479609618,-0.548720235712767,
-4.10917727473772));
#20242=CARTESIAN_POINT('Ctrl Pts',(3.77618303065766,-1.36701693788942,-4.18817711058528));
#20243=CARTESIAN_POINT('Ctrl Pts',(2.52391784424749,-0.94514514125183,-4.26717694643284));
#20244=CARTESIAN_POINT('Ctrl Pts',(2.19301404579585,0.334169748078935,-4.34617678228041));
#20245=CARTESIAN_POINT('Ctrl Pts',(3.08367015925906,1.31032321830978,-4.42517661812797));
#20246=CARTESIAN_POINT('Ctrl Pts',(4.38787596575953,1.09774117724432,-4.50417645397553));
#20247=CARTESIAN_POINT('Ctrl Pts',(4.92244571802357,-0.110720278432897,
-4.58317628982309));
#20248=CARTESIAN_POINT('Ctrl Pts',(4.20241353976848,-1.21873542822569,-4.66217612567066));
#20249=CARTESIAN_POINT('Ctrl Pts',(2.88099827624373,-1.22110422896304,-4.74117596151822));
#20250=CARTESIAN_POINT('Ctrl Pts',(2.15699822925082,-0.115677686018026,
-4.82017579736578));
#20251=CARTESIAN_POINT('Ctrl Pts',(2.68723192571078,1.09469256189437,-4.89917563321335));
#20252=CARTESIAN_POINT('Ctrl Pts',(3.99066719320976,1.31194912297586,-4.9781754690609));
#20253=CARTESIAN_POINT('Ctrl Pts',(4.88481732350589,0.33899513928263,-5.05717530490847));
#20254=CARTESIAN_POINT('Ctrl Pts',(4.55850229821843,-0.94149789629576,-5.13617514075603));
#20255=CARTESIAN_POINT('Ctrl Pts',(3.30775767026166,-1.36785664844046,-5.2151749766036));
#20256=CARTESIAN_POINT('Ctrl Pts',(2.26726878599858,-0.553285109766257,
-5.29417481245115));
#20257=CARTESIAN_POINT('Ctrl Pts',(2.38097533034757,0.763231024455163,-5.37317464829872));
#20258=CARTESIAN_POINT('Ctrl Pts',(3.5457218335393,1.38733798099046,-5.45217448414627));
#20259=CARTESIAN_POINT('Ctrl Pts',(4.70484112318846,0.752841028865123,-5.53117431999385));
#20260=CARTESIAN_POINT('Ctrl Pts',(4.80677107921609,-0.564639215372841,
-5.6101741558414));
#20261=CARTESIAN_POINT('Ctrl Pts',(3.75904004523867,-1.36987433031362,-5.68917399168897));
#20262=CARTESIAN_POINT('Ctrl Pts',(2.5121578412552,-0.932348697598894,-5.76817382753653));
#20263=CARTESIAN_POINT('Ctrl Pts',(2.19730579227532,0.351010993659279,-5.84717366338409));
#20264=CARTESIAN_POINT('Ctrl Pts',(3.10012014910864,1.3159307556026,-5.92617349923167));
#20265=CARTESIAN_POINT('Ctrl Pts',(4.40156063903508,1.08702780439152,-6.00517333507921));
#20266=CARTESIAN_POINT('Ctrl Pts',(4.92095023168801,-0.128035305466137,
-6.08417317092679));
#20267=CARTESIAN_POINT('Ctrl Pts',(4.18709461076685,-1.22694378097059,-6.16317300677434));
#20268=CARTESIAN_POINT('Ctrl Pts',(2.86575335723871,-1.21275922536378,-6.24217284262192));
#20269=CARTESIAN_POINT('Ctrl Pts',(2.15565763045507,-0.0983499788583807,
-6.32117267846946));
#20270=CARTESIAN_POINT('Ctrl Pts',(2.70101184887717,1.1052831406354,-6.40017251431704));
#20271=CARTESIAN_POINT('Ctrl Pts',(4.00706638385242,1.30619471711537,-6.47917235016458));
#20272=CARTESIAN_POINT('Ctrl Pts',(4.88895830712003,0.322116190996409,-6.55817218601216));
#20273=CARTESIAN_POINT('Ctrl Pts',(4.5466283419575,-0.954188672601991,-6.63717202185972));
#20274=CARTESIAN_POINT('Ctrl Pts',(3.29064092047072,-1.36484608086353,-6.71617185770728));
#20275=CARTESIAN_POINT('Ctrl Pts',(2.26043769247546,-0.537304408848601,
-6.79517169355484));
#20276=CARTESIAN_POINT('Ctrl Pts',(2.39062711476892,0.777684041372917,-6.87417152940241));
#20277=CARTESIAN_POINT('Ctrl Pts',(3.56310032129972,1.3871514234866,-6.95317136524997));
#20278=CARTESIAN_POINT('Ctrl Pts',(4.71418041374923,0.738184143371853,-7.03217120109753));
#20279=CARTESIAN_POINT('Ctrl Pts',(4.79959849485559,-0.580469587261487,
-7.11117103694509));
#20280=CARTESIAN_POINT('Ctrl Pts',(3.74186261080232,-1.37251675093242,-7.19017087279266));
#20281=CARTESIAN_POINT('Ctrl Pts',(2.50055906012761,-0.91940594221622,-7.26917070864021));
#20282=CARTESIAN_POINT('Ctrl Pts',(2.20180816976011,0.367797155743754,-7.34817054448779));
#20283=CARTESIAN_POINT('Ctrl Pts',(3.1166390930024,1.32133178635383,-7.42717038033534));
#20284=CARTESIAN_POINT('Ctrl Pts',(4.41511003374343,1.07614384630731,-7.50617021618291));
#20285=CARTESIAN_POINT('Ctrl Pts',(4.91923795995212,-0.145330240159424,
-7.58517005203047));
#20286=CARTESIAN_POINT('Ctrl Pts',(4.17167405894901,-1.23495959173261,-7.66416988787803));
#20287=CARTESIAN_POINT('Ctrl Pts',(2.85061417101823,-1.20422390573755,-7.74316972372559));
#20288=CARTESIAN_POINT('Ctrl Pts',(2.15453419843256,-0.0810068378210246,
-7.82216955957316));
#20289=CARTESIAN_POINT('Ctrl Pts',(2.7149233574034,1.11570026936884,-7.90116939542071));
#20290=CARTESIAN_POINT('Ctrl Pts',(4.02339220317067,1.30023533257259,-7.98016923126829));
#20291=CARTESIAN_POINT('Ctrl Pts',(4.89288752576577,0.305186693619449,-8.05916906711584));
#20292=CARTESIAN_POINT('Ctrl Pts',(4.53459634192857,-0.966729709868482,
-8.1381689029634));
#20293=CARTESIAN_POINT('Ctrl Pts',(3.27356322665466,-1.36162133056204,-8.21716873881097));
#20294=CARTESIAN_POINT('Ctrl Pts',(2.25380732279195,-0.521239389745805,
-8.29616857465853));
#20295=CARTESIAN_POINT('Ctrl Pts',(2.40045919263447,0.792015017769138,-8.37516841050609));
#20296=CARTESIAN_POINT('Ctrl Pts',(3.58047510851297,1.38674718296458,-8.45416824635366));
#20297=CARTESIAN_POINT('Ctrl Pts',(4.72333536687576,0.723411415934357,-8.53316808220121));
#20298=CARTESIAN_POINT('Ctrl Pts',(4.7922281686577,-0.596208866970824,-8.61216791804879));
#20299=CARTESIAN_POINT('Ctrl Pts',(3.72465342285165,-1.37494378541303,-8.69116775389634));
#20300=CARTESIAN_POINT('Ctrl Pts',(2.48912332126697,-0.906318905544476,
-8.77016758974391));
#20301=CARTESIAN_POINT('Ctrl Pts',(2.20652047126826,0.384525598891084,-8.84916742559147));
#20302=CARTESIAN_POINT('Ctrl Pts',(3.13322439947578,1.32652546531105,-8.92816726143904));
#20303=CARTESIAN_POINT('Ctrl Pts',(4.42852202203957,1.06509100657593,-9.00716709728659));
#20304=CARTESIAN_POINT('Ctrl Pts',(4.91730917449412,-0.162602360053987,
-9.08616693313416));
#20305=CARTESIAN_POINT('Ctrl Pts',(4.15615429857538,-1.24278161857717,-9.16516676898172));
#20306=CARTESIAN_POINT('Ctrl Pts',(2.83558310410754,-1.19549957913796,-9.24416660482928));
#20307=CARTESIAN_POINT('Ctrl Pts',(2.15362808901342,-0.0636510423119035,
-9.32316644067685));
#20308=CARTESIAN_POINT('Ctrl Pts',(2.72896430711279,1.12594242325137,-9.4021662765244));
#20309=CARTESIAN_POINT('Ctrl Pts',(4.03964201513864,1.29407169551693,-9.48116611237197));
#20310=CARTESIAN_POINT('Ctrl Pts',(4.896604503674,0.288209701435084,-9.56016594821952));
#20311=CARTESIAN_POINT('Ctrl Pts',(4.52240791841949,-0.979119796234855,
-9.6391657840671));
#20312=CARTESIAN_POINT('Ctrl Pts',(3.25652777827833,-1.35818146532484,-9.71816561991465));
#20313=CARTESIAN_POINT('Ctrl Pts',(2.24737774837526,-0.505095309108265,
-9.79716545576223));
#20314=CARTESIAN_POINT('Ctrl Pts',(2.41047186418625,0.806226907848581,-9.87616529160978));
#20315=CARTESIAN_POINT('Ctrl Pts',(3.59783996285183,1.38611542642761,-9.95516512745734));
#20316=CARTESIAN_POINT('Ctrl Pts',(4.73231121385275,0.708543987979741,-10.0341649633049));
#20317=CARTESIAN_POINT('Ctrl Pts',(4.78464857465049,-0.611890386791985,
-10.1131647991525));
#20318=CARTESIAN_POINT('Ctrl Pts',(3.70743930490157,-1.37708695373684,-10.1921646350001));
#20319=CARTESIAN_POINT('Ctrl Pts',(2.47780653301313,-0.8932191915644,-10.2711644708476));
#20320=CARTESIAN_POINT('Ctrl Pts',(2.21152926951652,0.401440317747649,-10.3501643066952));
#20321=CARTESIAN_POINT('Ctrl Pts',(3.14970708753058,1.33104006830733,-10.4291641425427));
#20322=CARTESIAN_POINT('Ctrl Pts',(4.44211361324239,1.05478245071491,-10.5081639783903));
#20323=CARTESIAN_POINT('Ctrl Pts',(4.91453401947221,-0.181717053669302,
-10.5871638142379));
#20324=CARTESIAN_POINT('Ctrl Pts',(4.39949689170713,-0.891101835687162,
-10.6398303714696));
#20325=CARTESIAN_POINT('Ctrl Pts',(4.04884578660764,-1.05964505011576,-10.6661636500854));
#20326=CARTESIAN_POINT('',(4.22506707917393,0.958749515186979,-10.500517058265));
#20327=CARTESIAN_POINT('Ctrl Pts',(4.22563688151301,0.959452996237738,-10.5));
#20328=CARTESIAN_POINT('Ctrl Pts',(4.2562168906156,0.942844384233757,-10.5));
#20329=CARTESIAN_POINT('Ctrl Pts',(4.28592702146003,0.924851671966296,-10.5));
#20330=CARTESIAN_POINT('Ctrl Pts',(4.31466131642553,0.90550344967816,-10.5));
#20331=CARTESIAN_POINT('Ctrl Pts',(4.35457535570847,0.878627352478251,-10.5));
#20332=CARTESIAN_POINT('Ctrl Pts',(4.39260790499763,0.849138177160262,-10.5));
#20333=CARTESIAN_POINT('Ctrl Pts',(4.42869685663605,0.817341922666849,-10.5));
#20334=CARTESIAN_POINT('Ctrl Pts',(4.46599521848368,0.784480114505271,-10.5));
#20335=CARTESIAN_POINT('Ctrl Pts',(4.50121824244792,0.74915350101323,-10.5));
#20336=CARTESIAN_POINT('Ctrl Pts',(4.53427434865288,0.71164930909598,-10.5));
#20337=CARTESIAN_POINT('Ctrl Pts',(4.54834774946247,0.695682167605729,-10.5));
#20338=CARTESIAN_POINT('Ctrl Pts',(4.56202803905104,0.679319759554166,-10.5));
#20339=CARTESIAN_POINT('Ctrl Pts',(4.57530644205088,0.66258198317025,-10.5));
#20340=CARTESIAN_POINT('Ctrl Pts',(4.58155620710802,0.654703989861894,-10.5));
#20341=CARTESIAN_POINT('Ctrl Pts',(4.58771180447156,0.646749202455899,-10.5));
#20342=CARTESIAN_POINT('Ctrl Pts',(4.59376918906261,0.638724849112881,-10.5));
#20343=CARTESIAN_POINT('Ctrl Pts',(4.62474005444643,0.597697048509672,-10.5));
#20344=CARTESIAN_POINT('Ctrl Pts',(4.65317519747177,0.554817087484474,-10.5));
#20345=CARTESIAN_POINT('Ctrl Pts',(4.67900095039148,0.5104163567665,-10.5));
#20346=CARTESIAN_POINT('Ctrl Pts',(4.7054689829035,0.464911391708797,-10.5));
#20347=CARTESIAN_POINT('Ctrl Pts',(4.7291969971767,0.41780829539787,-10.5));
#20348=CARTESIAN_POINT('Ctrl Pts',(4.75007397342937,0.369418834636001,-10.5));
#20349=CARTESIAN_POINT('Ctrl Pts',(4.76945845021146,0.324488746711177,-10.5));
#20350=CARTESIAN_POINT('Ctrl Pts',(4.78638508274871,0.278448543884407,-10.5));
#20351=CARTESIAN_POINT('Ctrl Pts',(4.80073253596587,0.231524038388971,-10.5));
#20352=CARTESIAN_POINT('Ctrl Pts',(4.8036207521087,0.222077894030463,-10.5));
#20353=CARTESIAN_POINT('Ctrl Pts',(4.80640169864761,0.212604391535165,-10.5));
#20354=CARTESIAN_POINT('Ctrl Pts',(4.80907390505575,0.20310887732277,-10.5));
#20355=CARTESIAN_POINT('Ctrl Pts',(4.82382063804542,0.150707306746792,-10.5));
#20356=CARTESIAN_POINT('Ctrl Pts',(4.83526858041764,0.097606612097567,-10.5));
#20357=CARTESIAN_POINT('Ctrl Pts',(4.84331427811994,0.0441419444719137,
-10.5));
#20358=CARTESIAN_POINT('Ctrl Pts',(4.85127241447955,-0.00874086707904043,
-10.5));
#20359=CARTESIAN_POINT('Ctrl Pts',(4.85590253247874,-0.06198087933818,-10.5));
#20360=CARTESIAN_POINT('Ctrl Pts',(4.85706162899042,-0.115279789094187,
-10.5));
#20361=CARTESIAN_POINT('Ctrl Pts',(4.85747724957996,-0.134391333363179,
-10.5));
#20362=CARTESIAN_POINT('Ctrl Pts',(4.85744613961991,-0.153510615472189,
-10.5));
#20363=CARTESIAN_POINT('Ctrl Pts',(4.85696012143623,-0.172624292325265,
-10.5));
#20364=CARTESIAN_POINT('Ctrl Pts',(4.85648938188235,-0.191137105254633,
-10.5));
#20365=CARTESIAN_POINT('Ctrl Pts',(4.85559188252653,-0.209644665520278,
-10.5));
#20366=CARTESIAN_POINT('Ctrl Pts',(4.85427508835799,-0.228137575142134,
-10.5));
#20367=CARTESIAN_POINT('Ctrl Pts',(4.85337448116019,-0.240785601623099,
-10.5));
#20368=CARTESIAN_POINT('Ctrl Pts',(4.85227772223906,-0.253426776185862,
-10.5));
#20369=CARTESIAN_POINT('Ctrl Pts',(4.85098698538755,-0.266058091305494,
-10.5));
#20370=CARTESIAN_POINT('Ctrl Pts',(4.84998324704724,-0.275880802464079,
-10.5));
#20371=CARTESIAN_POINT('Ctrl Pts',(4.84886269296499,-0.285692120985615,
-10.5));
#20372=CARTESIAN_POINT('Ctrl Pts',(4.84762783302268,-0.295482832018067,
-10.5));
#20373=CARTESIAN_POINT('Ctrl Pts',(4.8409806354647,-0.348185805234636,-10.5));
#20374=CARTESIAN_POINT('Ctrl Pts',(4.83101865061774,-0.400359240847176,
-10.5));
#20375=CARTESIAN_POINT('Ctrl Pts',(4.81798085892437,-0.451779699261908,
-10.5));
#20376=CARTESIAN_POINT('Ctrl Pts',(4.80449726831377,-0.50495836836319,-10.5));
#20377=CARTESIAN_POINT('Ctrl Pts',(4.78772387104494,-0.557332542920654,
-10.5));
#20378=CARTESIAN_POINT('Ctrl Pts',(4.76786911240598,-0.608661600473398,
-10.5));
#20379=CARTESIAN_POINT('Ctrl Pts',(4.75361695127058,-0.645506671847593,
-10.5));
#20380=CARTESIAN_POINT('Ctrl Pts',(4.73777586561183,-0.68181341338085,-10.5));
#20381=CARTESIAN_POINT('Ctrl Pts',(4.72040658847988,-0.717490842063492,
-10.5));
#20382=CARTESIAN_POINT('Ctrl Pts',(4.71341635861835,-0.731849149865565,
-10.5));
#20383=CARTESIAN_POINT('Ctrl Pts',(4.70617846932405,-0.746105493624825,
-10.5));
#20384=CARTESIAN_POINT('Ctrl Pts',(4.69869630293336,-0.760253747426929,
-10.5));
#20385=CARTESIAN_POINT('Ctrl Pts',(4.69367625902796,-0.769746299658832,
-10.5));
#20386=CARTESIAN_POINT('Ctrl Pts',(4.68854632090072,-0.779189830422629,
-10.5));
#20387=CARTESIAN_POINT('Ctrl Pts',(4.68331449686019,-0.788570465878601,
-10.5));
#20388=CARTESIAN_POINT('Ctrl Pts',(4.65536785501926,-0.838678660897688,
-10.5));
#20389=CARTESIAN_POINT('Ctrl Pts',(4.62447200580773,-0.887081914965809,
-10.5));
#20390=CARTESIAN_POINT('Ctrl Pts',(4.59084561731805,-0.933519384991513,
-10.5));
#20391=CARTESIAN_POINT('Ctrl Pts',(4.5630360211261,-0.971923963883094,-10.5));
#20392=CARTESIAN_POINT('Ctrl Pts',(4.53335770980376,-1.00898430302673,-10.5));
#20393=CARTESIAN_POINT('Ctrl Pts',(4.50190865869827,-1.04454497505135,-10.5));
#20394=CARTESIAN_POINT('Ctrl Pts',(4.49326968388208,-1.05431340173732,-10.5));
#20395=CARTESIAN_POINT('Ctrl Pts',(4.48449696594651,-1.06396860188547,-10.5));
#20396=CARTESIAN_POINT('Ctrl Pts',(4.4755922590162,-1.07350719070055,-10.5));
#20397=CARTESIAN_POINT('Ctrl Pts',(4.46697989294738,-1.08273262835935,-10.5));
#20398=CARTESIAN_POINT('Ctrl Pts',(4.45824953647072,-1.09184305726326,-10.5));
#20399=CARTESIAN_POINT('Ctrl Pts',(4.44940666939404,-1.10083236703997,-10.5));
#20400=CARTESIAN_POINT('Ctrl Pts',(4.40811313745869,-1.1428097423779,-10.5));
#20401=CARTESIAN_POINT('Ctrl Pts',(4.36434749913231,-1.18217192728758,-10.5));
#20402=CARTESIAN_POINT('Ctrl Pts',(4.3183086417908,-1.21863823117122,-10.5));
#20403=CARTESIAN_POINT('Ctrl Pts',(4.27226978444943,-1.25510453505477,-10.5));
#20404=CARTESIAN_POINT('Ctrl Pts',(4.22395717313442,-1.28867608466361,-10.5));
#20405=CARTESIAN_POINT('Ctrl Pts',(4.1735261449982,-1.31904027763685,-10.5));
#20406=CARTESIAN_POINT('Ctrl Pts',(4.21285985862019,0.966285267670136,-10.5));
#20407=CARTESIAN_POINT('Ctrl Pts',(4.21677432467609,0.963557533091195,-10.500172352755));
#20408=CARTESIAN_POINT('Ctrl Pts',(4.22067221525924,0.960806011697469,-10.50034470551));
#20409=CARTESIAN_POINT('Ctrl Pts',(4.22455324251919,0.95803090668261,-10.500517058265));
#20410=CARTESIAN_POINT('Ctrl Pts',(4.17505875713847,-1.32076734070061,3.60605642568679E-16));
#20411=CARTESIAN_POINT('Ctrl Pts',(4.21175869148079,-1.29893467734339,2.81168414804524E-15));
#20412=CARTESIAN_POINT('Ctrl Pts',(4.24734010600691,-1.27545799450025,1.12858061007627E-15));
#20413=CARTESIAN_POINT('Ctrl Pts',(4.28167883941674,-1.25033821821112,1.58033308661487E-15));
#20414=CARTESIAN_POINT('Ctrl Pts',(4.32789021929204,-1.21653325777111,2.12731127463373E-15));
#20415=CARTESIAN_POINT('Ctrl Pts',(4.37185284323022,-1.17975348759852,2.30323139873742E-15));
#20416=CARTESIAN_POINT('Ctrl Pts',(4.41343554449499,-1.14031584215013,1.65492619608187E-15));
#20417=CARTESIAN_POINT('Ctrl Pts',(4.45548068146681,-1.100439615876,9.99411277230459E-16));
#20418=CARTESIAN_POINT('Ctrl Pts',(4.49509318427713,-1.05784495275133,1.62667307186133E-15));
#20419=CARTESIAN_POINT('Ctrl Pts',(4.53209185513524,-1.01283383283948,1.56125112837913E-15));
#20420=CARTESIAN_POINT('Ctrl Pts',(4.54201219813825,-1.00076513582634,1.54370973826388E-15));
#20421=CARTESIAN_POINT('Ctrl Pts',(4.55174435185581,-0.988522626003564,
1.56237023283978E-15));
#20422=CARTESIAN_POINT('Ctrl Pts',(4.56128420031517,-0.976111976277783,
1.79023462720806E-15));
#20423=CARTESIAN_POINT('Ctrl Pts',(4.56823205005158,-0.967073328568305,
1.9869967211788E-15));
#20424=CARTESIAN_POINT('Ctrl Pts',(4.57507846805373,-0.95794470700848,2.05160167689976E-15));
#20425=CARTESIAN_POINT('Ctrl Pts',(4.58181998349954,-0.948730743276248,
2.21350715534641E-15));
#20426=CARTESIAN_POINT('Ctrl Pts',(4.5878624474001,-0.940472207983901,2.35862408293951E-15));
#20427=CARTESIAN_POINT('Ctrl Pts',(4.59381742463971,-0.932149464021884,
2.4118579661099E-15));
#20428=CARTESIAN_POINT('Ctrl Pts',(4.59968082387781,-0.923769113033705,
2.13024042849952E-15));
#20429=CARTESIAN_POINT('Ctrl Pts',(4.63227995240401,-0.877176321401323,
8.03406007810654E-16));
#20430=CARTESIAN_POINT('Ctrl Pts',(4.66208807399467,-0.828755572706594,
2.02916507695729E-15));
#20431=CARTESIAN_POINT('Ctrl Pts',(4.68897102900036,-0.778810683153279,
1.83880688453542E-15));
#20432=CARTESIAN_POINT('Ctrl Pts',(4.715408739606,-0.729692997394368,1.6516014675121E-15));
#20433=CARTESIAN_POINT('Ctrl Pts',(4.73901760306379,-0.679100122019099,
4.5266924147842E-16));
#20434=CARTESIAN_POINT('Ctrl Pts',(4.75962250001883,-0.627308223650069,
1.29757316003065E-15));
#20435=CARTESIAN_POINT('Ctrl Pts',(4.77786038072504,-0.581465991773642,
2.04541756363981E-15));
#20436=CARTESIAN_POINT('Ctrl Pts',(4.79374431288129,-0.534683755159472,
2.37654961231099E-15));
#20437=CARTESIAN_POINT('Ctrl Pts',(4.80711873651456,-0.487154600398972,
1.58206781009085E-15));
#20438=CARTESIAN_POINT('Ctrl Pts',(4.81112276225609,-0.472925354761761,
1.37998562811125E-15));
#20439=CARTESIAN_POINT('Ctrl Pts',(4.81490302992813,-0.458622862382454,
7.62743180822846E-16));
#20440=CARTESIAN_POINT('Ctrl Pts',(4.81844677957601,-0.444286884642647,
1.01307850997046E-15));
#20441=CARTESIAN_POINT('Ctrl Pts',(4.8314764555538,-0.391576291814387,1.94800769444789E-15));
#20442=CARTESIAN_POINT('Ctrl Pts',(4.84133483345071,-0.338344892022729,
-1.36320875843642E-15));
#20443=CARTESIAN_POINT('Ctrl Pts',(4.84786961538125,-0.284855426792769,
-1.81799020282369E-15));
#20444=CARTESIAN_POINT('Ctrl Pts',(4.85419670205816,-0.23306601952435,-1.58832042192958E-15));
#20445=CARTESIAN_POINT('Ctrl Pts',(4.85740809979461,-0.181033825930539,
-1.15722930975132E-15));
#20446=CARTESIAN_POINT('Ctrl Pts',(4.85731751599618,-0.129002639121944,
-4.16333634234434E-16));
#20447=CARTESIAN_POINT('Ctrl Pts',(4.85727473537566,-0.104429520122545,
-3.46124443849845E-16));
#20448=CARTESIAN_POINT('Ctrl Pts',(4.856494756818,-0.0798567823844845,3.76639887157404E-16));
#20449=CARTESIAN_POINT('Ctrl Pts',(4.85495404695298,-0.0553113446397769,
7.63278329429795E-16));
#20450=CARTESIAN_POINT('Ctrl Pts',(4.85315804114454,-0.0266987227821337,
1.1759601691976E-15));
#20451=CARTESIAN_POINT('Ctrl Pts',(4.85032828424195,0.00187688481085785,
1.38058548014164E-15));
#20452=CARTESIAN_POINT('Ctrl Pts',(4.8464840467839,0.0303705085563297,-4.57966997657877E-16));
#20453=CARTESIAN_POINT('Ctrl Pts',(4.8449279844867,0.0419040972341098,-1.17936797381194E-15));
#20454=CARTESIAN_POINT('Ctrl Pts',(4.84320517044147,0.0534263312481266,
1.71590219105396E-15));
#20455=CARTESIAN_POINT('Ctrl Pts',(4.84132080768837,0.0649121098521592,
1.36002320516582E-15));
#20456=CARTESIAN_POINT('Ctrl Pts',(4.83280402732952,0.116824542031136,-3.53615764954016E-16));
#20457=CARTESIAN_POINT('Ctrl Pts',(4.82097943108821,0.16809263458422,9.08710747336598E-16));
#20458=CARTESIAN_POINT('Ctrl Pts',(4.80603635446104,0.218463194567921,4.16333634234434E-16));
#20459=CARTESIAN_POINT('Ctrl Pts',(4.79103253706761,0.269038501304066,-7.80448982467912E-17));
#20460=CARTESIAN_POINT('Ctrl Pts',(4.77288409654513,0.318709937008753,-1.91585121700684E-16));
#20461=CARTESIAN_POINT('Ctrl Pts',(4.7517374255193,0.367195857426411,-6.52256026967279E-16));
#20462=CARTESIAN_POINT('Ctrl Pts',(4.73115375517605,0.414390907699223,-1.10066221057683E-15));
#20463=CARTESIAN_POINT('Ctrl Pts',(4.70772855633126,0.460463414084556,-1.80544295475632E-15));
#20464=CARTESIAN_POINT('Ctrl Pts',(4.68156583033195,0.50511771381136,-1.94289029309402E-16));
#20465=CARTESIAN_POINT('Ctrl Pts',(4.67575682331076,0.515032473483056,-4.95920238020822E-17));
#20466=CARTESIAN_POINT('Ctrl Pts',(4.66981719320886,0.524869491416437,-2.32356906808459E-16));
#20467=CARTESIAN_POINT('Ctrl Pts',(4.66375152405354,0.534621049953091,-4.9960036108132E-16));
#20468=CARTESIAN_POINT('Ctrl Pts',(4.63663984781298,0.578207518505316,-1.5147220868618E-15));
#20469=CARTESIAN_POINT('Ctrl Pts',(4.60699440856623,0.620121024458588,-2.06711395355149E-15));
#20470=CARTESIAN_POINT('Ctrl Pts',(4.57494698409233,0.660089312547657,-9.71445146547012E-16));
#20471=CARTESIAN_POINT('Ctrl Pts',(4.54970696039761,0.691567677969098,-1.08514439810198E-16));
#20472=CARTESIAN_POINT('Ctrl Pts',(4.52297617472456,0.721838929845157,8.87735236017173E-16));
#20473=CARTESIAN_POINT('Ctrl Pts',(4.49480733225647,0.750750410734639,5.27355936696949E-16));
#20474=CARTESIAN_POINT('Ctrl Pts',(4.48399014602072,0.761852779370735,3.51819881515091E-16));
#20475=CARTESIAN_POINT('Ctrl Pts',(4.47295717962163,0.772757609187209,-1.45592073936577E-15));
#20476=CARTESIAN_POINT('Ctrl Pts',(4.46173300251126,0.783435436762616,-1.27675647831893E-15));
#20477=CARTESIAN_POINT('Ctrl Pts',(4.42595244233202,0.817474337644931,-6.13637071966557E-16));
#20478=CARTESIAN_POINT('Ctrl Pts',(4.38819523463332,0.849248702584587,-1.66910301889349E-15));
#20479=CARTESIAN_POINT('Ctrl Pts',(4.34857042848663,0.878489835334903,-1.4432899320127E-15));
#20480=CARTESIAN_POINT('Ctrl Pts',(4.30894562233994,0.907730968085219,-1.25272571723038E-15));
#20481=CARTESIAN_POINT('Ctrl Pts',(4.26745256771982,0.934439563987207,-1.0624151382049E-17));
#20482=CARTESIAN_POINT('Ctrl Pts',(4.22418347496246,0.958295198918397,4.71844785465692E-16));
#20483=CARTESIAN_POINT('Origin',(3.53951905042299,8.32667268468867E-16,
-10.5));
#20484=CARTESIAN_POINT('Origin',(3.53951905042299,8.32667268468867E-16,
0.));
#20485=CARTESIAN_POINT('',(0.,0.,0.));
#20486=CARTESIAN_POINT('Origin',(96.460480949577,-1.76391462320204E-15,
-7.60421172358872));
#20487=CARTESIAN_POINT('',(95.5205266553345,1.22365637526845,-5.21861757766303));
#20488=CARTESIAN_POINT('',(95.5203485097068,1.22389080463934,-5.17716043768798));
#20489=CARTESIAN_POINT('',(95.5205266553345,1.22365637526844,-7.60421172358872));
#20490=CARTESIAN_POINT('',(96.0619671077198,-1.49064942821852,-4.99999999999999));
#20491=CARTESIAN_POINT('Ctrl Pts',(95.5203485097069,1.22389080463943,-5.17716043768799));
#20492=CARTESIAN_POINT('Ctrl Pts',(95.4222725293664,1.15010481933258,-5.17083051560054));
#20493=CARTESIAN_POINT('Ctrl Pts',(94.9624927983586,0.710147272658132,-5.13813881494215));
#20494=CARTESIAN_POINT('Ctrl Pts',(94.7305471663323,-0.566638877030392,
-5.07908533571281));
#20495=CARTESIAN_POINT('Ctrl Pts',(95.5681568698448,-1.35863299878938,-5.02636177857093));
#20496=CARTESIAN_POINT('Ctrl Pts',(96.0619671077198,-1.49064942821852,-4.99999999999999));
#20497=CARTESIAN_POINT('',(96.8589954712671,-1.49064924647019,-5.0000135609018));
#20498=CARTESIAN_POINT('Origin',(96.460480949577,-1.44499066804254E-15,
-4.99999999999999));
#20499=CARTESIAN_POINT('Ctrl Pts',(95.5205266553345,1.22365637526844,-5.21861757766303));
#20500=CARTESIAN_POINT('Ctrl Pts',(95.4750144572141,1.18869608173482,-5.21565740437065));
#20501=CARTESIAN_POINT('Ctrl Pts',(95.4313991185652,1.15115000799943,-5.21269723107828));
#20502=CARTESIAN_POINT('Ctrl Pts',(95.3899849632427,1.11125485071705,-5.20973705778591));
#20503=CARTESIAN_POINT('Ctrl Pts',(95.3485989120151,1.07138676672107,-5.20677889329923));
#20504=CARTESIAN_POINT('Ctrl Pts',(95.3094114587368,1.0291731200483,-5.20382072881256));
#20505=CARTESIAN_POINT('Ctrl Pts',(95.2726926383603,0.984889804870097,-5.20086256432588));
#20506=CARTESIAN_POINT('Ctrl Pts',(95.2359845401275,0.940619420719128,-5.19790526364323));
#20507=CARTESIAN_POINT('Ctrl Pts',(95.2017439775786,0.894280968963252,-5.19494796296057));
#20508=CARTESIAN_POINT('Ctrl Pts',(95.1702014867204,0.846184322550652,-5.19199066227792));
#20509=CARTESIAN_POINT('Ctrl Pts',(95.1378112632144,0.79679503575649,-5.18895388149492));
#20510=CARTESIAN_POINT('Ctrl Pts',(95.1082666015211,0.745552129788192,-5.18591710071193));
#20511=CARTESIAN_POINT('Ctrl Pts',(95.0817688683063,0.692821764206503,-5.18288031992893));
#20512=CARTESIAN_POINT('Ctrl Pts',(95.0559329333177,0.64140837401016,-5.17991938473316));
#20513=CARTESIAN_POINT('Ctrl Pts',(95.0329936325855,0.58858149012942,-5.17695844953738));
#20514=CARTESIAN_POINT('Ctrl Pts',(95.0130891572679,0.534701785630407,-5.17399751434161));
#20515=CARTESIAN_POINT('Ctrl Pts',(94.9924198898227,0.478751854552561,-5.170922810765));
#20516=CARTESIAN_POINT('Ctrl Pts',(94.9750236328371,0.421667129375691,-5.1678481071884));
#20517=CARTESIAN_POINT('Ctrl Pts',(94.9609977142078,0.363866770737305,-5.16477340361179));
#20518=CARTESIAN_POINT('Ctrl Pts',(94.9469717955786,0.30606641209892,-5.16169870003519));
#20519=CARTESIAN_POINT('Ctrl Pts',(94.9363162543708,0.247551045391105,-5.15862399645858));
#20520=CARTESIAN_POINT('Ctrl Pts',(94.9290685719962,0.18874620470976,-5.15554929288198));
#20521=CARTESIAN_POINT('Ctrl Pts',(94.9220560770625,0.131849582307344,-5.15257436349912));
#20522=CARTESIAN_POINT('Ctrl Pts',(94.918204319441,0.0744450502569582,-5.14959943411625));
#20523=CARTESIAN_POINT('Ctrl Pts',(94.9175736512373,0.0169135664489606,
-5.14662450473339));
#20524=CARTESIAN_POINT('Ctrl Pts',(94.9169441008334,-0.0405159482364207,
-5.14365484813195));
#20525=CARTESIAN_POINT('Ctrl Pts',(94.9195243124124,-0.0980714527019945,
-5.14068519153051));
#20526=CARTESIAN_POINT('Ctrl Pts',(94.9253229143521,-0.155366685246577,
-5.13771553492907));
#20527=CARTESIAN_POINT('Ctrl Pts',(94.9311157645249,-0.212605085329118,
-5.13474882399848));
#20528=CARTESIAN_POINT('Ctrl Pts',(94.9401206269862,-0.269583210779604,
-5.13178211306788));
#20529=CARTESIAN_POINT('Ctrl Pts',(94.9522941165142,-0.325916364388086,
-5.12881540213729));
#20530=CARTESIAN_POINT('Ctrl Pts',(94.9644601768167,-0.382215139053537,
-5.1258505017282));
#20531=CARTESIAN_POINT('Ctrl Pts',(94.9797909208417,-0.437869215515292,
-5.12288560131911));
#20532=CARTESIAN_POINT('Ctrl Pts',(94.9981916392351,-0.492502764316785,
-5.11992070091002));
#20533=CARTESIAN_POINT('Ctrl Pts',(95.0165881500904,-0.54712382052268,-5.11695647845985));
#20534=CARTESIAN_POINT('Ctrl Pts',(95.038053075711,-0.600724320370488,-5.11399225600968));
#20535=CARTESIAN_POINT('Ctrl Pts',(95.0624421197003,-0.652944431140126,
-5.11102803355951));
#20536=CARTESIAN_POINT('Ctrl Pts',(95.0868523696764,-0.705209946681921,
-5.10806123375279));
#20537=CARTESIAN_POINT('Ctrl Pts',(95.114191599417,-0.756092202470218,-5.10509443394606));
#20538=CARTESIAN_POINT('Ctrl Pts',(95.144268246225,-0.805253450495386,-5.10212763413933));
#20539=CARTESIAN_POINT('Ctrl Pts',(95.1743571322149,-0.854434703857716,
-5.09915962704368));
#20540=CARTESIAN_POINT('Ctrl Pts',(95.2071853615618,-0.901893124030684,
-5.09619161994802));
#20541=CARTESIAN_POINT('Ctrl Pts',(95.2425182043213,-0.947320300199004,
-5.09322361285237));
#20542=CARTESIAN_POINT('Ctrl Pts',(95.2779171534899,-0.992832468891667,
-5.09025005272796));
#20543=CARTESIAN_POINT('Ctrl Pts',(95.3158297384057,-1.03630540574857,-5.08727649260356));
#20544=CARTESIAN_POINT('Ctrl Pts',(95.3559817788718,-1.07746488662573,-5.08430293247915));
#20545=CARTESIAN_POINT('Ctrl Pts',(95.3912650578024,-1.11363344562234,-5.08168994070915));
#20546=CARTESIAN_POINT('Ctrl Pts',(95.4282768703245,-1.1480159863261,-5.07907694893915));
#20547=CARTESIAN_POINT('Ctrl Pts',(95.4668104992014,-1.18045247089848,-5.07646395716915));
#20548=CARTESIAN_POINT('Ctrl Pts',(95.5103555387519,-1.21710741476826,-5.07351113820852));
#20549=CARTESIAN_POINT('Ctrl Pts',(95.5560263432748,-1.25142937469358,-5.07055831924789));
#20550=CARTESIAN_POINT('Ctrl Pts',(95.6035414147712,-1.28316157738879,-5.06760550028725));
#20551=CARTESIAN_POINT('Ctrl Pts',(95.6509741899481,-1.31483881976484,-5.06465779562247));
#20552=CARTESIAN_POINT('Ctrl Pts',(95.7002444587964,-1.34393491375805,-5.06171009095769));
#20553=CARTESIAN_POINT('Ctrl Pts',(95.7510378262279,-1.37023335776525,-5.05876238629291));
#20554=CARTESIAN_POINT('Ctrl Pts',(95.8017825605679,-1.39650662181891,-5.05581750396493));
#20555=CARTESIAN_POINT('Ctrl Pts',(95.8540470385658,-1.41998729947719,-5.05287262163696));
#20556=CARTESIAN_POINT('Ctrl Pts',(95.9074896665142,-1.44050325957859,-5.04992773930898));
#20557=CARTESIAN_POINT('Ctrl Pts',(95.9609023205119,-1.46100771305315,-5.04698450865424));
#20558=CARTESIAN_POINT('Ctrl Pts',(96.0154913228705,-1.47855055532387,-5.04404127799949));
#20559=CARTESIAN_POINT('Ctrl Pts',(96.0708944764094,-1.49300749493256,-5.04109804734474));
#20560=CARTESIAN_POINT('Ctrl Pts',(96.1262885285363,-1.50746205961214,-5.03815530019234));
#20561=CARTESIAN_POINT('Ctrl Pts',(96.1824959553726,-1.51883159556475,-5.03521255303994));
#20562=CARTESIAN_POINT('Ctrl Pts',(96.2391409909009,-1.52704211555977,-5.03226980588753));
#20563=CARTESIAN_POINT('Ctrl Pts',(96.2958391305459,-1.53526033282972,-5.02932429994105));
#20564=CARTESIAN_POINT('Ctrl Pts',(96.3529751744367,-1.54031354422022,-5.02637879399458));
#20565=CARTESIAN_POINT('Ctrl Pts',(96.4101662980206,-1.54217944346265,-5.0234332880481));
#20566=CARTESIAN_POINT('Ctrl Pts',(96.4673854787933,-1.54404625808991,-5.02048633707639));
#20567=CARTESIAN_POINT('Ctrl Pts',(96.5246592645381,-1.54272265947058,-5.01753938610469));
#20568=CARTESIAN_POINT('Ctrl Pts',(96.5816061911329,-1.5382384977168,-5.01459243513298));
#20569=CARTESIAN_POINT('Ctrl Pts',(96.6386579446969,-1.53374608159154,-5.01164005946222));
#20570=CARTESIAN_POINT('Ctrl Pts',(96.6953811140427,-1.52608155800054,-5.00868768379145));
#20571=CARTESIAN_POINT('Ctrl Pts',(96.7514019547242,-1.51532635717992,-5.00573530812069));
#20572=CARTESIAN_POINT('Ctrl Pts',(96.7875916908457,-1.50837844502977,-5.00382805904772));
#20573=CARTESIAN_POINT('Ctrl Pts',(96.8234885518963,-1.50014176996171,-5.00192080997476));
#20574=CARTESIAN_POINT('Ctrl Pts',(96.8589954712671,-1.49064924647019,-5.0000135609018));
#20575=CARTESIAN_POINT('Origin',(96.460480949577,-1.76391462320204E-15,
-7.60421172358872));
#20576=CARTESIAN_POINT('',(95.5205266553345,1.22365637526845,-5.71870242479901));
#20577=CARTESIAN_POINT('',(95.5205266553345,1.22365637526844,-5.67707251971253));
#20578=CARTESIAN_POINT('',(95.5205266553345,1.22365637526844,-7.60421172358872));
#20579=CARTESIAN_POINT('',(98.0032284820363,0.000204932544027349,-5.35421171129878));
#20580=CARTESIAN_POINT('Ctrl Pts',(95.5205266553345,1.22365637526844,-5.67707251971253));
#20581=CARTESIAN_POINT('Ctrl Pts',(95.4748841937922,1.18859601960518,-5.67411288279253));
#20582=CARTESIAN_POINT('Ctrl Pts',(95.431194703542,1.15096983641646,-5.67115324587254));
#20583=CARTESIAN_POINT('Ctrl Pts',(95.389751479782,1.11102988371714,-5.66819360895254));
#20584=CARTESIAN_POINT('Ctrl Pts',(95.3482719803909,1.07105497121361,-5.66523138143541));
#20585=CARTESIAN_POINT('Ctrl Pts',(95.3090430547088,1.02876260271372,-5.66226915391828));
#20586=CARTESIAN_POINT('Ctrl Pts',(95.2723218698293,0.98444248243012,-5.65930692640114));
#20587=CARTESIAN_POINT('Ctrl Pts',(95.235586418872,0.940105143903381,-5.65634354806688));
#20588=CARTESIAN_POINT('Ctrl Pts',(95.2013609632822,0.893738901946624,-5.65338016973261));
#20589=CARTESIAN_POINT('Ctrl Pts',(95.1698609586239,0.845664850252347,-5.65041679139835));
#20590=CARTESIAN_POINT('Ctrl Pts',(95.1382994660804,0.797496958198043,-5.64744762856122));
#20591=CARTESIAN_POINT('Ctrl Pts',(95.1094743206732,0.747615046009535,-5.64447846572409));
#20592=CARTESIAN_POINT('Ctrl Pts',(95.0835559073487,0.696366590298917,-5.64150930288695));
#20593=CARTESIAN_POINT('Ctrl Pts',(95.0578728079937,0.645583420691764,-5.63856709715883));
#20594=CARTESIAN_POINT('Ctrl Pts',(95.0350439730977,0.593458919368784,-5.63562489143071));
#20595=CARTESIAN_POINT('Ctrl Pts',(95.015187493322,0.54034787434249,-5.63268268570259));
#20596=CARTESIAN_POINT('Ctrl Pts',(94.9951440173245,0.486736661871289,-5.62971277207452));
#20597=CARTESIAN_POINT('Ctrl Pts',(94.9780457917068,0.431897056842871,-5.62674285844645));
#20598=CARTESIAN_POINT('Ctrl Pts',(94.9640403772373,0.376184281244761,-5.62377294481839));
#20599=CARTESIAN_POINT('Ctrl Pts',(94.9500597005158,0.320569911059979,-5.62080827694545));
#20600=CARTESIAN_POINT('Ctrl Pts',(94.9391611181184,0.264085933076503,-5.61784360907251));
#20601=CARTESIAN_POINT('Ctrl Pts',(94.9314431550967,0.207104860036487,-5.61487894119957));
#20602=CARTESIAN_POINT('Ctrl Pts',(94.9237328082311,0.15018001643842,-5.61191719888789));
#20603=CARTESIAN_POINT('Ctrl Pts',(94.9191969316952,0.0927595638259635,
-5.60895545657621));
#20604=CARTESIAN_POINT('Ctrl Pts',(94.9178831141031,0.0352266659123865,
-5.60599371426454));
#20605=CARTESIAN_POINT('Ctrl Pts',(94.9165700869607,-0.0222716177118651,
-5.60303375386563));
#20606=CARTESIAN_POINT('Ctrl Pts',(94.918475287831,-0.0798816922939508,
-5.60007379346672));
#20607=CARTESIAN_POINT('Ctrl Pts',(94.9235943283679,-0.137217030824841,
-5.59711383306781));
#20608=CARTESIAN_POINT('Ctrl Pts',(94.928712260639,-0.194539956328421,-5.59415451349653));
#20609=CARTESIAN_POINT('Ctrl Pts',(94.9370426047138,-0.251587744788432,
-5.59119519392525));
#20610=CARTESIAN_POINT('Ctrl Pts',(94.9485290217771,-0.307977869370634,
-5.58823587435398));
#20611=CARTESIAN_POINT('Ctrl Pts',(94.9600258197224,-0.364418956687777,
-5.58527388028925));
#20612=CARTESIAN_POINT('Ctrl Pts',(94.9746842868066,-0.420200680143225,
-5.58231188622452));
#20613=CARTESIAN_POINT('Ctrl Pts',(94.992396971953,-0.474950981306263,-5.57934989215979));
#20614=CARTESIAN_POINT('Ctrl Pts',(95.0101171507595,-0.529724445538065,
-5.57638664497187));
#20615=CARTESIAN_POINT('Ctrl Pts',(95.0308939360851,-0.583465129881837,
-5.57342339778395));
#20616=CARTESIAN_POINT('Ctrl Pts',(95.0545710783864,-0.635819498040814,
-5.57046015059603));
#20617=CARTESIAN_POINT('Ctrl Pts',(95.0782936927137,-0.68827441292784,-5.5674912124826));
#20618=CARTESIAN_POINT('Ctrl Pts',(95.1049275530735,-0.73933722734849,-5.56452227436917));
#20619=CARTESIAN_POINT('Ctrl Pts',(95.1342700994957,-0.788678503020507,
-5.56155333625574));
#20620=CARTESIAN_POINT('Ctrl Pts',(95.1604802446076,-0.832752455456761,
-5.55890134083375));
#20621=CARTESIAN_POINT('Ctrl Pts',(95.1888508426266,-0.875452974566531,
-5.55624934541176));
#20622=CARTESIAN_POINT('Ctrl Pts',(95.2192098937526,-0.916567054815212,
-5.55359734998977));
#20623=CARTESIAN_POINT('Ctrl Pts',(95.2532166176942,-0.962621036256481,
-5.5506267144506));
#20624=CARTESIAN_POINT('Ctrl Pts',(95.289860525436,-1.0068755466702,-5.54765607891144));
#20625=CARTESIAN_POINT('Ctrl Pts',(95.3289242373537,-1.049013063323,-5.54468544337228));
#20626=CARTESIAN_POINT('Ctrl Pts',(95.3679189255036,-1.09107612493763,-5.54172005680837));
#20627=CARTESIAN_POINT('Ctrl Pts',(95.4093245796525,-1.13102923844691,-5.53875467024447));
#20628=CARTESIAN_POINT('Ctrl Pts',(95.4528825877961,-1.16858655705792,-5.53578928368057));
#20629=CARTESIAN_POINT('Ctrl Pts',(95.4963975867957,-1.20610679160112,-5.5328268251371));
#20630=CARTESIAN_POINT('Ctrl Pts',(95.5420603362235,-1.24123557973104,-5.52986436659364));
#20631=CARTESIAN_POINT('Ctrl Pts',(95.5895755179663,-1.27372396114343,-5.52690190805017));
#20632=CARTESIAN_POINT('Ctrl Pts',(95.6370620606586,-1.30619276067987,-5.52394123508337));
#20633=CARTESIAN_POINT('Ctrl Pts',(95.6863983929707,-1.33602401481992,-5.52098056211656));
#20634=CARTESIAN_POINT('Ctrl Pts',(95.7372580288026,-1.36301049404125,-5.51801988914976));
#20635=CARTESIAN_POINT('Ctrl Pts',(95.7881065725598,-1.38999108772998,-5.51505986188176));
#20636=CARTESIAN_POINT('Ctrl Pts',(95.8404773000814,-1.41412789423585,-5.51209983461376));
#20637=CARTESIAN_POINT('Ctrl Pts',(95.894018740221,-1.43525940699636,-5.50913980734576));
#20638=CARTESIAN_POINT('Ctrl Pts',(95.9476083176209,-1.45640991837041,-5.50617711881943));
#20639=CARTESIAN_POINT('Ctrl Pts',(96.002370225348,-1.47454954419522,-5.50321443029311));
#20640=CARTESIAN_POINT('Ctrl Pts',(96.0579338846565,-1.48956532603436,-5.50025174176679));
#20641=CARTESIAN_POINT('Ctrl Pts',(96.1135209303122,-1.50458742790881,-5.49728780626603));
#20642=CARTESIAN_POINT('Ctrl Pts',(96.1699098895527,-1.51648295576778,-5.49432387076527));
#20643=CARTESIAN_POINT('Ctrl Pts',(96.2267190814007,-1.52518995177216,-5.49135993526452));
#20644=CARTESIAN_POINT('Ctrl Pts',(96.2836369827036,-1.53391360938986,-5.48839032800886));
#20645=CARTESIAN_POINT('Ctrl Pts',(96.3409762031023,-1.53943649198693,-5.4854207207532));
#20646=CARTESIAN_POINT('Ctrl Pts',(96.3983499902363,-1.54174859944526,-5.48245111349755));
#20647=CARTESIAN_POINT('Ctrl Pts',(96.4494786580482,-1.54380903470825,-5.47980474709068));
#20648=CARTESIAN_POINT('Ctrl Pts',(96.5006344931726,-1.54332039128355,-5.4771583806838));
#20649=CARTESIAN_POINT('Ctrl Pts',(96.5515469365361,-1.5403103537986,-5.47451201427693));
#20650=CARTESIAN_POINT('Ctrl Pts',(96.6086915661517,-1.5369318579763,-5.47154170646695));
#20651=CARTESIAN_POINT('Ctrl Pts',(96.6657666142044,-1.53036198970351,-5.46857139865697));
#20652=CARTESIAN_POINT('Ctrl Pts',(96.7223874348522,-1.52060974381029,-5.465601090847));
#20653=CARTESIAN_POINT('Ctrl Pts',(96.7789084359758,-1.51087469061287,-5.46263601953322));
#20654=CARTESIAN_POINT('Ctrl Pts',(96.8349762896129,-1.49796848339876,-5.45967094821944));
#20655=CARTESIAN_POINT('Ctrl Pts',(96.8902104071771,-1.48195195376596,-5.45670587690567));
#20656=CARTESIAN_POINT('Ctrl Pts',(96.9453901259224,-1.46595119844679,-5.45374372582279));
#20657=CARTESIAN_POINT('Ctrl Pts',(96.9997372373803,-1.44684633457203,-5.45078157473993));
#20658=CARTESIAN_POINT('Ctrl Pts',(97.0528820496656,-1.42474907847445,-5.44781942365706));
#20659=CARTESIAN_POINT('Ctrl Pts',(97.1059949740077,-1.40266508116957,-5.44485904992369));
#20660=CARTESIAN_POINT('Ctrl Pts',(97.1579065489178,-1.37759245067629,-5.44189867619032));
#20661=CARTESIAN_POINT('Ctrl Pts',(97.2082650614677,-1.34969178778116,-5.43893830245695));
#20662=CARTESIAN_POINT('Ctrl Pts',(97.2586127376763,-1.32179712865954,-5.43597856574836));
#20663=CARTESIAN_POINT('Ctrl Pts',(97.3074075593723,-1.29107589793588,-5.43301882903976));
#20664=CARTESIAN_POINT('Ctrl Pts',(97.3543225121326,-1.25773457495933,-5.43005909233116));
#20665=CARTESIAN_POINT('Ctrl Pts',(97.4012798979,-1.22436309587025,-5.42709667863961));
#20666=CARTESIAN_POINT('Ctrl Pts',(97.446353590799,-1.18836709109256,-5.42413426494806));
#20667=CARTESIAN_POINT('Ctrl Pts',(97.4892468475387,-1.14999553355268,-5.42117185125652));
#20668=CARTESIAN_POINT('Ctrl Pts',(97.532158277977,-1.11160771813977,-5.41820818240232));
#20669=CARTESIAN_POINT('Ctrl Pts',(97.5728870606587,-1.07084271222311,-5.41524451354813));
#20670=CARTESIAN_POINT('Ctrl Pts',(97.6111731483929,-1.02798660671445,-5.41228084469394));
#20671=CARTESIAN_POINT('Ctrl Pts',(97.6495327267123,-0.985048238418837,
-5.40931148704332));
#20672=CARTESIAN_POINT('Ctrl Pts',(97.6854399142855,-0.940011158372543,
-5.40634212939271));
#20673=CARTESIAN_POINT('Ctrl Pts',(97.7186754499643,-0.893194043416801,
-5.4033727717421));
#20674=CARTESIAN_POINT('Ctrl Pts',(97.7483218914283,-0.851432692811103,
-5.4007240740161));
#20675=CARTESIAN_POINT('Ctrl Pts',(97.7758430203872,-0.808255648373526,
-5.39807537629011));
#20676=CARTESIAN_POINT('Ctrl Pts',(97.8011141758143,-0.763905460582941,
-5.39542667856411));
#20677=CARTESIAN_POINT('Ctrl Pts',(97.8306220844796,-0.712119886536653,
-5.39233392204945));
#20678=CARTESIAN_POINT('Ctrl Pts',(97.8571762815607,-0.658533688473516,
-5.38924116553479));
#20679=CARTESIAN_POINT('Ctrl Pts',(97.8805635330969,-0.603501827655418,
-5.38614840902013));
#20680=CARTESIAN_POINT('Ctrl Pts',(97.9038863169094,-0.548621663961602,
-5.38306417778996));
#20681=CARTESIAN_POINT('Ctrl Pts',(97.9240593452705,-0.49230418697146,-5.37997994655978));
#20682=CARTESIAN_POINT('Ctrl Pts',(97.9409154985417,-0.434928208135278,
-5.37689571532961));
#20683=CARTESIAN_POINT('Ctrl Pts',(97.9577436590148,-0.377647512852836,
-5.37381660604277));
#20684=CARTESIAN_POINT('Ctrl Pts',(97.9712657552404,-0.319312245702585,
-5.37073749675593));
#20685=CARTESIAN_POINT('Ctrl Pts',(97.9813630912672,-0.260320016686897,
-5.36765838746908));
#20686=CARTESIAN_POINT('Ctrl Pts',(97.9914417164285,-0.201437103203514,
-5.36458498392478));
#20687=CARTESIAN_POINT('Ctrl Pts',(97.9981081279234,-0.14190010128785,-5.36151158038048));
#20688=CARTESIAN_POINT('Ctrl Pts',(98.0012942200649,-0.0821186062255512,
-5.35843817683618));
#20689=CARTESIAN_POINT('Ctrl Pts',(98.002754693151,-0.0547153608980888,
-5.35702935908703));
#20690=CARTESIAN_POINT('Ctrl Pts',(98.0034845801625,-0.0272608981217706,
-5.35562054133788));
#20691=CARTESIAN_POINT('Ctrl Pts',(98.0034809359953,0.000204726815253606,
-5.35421172358872));
#20692=CARTESIAN_POINT('Ctrl Pts',(98.001071826132,0.000206690037458163,
-5.35421160630865));
#20693=CARTESIAN_POINT('Ctrl Pts',(98.0013064289223,0.24592255753606,-5.3415881851562));
#20694=CARTESIAN_POINT('Ctrl Pts',(97.8302188552265,1.00442272708515,-5.30260298543279));
#20695=CARTESIAN_POINT('Ctrl Pts',(96.7594849884078,1.73376085900502,-5.24358592922591));
#20696=CARTESIAN_POINT('Ctrl Pts',(95.8307226241933,1.4573960907615,-5.19719229417148));
#20697=CARTESIAN_POINT('Ctrl Pts',(95.5203485097069,1.22389080463943,-5.17716043768799));
#20698=CARTESIAN_POINT('',(98.0034809091236,0.000353326024287275,-5.39578827645383));
#20699=CARTESIAN_POINT('Ctrl Pts',(98.0034809091234,0.000353326844981171,
-5.39578827641126));
#20700=CARTESIAN_POINT('Ctrl Pts',(98.003476520187,0.0195200805027758,-5.39479395094765));
#20701=CARTESIAN_POINT('Ctrl Pts',(98.0031150178881,0.0386823176935148,
-5.39379962548405));
#20702=CARTESIAN_POINT('Ctrl Pts',(98.0023968252469,0.0578310674047492,
-5.39280530002044));
#20703=CARTESIAN_POINT('Ctrl Pts',(98.000251161033,0.115039655516275,-5.38983466450877));
#20704=CARTESIAN_POINT('Ctrl Pts',(97.9949128750843,0.17224752489316,-5.38686402899711));
#20705=CARTESIAN_POINT('Ctrl Pts',(97.9863826482311,0.229069871533753,-5.38389339348544));
#20706=CARTESIAN_POINT('Ctrl Pts',(97.9778674938922,0.285791815729505,-5.38092800694861));
#20707=CARTESIAN_POINT('Ctrl Pts',(97.966171670182,0.342129078111066,-5.37796262041179));
#20708=CARTESIAN_POINT('Ctrl Pts',(97.9513477698711,0.397699791483852,-5.37499723387497));
#20709=CARTESIAN_POINT('Ctrl Pts',(97.9365385066668,0.453215634381072,-5.37203477535831));
#20710=CARTESIAN_POINT('Ctrl Pts',(97.9186074202501,0.507965926904492,-5.36907231684166));
#20711=CARTESIAN_POINT('Ctrl Pts',(97.8976582118212,0.561578593687674,-5.366109858325));
#20712=CARTESIAN_POINT('Ctrl Pts',(97.8767216302059,0.615158946259722,-5.3631491853847));
#20713=CARTESIAN_POINT('Ctrl Pts',(97.8527707220503,0.667602547953602,-5.36018851244439));
#20714=CARTESIAN_POINT('Ctrl Pts',(97.8259584511658,0.718554237796173,-5.35722783950409));
#20715=CARTESIAN_POINT('Ctrl Pts',(97.7991520278174,0.76949481549371,-5.35426781226224));
#20716=CARTESIAN_POINT('Ctrl Pts',(97.7694857233649,0.818943666434629,-5.35130778502038));
#20717=CARTESIAN_POINT('Ctrl Pts',(97.7371589055721,0.866569325949268,-5.34834775777853));
#20718=CARTESIAN_POINT('Ctrl Pts',(97.7048030238451,0.914237804062493,-5.34538506927761));
#20719=CARTESIAN_POINT('Ctrl Pts',(97.6697821416117,0.960079382567713,-5.34242238077668));
#20720=CARTESIAN_POINT('Ctrl Pts',(97.6323387667623,1.00379193875112,-5.33945969227576));
#20721=CARTESIAN_POINT('Ctrl Pts',(97.5948796322591,1.04752289324275,-5.33649575680003));
#20722=CARTESIAN_POINT('Ctrl Pts',(97.5549963330695,1.08912266127467,-5.3335318213243));
#20723=CARTESIAN_POINT('Ctrl Pts',(97.5129692854056,1.12832499881233,-5.33056788584858));
#20724=CARTESIAN_POINT('Ctrl Pts',(97.470861815224,1.1676023535319,-5.32759827861701));
#20725=CARTESIAN_POINT('Ctrl Pts',(97.4266028005723,1.20447277522765,-5.32462867138545));
#20726=CARTESIAN_POINT('Ctrl Pts',(97.3805061228808,1.23871008734385,-5.32165906415388));
#20727=CARTESIAN_POINT('Ctrl Pts',(97.3394270509994,1.26922068107591,-5.31901269753846));
#20728=CARTESIAN_POINT('Ctrl Pts',(97.2968892605857,1.29764065707482,-5.31636633092304));
#20729=CARTESIAN_POINT('Ctrl Pts',(97.2531318732976,1.32384044096142,-5.31371996430762));
#20730=CARTESIAN_POINT('Ctrl Pts',(97.2040181546192,1.35324733417394,-5.31074965658303));
#20731=CARTESIAN_POINT('Ctrl Pts',(97.1531637475995,1.37997846532703,-5.30777934885844));
#20732=CARTESIAN_POINT('Ctrl Pts',(97.1008914960143,1.40382453747323,-5.30480904113386));
#20733=CARTESIAN_POINT('Ctrl Pts',(97.0487113976704,1.42762857024337,-5.30184396990619));
#20734=CARTESIAN_POINT('Ctrl Pts',(96.9951188865058,1.44855742488113,-5.29887889867853));
#20735=CARTESIAN_POINT('Ctrl Pts',(96.9404626617286,1.46644691550702,-5.29591382745087));
#20736=CARTESIAN_POINT('Ctrl Pts',(96.8858602666252,1.48431878718006,-5.29295167645449));
#20737=CARTESIAN_POINT('Ctrl Pts',(96.8301967265524,1.49915706444531,-5.28998952545811));
#20738=CARTESIAN_POINT('Ctrl Pts',(96.7738404093114,1.5108457396422,-5.28702737446173));
#20739=CARTESIAN_POINT('Ctrl Pts',(96.7175179069856,1.52252740140064,-5.28406700081508));
#20740=CARTESIAN_POINT('Ctrl Pts',(96.6605039608838,1.53106310175209,-5.28110662716842));
#20741=CARTESIAN_POINT('Ctrl Pts',(96.6031796293305,1.53638734920482,-5.27814625352177));
#20742=CARTESIAN_POINT('Ctrl Pts',(96.5458676330524,1.54171045096503,-5.27518651689996));
#20743=CARTESIAN_POINT('Ctrl Pts',(96.4882459026943,1.54382342377984,-5.27222678027816));
#20744=CARTESIAN_POINT('Ctrl Pts',(96.4307009420754,1.54271259512367,-5.26926704365635));
#20745=CARTESIAN_POINT('Ctrl Pts',(96.3731039339497,1.54160076175984,-5.26630463005101));
#20746=CARTESIAN_POINT('Ctrl Pts',(96.3155843566986,1.53725930964672,-5.26334221644566));
#20747=CARTESIAN_POINT('Ctrl Pts',(96.2585276485382,1.52972672860205,-5.26037980284032));
#20748=CARTESIAN_POINT('Ctrl Pts',(96.2014467656781,1.52219095603283,-5.25741613407214));
#20749=CARTESIAN_POINT('Ctrl Pts',(96.1448296562402,1.51146145538865,-5.25445246530397));
#20750=CARTESIAN_POINT('Ctrl Pts',(96.0890523559733,1.49762805791478,-5.25148879653579));
#20751=CARTESIAN_POINT('Ctrl Pts',(96.0331679905079,1.48376810706812,-5.24851943896978));
#20752=CARTESIAN_POINT('Ctrl Pts',(95.9781271553534,1.46679250751296,-5.24555008140377));
#20753=CARTESIAN_POINT('Ctrl Pts',(95.9242905513001,1.44684099222951,-5.24258072383776));
#20754=CARTESIAN_POINT('Ctrl Pts',(95.8762677299935,1.42904402917615,-5.23993202542344));
#20755=CARTESIAN_POINT('Ctrl Pts',(95.8292030686934,1.40887998385358,-5.23728332700912));
#20756=CARTESIAN_POINT('Ctrl Pts',(95.7833362211146,1.38647899973839,-5.2346346285948));
#20757=CARTESIAN_POINT('Ctrl Pts',(95.7319583286611,1.36138646747434,-5.23166768080013));
#20758=CARTESIAN_POINT('Ctrl Pts',(95.6818691784263,1.33338154606915,-5.22870073300546));
#20759=CARTESIAN_POINT('Ctrl Pts',(95.6334196355374,1.30261989191745,-5.22573378521079));
#20760=CARTESIAN_POINT('Ctrl Pts',(95.5946843171056,1.27802600726951,-5.2233617160282));
#20761=CARTESIAN_POINT('Ctrl Pts',(95.5569968453978,1.25167103073437,-5.22098964684561));
#20762=CARTESIAN_POINT('Ctrl Pts',(95.5205266553345,1.22365637526844,-5.21861757766303));
#20763=CARTESIAN_POINT('Ctrl Pts',(95.5205266553345,1.22365637526844,-5.71870242479901));
#20764=CARTESIAN_POINT('Ctrl Pts',(95.4749536865538,1.18864940062048,-5.7157321319398));
#20765=CARTESIAN_POINT('Ctrl Pts',(95.4314109543683,1.15114839457577,-5.71276183908059));
#20766=CARTESIAN_POINT('Ctrl Pts',(95.3901664893481,1.11142969018513,-5.70979154622138));
#20767=CARTESIAN_POINT('Ctrl Pts',(95.387181520648,1.10855514473135,-5.70957657843817));
#20768=CARTESIAN_POINT('Ctrl Pts',(95.3842085724413,1.10566899796144,-5.70936161065496));
#20769=CARTESIAN_POINT('Ctrl Pts',(95.3812477380923,1.10277136126598,-5.70914664287175));
#20770=CARTESIAN_POINT('Ctrl Pts',(95.3403390789929,1.06273587876419,-5.7061765193443));
#20771=CARTESIAN_POINT('Ctrl Pts',(95.3015760537394,1.02033766352785,-5.70320639581685));
#20772=CARTESIAN_POINT('Ctrl Pts',(95.2652430743696,0.975835755478162,-5.7002362722894));
#20773=CARTESIAN_POINT('Ctrl Pts',(95.2289742695963,0.93141245072607,-5.69727139486294));
#20774=CARTESIAN_POINT('Ctrl Pts',(95.1951273183703,0.884893228937414,-5.69430651743647));
#20775=CARTESIAN_POINT('Ctrl Pts',(95.1639495713149,0.836573598185967,-5.69134164001001));
#20776=CARTESIAN_POINT('Ctrl Pts',(95.1328025923278,0.788301652140296,-5.68837968850217));
#20777=CARTESIAN_POINT('Ctrl Pts',(95.1043198796868,0.738233253343213,-5.68541773699433));
#20778=CARTESIAN_POINT('Ctrl Pts',(95.0787071842613,0.686695173628923,-5.6824557854865));
#20779=CARTESIAN_POINT('Ctrl Pts',(95.0531099036377,0.635188111707661,-5.67949561660617));
#20780=CARTESIAN_POINT('Ctrl Pts',(95.0303794476811,0.582213588207815,-5.67653544772585));
#20781=CARTESIAN_POINT('Ctrl Pts',(95.0106759326748,0.528123482686638,-5.67357527884552));
#20782=CARTESIAN_POINT('Ctrl Pts',(94.990976690292,0.47404510637522,-5.67061575186525));
#20783=CARTESIAN_POINT('Ctrl Pts',(94.9743032639424,0.418852117964194,-5.66765622488498));
#20784=CARTESIAN_POINT('Ctrl Pts',(94.9607670341548,0.362914827320599,-5.66469669790471));
#20785=CARTESIAN_POINT('Ctrl Pts',(94.9472185870789,0.306927049796871,-5.66173449976747));
#20786=CARTESIAN_POINT('Ctrl Pts',(94.9368131183915,0.250194135348607,-5.65877230163023));
#20787=CARTESIAN_POINT('Ctrl Pts',(94.9296112862886,0.193098612172937,-5.65581010349299));
#20788=CARTESIAN_POINT('Ctrl Pts',(94.9224064111878,0.135978964365221,-5.65284665373502));
#20789=CARTESIAN_POINT('Ctrl Pts',(94.9184079084876,0.0784969234628313,
-5.64988320397706));
#20790=CARTESIAN_POINT('Ctrl Pts',(94.9176243904604,0.0210389636377934,
-5.64691975421909));
#20791=CARTESIAN_POINT('Ctrl Pts',(94.9168393691463,-0.0365292371737625,
-5.6439506186758));
#20792=CARTESIAN_POINT('Ctrl Pts',(94.9192816368559,-0.0940727419538194,
-5.6409814831325));
#20793=CARTESIAN_POINT('Ctrl Pts',(94.9249076455712,-0.151207235358418,
-5.63801234758921));
#20794=CARTESIAN_POINT('Ctrl Pts',(94.9299296036579,-0.202207339642452,
-5.63536200077912));
#20795=CARTESIAN_POINT('Ctrl Pts',(94.9374875626971,-0.252881366441544,
-5.63271165396902));
#20796=CARTESIAN_POINT('Ctrl Pts',(94.9475163614128,-0.302963949936223,
-5.63006130715892));
#20797=CARTESIAN_POINT('Ctrl Pts',(94.9587555728084,-0.359091185021949,
-5.62709108022395));
#20798=CARTESIAN_POINT('Ctrl Pts',(94.9731456644885,-0.414708903174088,
-5.62412085328898));
#20799=CARTESIAN_POINT('Ctrl Pts',(94.990624657851,-0.469437409750782,-5.621150626354));
#20800=CARTESIAN_POINT('Ctrl Pts',(95.0080727808134,-0.524069257963947,
-5.61818564526425));
#20801=CARTESIAN_POINT('Ctrl Pts',(95.0285988198162,-0.577814519235535,
-5.6152206641745));
#20802=CARTESIAN_POINT('Ctrl Pts',(95.0520900154419,-0.630304669700307,
-5.61225568308475));
#20803=CARTESIAN_POINT('Ctrl Pts',(95.0755580300179,-0.682743023023606,
-5.60929362783049));
#20804=CARTESIAN_POINT('Ctrl Pts',(95.1019851919303,-0.733928246044934,
-5.60633157257623));
#20805=CARTESIAN_POINT('Ctrl Pts',(95.1312098473067,-0.783509627681161,
-5.60336951732197));
#20806=CARTESIAN_POINT('Ctrl Pts',(95.160416913738,-0.833061168616398,-5.60040924478941));
#20807=CARTESIAN_POINT('Ctrl Pts',(95.1924178718189,-0.881010333496331,
-5.59744897225685));
#20808=CARTESIAN_POINT('Ctrl Pts',(95.2270051316858,-0.927030963170926,
-5.59448869972429));
#20809=CARTESIAN_POINT('Ctrl Pts',(95.2615848885443,-0.973041609598184,
-5.59152906936315));
#20810=CARTESIAN_POINT('Ctrl Pts',(95.2987495201731,-1.0171241349703,-5.588569439002));
#20811=CARTESIAN_POINT('Ctrl Pts',(95.3382494053052,-1.05898317316256,-5.58560980864086));
#20812=CARTESIAN_POINT('Ctrl Pts',(95.3777849236423,-1.10087997277314,-5.5826475083703));
#20813=CARTESIAN_POINT('Ctrl Pts',(95.4196595471311,-1.14054889643074,-5.57968520809974));
#20814=CARTESIAN_POINT('Ctrl Pts',(95.4635857456885,-1.17773042436041,-5.57672290782919));
#20815=CARTESIAN_POINT('Ctrl Pts',(95.5075304960702,-1.214927655565,-5.57375935645847));
#20816=CARTESIAN_POINT('Ctrl Pts',(95.5535281325113,-1.24963508129856,-5.57079580508775));
#20817=CARTESIAN_POINT('Ctrl Pts',(95.6012594266263,-1.2816346493827,-5.56783225371703));
#20818=CARTESIAN_POINT('Ctrl Pts',(95.6490822614954,-1.31369558736362,-5.5648630187433));
#20819=CARTESIAN_POINT('Ctrl Pts',(95.6986449481703,-1.34303802339517,-5.56189378376956));
#20820=CARTESIAN_POINT('Ctrl Pts',(95.7496016140659,-1.36948879891122,-5.55892454879583));
#20821=CARTESIAN_POINT('Ctrl Pts',(95.795071575626,-1.3930915155492,-5.55627502301258));
#20822=CARTESIAN_POINT('Ctrl Pts',(95.8416509103096,-1.41439231708115,-5.55362549722934));
#20823=CARTESIAN_POINT('Ctrl Pts',(95.8890819197383,-1.43330113678159,-5.55097597144609));
#20824=CARTESIAN_POINT('Ctrl Pts',(95.9422538451485,-1.45449862683748,-5.54800575451384));
#20825=CARTESIAN_POINT('Ctrl Pts',(95.9967175171977,-1.47277737640127,-5.54503553758159));
#20826=CARTESIAN_POINT('Ctrl Pts',(96.0521208977492,-1.48798221362729,-5.54206532064933));
#20827=CARTESIAN_POINT('Ctrl Pts',(96.10742645343,-1.50316020391331,-5.53910034818202));
#20828=CARTESIAN_POINT('Ctrl Pts',(96.1636679256365,-1.51527491800201,-5.53613537571471));
#20829=CARTESIAN_POINT('Ctrl Pts',(96.2204749385166,-1.5242198380335,-5.5331704032474));
#20830=CARTESIAN_POINT('Ctrl Pts',(96.2772259103806,-1.53315593376,-5.53020835577229));
#20831=CARTESIAN_POINT('Ctrl Pts',(96.3345408051066,-1.53892835047816,-5.52724630829718));
#20832=CARTESIAN_POINT('Ctrl Pts',(96.3920375051383,-1.54148126648149,-5.52428426082207));
#20833=CARTESIAN_POINT('Ctrl Pts',(96.4494996169699,-1.54403264673112,-5.52132399522124));
#20834=CARTESIAN_POINT('Ctrl Pts',(96.5071427975625,-1.543368342504,-5.51836372962041));
#20835=CARTESIAN_POINT('Ctrl Pts',(96.5645804497071,-1.53948442475806,-5.51540346401958));
#20836=CARTESIAN_POINT('Ctrl Pts',(96.6220056584249,-1.53560134843313,-5.51244383973759));
#20837=CARTESIAN_POINT('Ctrl Pts',(96.679224907255,-1.52850007866818,-5.5094842154556));
#20838=CARTESIAN_POINT('Ctrl Pts',(96.7358544800438,-1.5182287109386,-5.5065245911736));
#20839=CARTESIAN_POINT('Ctrl Pts',(96.7925351651291,-1.50794807255469,-5.50356229561605));
#20840=CARTESIAN_POINT('Ctrl Pts',(96.848624596372,-1.49449171112577,-5.50060000005849));
#20841=CARTESIAN_POINT('Ctrl Pts',(96.9037484226053,-1.47795904792898,-5.49763770450093));
#20842=CARTESIAN_POINT('Ctrl Pts',(96.9588955437214,-1.46141939816253,-5.49467415710125));
#20843=CARTESIAN_POINT('Ctrl Pts',(97.0130757548387,-1.44180103184701,-5.49171060970156));
#20844=CARTESIAN_POINT('Ctrl Pts',(97.0659321690558,-1.41925255709888,-5.48874706230188));
#20845=CARTESIAN_POINT('Ctrl Pts',(97.1188899761845,-1.39666082827187,-5.48577783001599));
#20846=CARTESIAN_POINT('Ctrl Pts',(97.1705184429738,-1.37112799073345,-5.4828085977301));
#20847=CARTESIAN_POINT('Ctrl Pts',(97.2204837749586,-1.34284947235793,-5.47983936544422));
#20848=CARTESIAN_POINT('Ctrl Pts',(97.2650700384127,-1.31761530658144,-5.4771897888739));
#20849=CARTESIAN_POINT('Ctrl Pts',(97.3083321370077,-1.29019560379683,-5.47454021230359));
#20850=CARTESIAN_POINT('Ctrl Pts',(97.3500540021067,-1.26075722651627,-5.47189063573328));
#20851=CARTESIAN_POINT('Ctrl Pts',(97.396541183261,-1.22795650741416,-5.46893843439439));
#20852=CARTESIAN_POINT('Ctrl Pts',(97.4413143141274,-1.19250873107517,-5.4659862330555));
#20853=CARTESIAN_POINT('Ctrl Pts',(97.4840534865511,-1.15462039716629,-5.46303403171661));
#20854=CARTESIAN_POINT('Ctrl Pts',(97.5267172034443,-1.11679895468675,-5.46008704245614));
#20855=CARTESIAN_POINT('Ctrl Pts',(97.5673536947163,-1.07654585136958,-5.45714005319566));
#20856=CARTESIAN_POINT('Ctrl Pts',(97.605673592613,-1.03410967036203,-5.45419306393519));
#20857=CARTESIAN_POINT('Ctrl Pts',(97.6439560356009,-0.991714967630169,
-5.45124895514204));
#20858=CARTESIAN_POINT('Ctrl Pts',(97.6799260173105,-0.947141803429666,
-5.4483048463489));
#20859=CARTESIAN_POINT('Ctrl Pts',(97.7133301206631,-0.90067638722735,-5.44536073755575));
#20860=CARTESIAN_POINT('Ctrl Pts',(97.7467148424364,-0.854237930980674,
-5.44241833698022));
#20861=CARTESIAN_POINT('Ctrl Pts',(97.777536328314,-0.805909826724527,-5.43947593640469));
#20862=CARTESIAN_POINT('Ctrl Pts',(97.805582153967,-0.75601041656096,-5.43653353582916));
#20863=CARTESIAN_POINT('Ctrl Pts',(97.8336228464436,-0.706120139395519,
-5.43359167379585));
#20864=CARTESIAN_POINT('Ctrl Pts',(97.8588886290636,-0.654659588043249,
-5.43064981176254));
#20865=CARTESIAN_POINT('Ctrl Pts',(97.8812122520137,-0.60197306108882,-5.42770794972922));
#20866=CARTESIAN_POINT('Ctrl Pts',(97.9035559399446,-0.549239178283588,
-5.42476344348329));
#20867=CARTESIAN_POINT('Ctrl Pts',(97.9229519806668,-0.495277606861794,
-5.42181893723735));
#20868=CARTESIAN_POINT('Ctrl Pts',(97.9392813010349,-0.440452631423638,
-5.41887443099142));
#20869=CARTESIAN_POINT('Ctrl Pts',(97.9556183951784,-0.385601555876467,
-5.41592852297679));
#20870=CARTESIAN_POINT('Ctrl Pts',(97.9688857392088,-0.329886772435975,
-5.41298261496217));
#20871=CARTESIAN_POINT('Ctrl Pts',(97.9790150338574,-0.273684553599324,
-5.41003670694755));
#20872=CARTESIAN_POINT('Ctrl Pts',(97.9891624434043,-0.217381824557753,
-5.40708553056764));
#20873=CARTESIAN_POINT('Ctrl Pts',(97.9961605356595,-0.160590444823081,
-5.40413435418774));
#20874=CARTESIAN_POINT('Ctrl Pts',(97.9999928529454,-0.103692330415918,
-5.40118317780784));
#20875=CARTESIAN_POINT('Ctrl Pts',(98.0023280769435,-0.0690214427267606,
-5.39938487735651));
#20876=CARTESIAN_POINT('Ctrl Pts',(98.0034888467739,-0.0343109594795624,
-5.39758657690517));
#20877=CARTESIAN_POINT('Ctrl Pts',(98.0034809091236,0.000353326024288114,
-5.39578827645384));
#20878=CARTESIAN_POINT('Origin',(96.460480949577,-1.76391462320204E-15,
-7.60421172358872));
#20879=CARTESIAN_POINT('',(95.5205266553345,1.22365637526844,-6.21868058178697));
#20880=CARTESIAN_POINT('',(95.5205266553345,1.22365637526844,-6.17704955921195));
#20881=CARTESIAN_POINT('',(95.5205266553345,1.22365637526844,-7.60421172358872));
#20882=CARTESIAN_POINT('',(98.0034803814948,-0.00132404739565839,-6.39578827645092));
#20883=CARTESIAN_POINT('Ctrl Pts',(98.0034803814954,-0.0013240466246711,
-6.39578827641126));
#20884=CARTESIAN_POINT('Ctrl Pts',(98.0035294092285,0.0558112255743518,
-6.39284931489647));
#20885=CARTESIAN_POINT('Ctrl Pts',(98.000400664574,0.112996196184301,-6.38991035338168));
#20886=CARTESIAN_POINT('Ctrl Pts',(97.9941042309439,0.169848847065066,-6.38697139186689));
#20887=CARTESIAN_POINT('Ctrl Pts',(97.9878096391193,0.226684867654557,-6.3840332900444));
#20888=CARTESIAN_POINT('Ctrl Pts',(97.9783492542707,0.283188235566044,-6.3810951882219));
#20889=CARTESIAN_POINT('Ctrl Pts',(97.9657850465216,0.338981674610642,-6.37815708639941));
#20890=CARTESIAN_POINT('Ctrl Pts',(97.9528393442749,0.396469202962078,-6.37512977324732));
#20891=CARTESIAN_POINT('Ctrl Pts',(97.9365983367856,0.453202398648983,-6.37210246009523));
#20892=CARTESIAN_POINT('Ctrl Pts',(97.9171860160137,0.508782221994395,-6.36907514694314));
#20893=CARTESIAN_POINT('Ctrl Pts',(97.8983213792134,0.562793959857088,-6.36613324402663));
#20894=CARTESIAN_POINT('Ctrl Pts',(97.8764623091867,0.61571607736221,-6.36319134111012));
#20895=CARTESIAN_POINT('Ctrl Pts',(97.8517715838318,0.667202646154045,-6.36024943819362));
#20896=CARTESIAN_POINT('Ctrl Pts',(97.8260056153116,0.720931375935481,-6.35717941992374));
#20897=CARTESIAN_POINT('Ctrl Pts',(97.7971559708585,0.773096069312216,-6.35410940165386));
#20898=CARTESIAN_POINT('Ctrl Pts',(97.7654592242794,0.823335109511779,-6.35103938338398));
#20899=CARTESIAN_POINT('Ctrl Pts',(97.7337624777003,0.873574149711343,-6.3479693651141));
#20900=CARTESIAN_POINT('Ctrl Pts',(97.6992190724388,0.92188706063909,-6.34489934684422));
#20901=CARTESIAN_POINT('Ctrl Pts',(97.662112314353,0.967951994257261,-6.34182932857434));
#20902=CARTESIAN_POINT('Ctrl Pts',(97.6262157705618,1.01251454814676,-6.33885943707885));
#20903=CARTESIAN_POINT('Ctrl Pts',(97.5877611235107,1.0551717064333,-6.33588954558335));
#20904=CARTESIAN_POINT('Ctrl Pts',(97.5469782282762,1.09561519858899,-6.33291965408785));
#20905=CARTESIAN_POINT('Ctrl Pts',(97.5062689650265,1.13598567153943,-6.32995512461984));
#20906=CARTESIAN_POINT('Ctrl Pts',(97.4632401644032,1.17415004716957,-6.32699059515184));
#20907=CARTESIAN_POINT('Ctrl Pts',(97.4181615998277,1.20983336544144,-6.32402606568383));
#20908=CARTESIAN_POINT('Ctrl Pts',(97.3731285950243,1.24548061948056,-6.32106453239123));
#20909=CARTESIAN_POINT('Ctrl Pts',(97.3260503376017,1.27865146231512,-6.31810299909863));
#20910=CARTESIAN_POINT('Ctrl Pts',(97.2772317951421,1.30910926063057,-6.31514146580603));
#20911=CARTESIAN_POINT('Ctrl Pts',(97.22844377863,1.3395480138638,-6.31218178434279));
#20912=CARTESIAN_POINT('Ctrl Pts',(97.1779180757227,1.36727680997693,-6.30922210287954));
#20913=CARTESIAN_POINT('Ctrl Pts',(97.1259891167632,1.39210196444385,-6.3062624214163));
#20914=CARTESIAN_POINT('Ctrl Pts',(97.0740726173981,1.41692116247797,-6.30330345008535));
#20915=CARTESIAN_POINT('Ctrl Pts',(97.0207540006523,1.43883787713433,-6.30034447875439));
#20916=CARTESIAN_POINT('Ctrl Pts',(96.9663908171012,1.45770511625006,-6.29738550742343));
#20917=CARTESIAN_POINT('Ctrl Pts',(96.9119804370647,1.47658873533691,-6.29442396720232));
#20918=CARTESIAN_POINT('Ctrl Pts',(96.856524171388,1.4924174156804,-6.2914624269812));
#20919=CARTESIAN_POINT('Ctrl Pts',(96.8003966884087,1.5050934490903,-6.28850088676009));
#20920=CARTESIAN_POINT('Ctrl Pts',(96.7442465679591,1.5177745950282,-6.28553815208351));
#20921=CARTESIAN_POINT('Ctrl Pts',(96.6874252056233,1.52730047099368,-6.28257541740693));
#20922=CARTESIAN_POINT('Ctrl Pts',(96.6303162990154,1.53362477616956,-6.27961268273036));
#20923=CARTESIAN_POINT('Ctrl Pts',(96.5730994693102,1.53996103287181,-6.27664434914598));
#20924=CARTESIAN_POINT('Ctrl Pts',(96.5155945319472,1.54308359937165,-6.2736760155616));
#20925=CARTESIAN_POINT('Ctrl Pts',(96.4581881356583,1.54299829650079,-6.27070768197723));
#20926=CARTESIAN_POINT('Ctrl Pts',(96.4068499374961,1.54292201065162,-6.26805311893866));
#20927=CARTESIAN_POINT('Ctrl Pts',(96.3555908081535,1.54028094513122,-6.26539855590009));
#20928=CARTESIAN_POINT('Ctrl Pts',(96.304682680796,1.53511429523826,-6.26274399286152));
#20929=CARTESIAN_POINT('Ctrl Pts',(96.2476427768939,1.52932533326523,-6.259769693305));
#20930=CARTESIAN_POINT('Ctrl Pts',(96.1908111694043,1.52034130012038,-6.25679539374849));
#20931=CARTESIAN_POINT('Ctrl Pts',(96.134572654946,1.50818857689968,-6.25382109419198));
#20932=CARTESIAN_POINT('Ctrl Pts',(96.0784269630212,1.49605591193566,-6.25085170376265));
#20933=CARTESIAN_POINT('Ctrl Pts',(96.0228729253038,1.48076504427997,-6.24788231333332));
#20934=CARTESIAN_POINT('Ctrl Pts',(95.9682890204752,1.46239396365242,-6.24491292290399));
#20935=CARTESIAN_POINT('Ctrl Pts',(95.9137589250248,1.44404099342626,-6.24194645973047));
#20936=CARTESIAN_POINT('Ctrl Pts',(95.8601975568746,1.42261399382697,-6.23897999655696));
#20937=CARTESIAN_POINT('Ctrl Pts',(95.8079701860178,1.39824128942019,-6.23601353338344));
#20938=CARTESIAN_POINT('Ctrl Pts',(95.7557619845293,1.37387753069333,-6.23304815901114));
#20939=CARTESIAN_POINT('Ctrl Pts',(95.704887285087,1.34657041820749,-6.23008278463884));
#20940=CARTESIAN_POINT('Ctrl Pts',(95.6556914329275,1.31649642380486,-6.22711741026653));
#20941=CARTESIAN_POINT('Ctrl Pts',(95.6090354951532,1.28797510849305,-6.22430513410668));
#20942=CARTESIAN_POINT('Ctrl Pts',(95.5638897013052,1.25696579292471,-6.22149285794683));
#20943=CARTESIAN_POINT('Ctrl Pts',(95.5205266553345,1.22365637526844,-6.21868058178697));
#20944=CARTESIAN_POINT('',(96.8589947914343,-1.49064942821851,-6.49999999999999));
#20945=CARTESIAN_POINT('Ctrl Pts',(96.8589947914343,-1.4906494282185,-6.49999999999999));
#20946=CARTESIAN_POINT('Ctrl Pts',(96.915764516961,-1.47547247179094,-6.49696938050472));
#20947=CARTESIAN_POINT('Ctrl Pts',(96.9717164672414,-1.45703484475423,-6.49393876100945));
#20948=CARTESIAN_POINT('Ctrl Pts',(97.0264642179596,-1.43544834108058,-6.49090814151418));
#20949=CARTESIAN_POINT('Ctrl Pts',(97.0811796713535,-1.41387457192662,-6.48787930987136));
#20950=CARTESIAN_POINT('Ctrl Pts',(97.1346918794132,-1.38915579118626,-6.48485047822855));
#20951=CARTESIAN_POINT('Ctrl Pts',(97.1866316757174,-1.36145294554228,-6.48182164658573));
#20952=CARTESIAN_POINT('Ctrl Pts',(97.2385557247662,-1.33375849892596,-6.47879373323272));
#20953=CARTESIAN_POINT('Ctrl Pts',(97.2889078761591,-1.30308201422557,-6.47576581987971));
#20954=CARTESIAN_POINT('Ctrl Pts',(97.3373426670593,-1.26963086305194,-6.4727379065267));
#20955=CARTESIAN_POINT('Ctrl Pts',(97.3857779905807,-1.23617934402719,-6.46970995987674));
#20956=CARTESIAN_POINT('Ctrl Pts',(97.432295508573,-1.19995337703009,-6.46668201322678));
#20957=CARTESIAN_POINT('Ctrl Pts',(97.4765794454682,-1.16120318921698,-6.46365406657682));
#20958=CARTESIAN_POINT('Ctrl Pts',(97.5208777825532,-1.12244040067102,-6.46062513530333));
#20959=CARTESIAN_POINT('Ctrl Pts',(97.5629407278518,-1.08115208480294,-6.45759620402984));
#20960=CARTESIAN_POINT('Ctrl Pts',(97.6024876336847,-1.03762697220795,-6.45456727275634));
#20961=CARTESIAN_POINT('Ctrl Pts',(97.6420930678142,-0.994037443683377,
-6.45153385875065));
#20962=CARTESIAN_POINT('Ctrl Pts',(97.6791746980187,-0.948204873361764,
-6.44850044474496));
#20963=CARTESIAN_POINT('Ctrl Pts',(97.7134912103065,-0.900452267755797,
-6.44546703073927));
#20964=CARTESIAN_POINT('Ctrl Pts',(97.7478340052991,-0.852663088863378,
-6.44243129346937));
#20965=CARTESIAN_POINT('Ctrl Pts',(97.7794072000822,-0.802951359379204,
-6.43939555619948));
#20966=CARTESIAN_POINT('Ctrl Pts',(97.8080137200766,-0.751667767321239,
-6.43635981892958));
#20967=CARTESIAN_POINT('Ctrl Pts',(97.8366807930495,-0.700275620491613,
-6.43331765574931));
#20968=CARTESIAN_POINT('Ctrl Pts',(97.8623684296765,-0.64730540536536,-6.43027549256904));
#20969=CARTESIAN_POINT('Ctrl Pts',(97.8849265505216,-0.59313044935296,-6.42723332938877));
#20970=CARTESIAN_POINT('Ctrl Pts',(97.9005445173536,-0.555622774314743,
-6.42512710768823));
#20971=CARTESIAN_POINT('Ctrl Pts',(97.9146633972451,-0.51753805012281,-6.4230208859877));
#20972=CARTESIAN_POINT('Ctrl Pts',(97.9272474852871,-0.479004101987811,
-6.42091466428717));
#20973=CARTESIAN_POINT('Ctrl Pts',(97.9479486403942,-0.415614745955782,
-6.41744987431055));
#20974=CARTESIAN_POINT('Ctrl Pts',(97.9645639136385,-0.350798124206962,
-6.41398508433394));
#20975=CARTESIAN_POINT('Ctrl Pts',(97.9769231303583,-0.285047561553121,
-6.41052029435732));
#20976=CARTESIAN_POINT('Ctrl Pts',(97.9891473600444,-0.220015124781231,
-6.40709334672391));
#20977=CARTESIAN_POINT('Ctrl Pts',(97.9972078859358,-0.154069184982509,
-6.4036663990905));
#20978=CARTESIAN_POINT('Ctrl Pts',(98.0009861219586,-0.0877086875140339,
-6.40023945145709));
#20979=CARTESIAN_POINT('Ctrl Pts',(98.0026219401416,-0.0589773674661508,
-6.39875572645503));
#20980=CARTESIAN_POINT('Ctrl Pts',(98.0034556299914,-0.0301686006272956,
-6.39727200145298));
#20981=CARTESIAN_POINT('Ctrl Pts',(98.0034803814948,-0.00132404739565834,
-6.39578827645092));
#20982=CARTESIAN_POINT('',(96.0617145053845,-1.49058187396268,-6.49999996996503));
#20983=CARTESIAN_POINT('Origin',(96.460480949577,-1.62868768791465E-15,
-6.49999999999999));
#20984=CARTESIAN_POINT('',(98.0034806316228,0.000990558803381491,-6.35421172362388));
#20985=CARTESIAN_POINT('Ctrl Pts',(96.0617145053845,-1.49058187396268,-6.49999996996503));
#20986=CARTESIAN_POINT('Ctrl Pts',(96.116690584544,-1.50528929526237,-6.49704678467027));
#20987=CARTESIAN_POINT('Ctrl Pts',(96.1726030058333,-1.51698360757519,-6.49409359937551));
#20988=CARTESIAN_POINT('Ctrl Pts',(96.229088163052,-1.5255511719848,-6.49114041408075));
#20989=CARTESIAN_POINT('Ctrl Pts',(96.2854728766418,-1.53410350129014,-6.48819248023013));
#20990=CARTESIAN_POINT('Ctrl Pts',(96.3424277877649,-1.53954003633601,-6.48524454637951));
#20991=CARTESIAN_POINT('Ctrl Pts',(96.3995765076143,-1.54179753824853,-6.48229661252888));
#20992=CARTESIAN_POINT('Ctrl Pts',(96.4566688759794,-1.54405281415171,-6.47935158548787));
#20993=CARTESIAN_POINT('Ctrl Pts',(96.5139541496305,-1.54313524452192,-6.47640655844686));
#20994=CARTESIAN_POINT('Ctrl Pts',(96.5710500339397,-1.53903329320168,-6.47346153140585));
#20995=CARTESIAN_POINT('Ctrl Pts',(96.6281122636852,-1.53493375973315,-6.4705182402798));
#20996=CARTESIAN_POINT('Ctrl Pts',(96.6849847996598,-1.52765360202188,-6.46757494915375));
#20997=CARTESIAN_POINT('Ctrl Pts',(96.7412868843653,-1.51723334625485,-6.46463165802771));
#20998=CARTESIAN_POINT('Ctrl Pts',(96.7975781110642,-1.50681510006181,-6.46168893452317));
#20999=CARTESIAN_POINT('Ctrl Pts',(96.8532985860008,-1.49325805459338,-6.45874621101863));
#21000=CARTESIAN_POINT('Ctrl Pts',(96.9080765059447,-1.47665406169484,-6.45580348751409));
#21001=CARTESIAN_POINT('Ctrl Pts',(96.962903420947,-1.46003521767378,-6.45285813194704));
#21002=CARTESIAN_POINT('Ctrl Pts',(97.0167855908051,-1.44036413669594,-6.44991277637998));
#21003=CARTESIAN_POINT('Ctrl Pts',(97.0693666645714,-1.41778248898616,-6.44696742081293));
#21004=CARTESIAN_POINT('Ctrl Pts',(97.1219722445091,-1.39519031677222,-6.44402069252023));
#21005=CARTESIAN_POINT('Ctrl Pts',(97.1732750471856,-1.36968511148393,-6.44107396422753));
#21006=CARTESIAN_POINT('Ctrl Pts',(97.2229419852295,-1.34145524305203,-6.43812723593483));
#21007=CARTESIAN_POINT('Ctrl Pts',(97.2726985259559,-1.31317444593322,-6.43517519153508));
#21008=CARTESIAN_POINT('Ctrl Pts',(97.3208128653744,-1.28215945799747,-6.43222314713533));
#21009=CARTESIAN_POINT('Ctrl Pts',(97.3669807123812,-1.2486421344949,-6.42927110273557));
#21010=CARTESIAN_POINT('Ctrl Pts',(97.3968781136849,-1.22693696658367,-6.42735941610066));
#21011=CARTESIAN_POINT('Ctrl Pts',(97.4259598757987,-1.2041832735016,-6.42544772946574));
#21012=CARTESIAN_POINT('Ctrl Pts',(97.4541514013328,-1.18045246973672,-6.42353604283083));
#21013=CARTESIAN_POINT('Ctrl Pts',(97.497390358046,-1.14405517738296,-6.42060397959229));
#21014=CARTESIAN_POINT('Ctrl Pts',(97.5387259925091,-1.10519533681692,-6.41767191635376));
#21015=CARTESIAN_POINT('Ctrl Pts',(97.577859829369,-1.06410217507283,-6.41473985311523));
#21016=CARTESIAN_POINT('Ctrl Pts',(97.6169405909014,-1.02306474599376,-6.41181176649206));
#21017=CARTESIAN_POINT('Ctrl Pts',(97.6538250987265,-0.979800374259077,
-6.4088836798689));
#21018=CARTESIAN_POINT('Ctrl Pts',(97.6882484389171,-0.934577975408972,
-6.40595559324573));
#21019=CARTESIAN_POINT('Ctrl Pts',(97.7226391559366,-0.889398434051653,
-6.40303028158485));
#21020=CARTESIAN_POINT('Ctrl Pts',(97.7545730006852,-0.842264963907663,
-6.40010496992396));
#21021=CARTESIAN_POINT('Ctrl Pts',(97.7838240659667,-0.793480936320484,
-6.39717965826308));
#21022=CARTESIAN_POINT('Ctrl Pts',(97.8130593554045,-0.744723219200589,
-6.39425592429721));
#21023=CARTESIAN_POINT('Ctrl Pts',(97.8396144577919,-0.69431716737565,-6.39133219033133));
#21024=CARTESIAN_POINT('Ctrl Pts',(97.8633070811437,-0.642594619175778,
-6.38840845636546));
#21025=CARTESIAN_POINT('Ctrl Pts',(97.8870109123206,-0.590847603559806,
-6.38548333932357));
#21026=CARTESIAN_POINT('Ctrl Pts',(97.9078493244683,-0.537783329902571,
-6.38255822228169));
#21027=CARTESIAN_POINT('Ctrl Pts',(97.9256870770652,-0.483756141016263,
-6.37963310523981));
#21028=CARTESIAN_POINT('Ctrl Pts',(97.9435281104811,-0.429719015147953,
-6.37670745019408));
#21029=CARTESIAN_POINT('Ctrl Pts',(97.9583672355104,-0.374719136651115,
-6.37378179514835));
#21030=CARTESIAN_POINT('Ctrl Pts',(97.9701192774561,-0.319125553659244,
-6.37085614010262));
#21031=CARTESIAN_POINT('Ctrl Pts',(97.9818901361726,-0.26344295705512,-6.36792580064712));
#21032=CARTESIAN_POINT('Ctrl Pts',(97.9905639489311,-0.207165286916391,
-6.36499546119161));
#21033=CARTESIAN_POINT('Ctrl Pts',(97.9961070578707,-0.150670021991439,
-6.3620651217361));
#21034=CARTESIAN_POINT('Ctrl Pts',(98.0010589575786,-0.100200350741447,
-6.35944732236536));
#21035=CARTESIAN_POINT('Ctrl Pts',(98.0035130818555,-0.0495573729400543,
-6.35682952299462));
#21036=CARTESIAN_POINT('Ctrl Pts',(98.0034806316228,0.000990558803380336,
-6.35421172362388));
#21037=CARTESIAN_POINT('Ctrl Pts',(98.0034806316223,0.000990559482311531,
-6.35421172358872));
#21038=CARTESIAN_POINT('Ctrl Pts',(98.0034402990849,0.0638167637889655,
-6.35095805143181));
#21039=CARTESIAN_POINT('Ctrl Pts',(97.9995628740167,0.126518520347403,-6.34770437927491));
#21040=CARTESIAN_POINT('Ctrl Pts',(97.9918933276673,0.188746200575634,-6.34445070711801));
#21041=CARTESIAN_POINT('Ctrl Pts',(97.984897247495,0.245509641329849,-6.34148274131831));
#21042=CARTESIAN_POINT('Ctrl Pts',(97.9747261260543,0.302003370910422,-6.33851477551861));
#21043=CARTESIAN_POINT('Ctrl Pts',(97.9614127380147,0.357844612167181,-6.33554680971891));
#21044=CARTESIAN_POINT('Ctrl Pts',(97.9481230811933,0.413586315975266,-6.33258413434143));
#21045=CARTESIAN_POINT('Ctrl Pts',(97.9317023948098,0.468677336106132,-6.32962145896395));
#21046=CARTESIAN_POINT('Ctrl Pts',(97.9122349375888,0.522742152778854,-6.32665878358647));
#21047=CARTESIAN_POINT('Ctrl Pts',(97.8927868733996,0.576753111328393,-6.32369905955785));
#21048=CARTESIAN_POINT('Ctrl Pts',(97.8702982275636,0.629739402907963,-6.32073933552924));
#21049=CARTESIAN_POINT('Ctrl Pts',(97.844903368191,0.681339538584773,-6.31777961150063));
#21050=CARTESIAN_POINT('Ctrl Pts',(97.8195239884064,0.732908221091223,-6.31482169158944));
#21051=CARTESIAN_POINT('Ctrl Pts',(97.7912421366924,0.783091954952207,-6.31186377167826));
#21052=CARTESIAN_POINT('Ctrl Pts',(97.7602398503536,0.831550238922453,-6.30890585176707));
#21053=CARTESIAN_POINT('Ctrl Pts',(97.7292444761241,0.879997718884657,-6.30594859133839));
#21054=CARTESIAN_POINT('Ctrl Pts',(97.6955301527396,0.92672007303637,-6.30299133090971));
#21055=CARTESIAN_POINT('Ctrl Pts',(97.6593231617635,0.971404318643746,-6.30003407048103));
#21056=CARTESIAN_POINT('Ctrl Pts',(97.6230835810073,1.01612878437716,-6.29707414823306));
#21057=CARTESIAN_POINT('Ctrl Pts',(97.5843471780464,1.05881106844031,-6.29411422598508));
#21058=CARTESIAN_POINT('Ctrl Pts',(97.5433807445106,1.09917106681933,-6.2911543037371));
#21059=CARTESIAN_POINT('Ctrl Pts',(97.5023971101579,1.13954801138771,-6.2881931386892));
#21060=CARTESIAN_POINT('Ctrl Pts',(97.4591819707229,1.17760037988561,-6.2852319736413));
#21061=CARTESIAN_POINT('Ctrl Pts',(97.4140368499147,1.21308703106216,-6.2822708085934));
#21062=CARTESIAN_POINT('Ctrl Pts',(97.3688048204051,1.24864199745671,-6.27930394301787));
#21063=CARTESIAN_POINT('Ctrl Pts',(97.32163581439,1.28162107604611,-6.27633707744233));
#21064=CARTESIAN_POINT('Ctrl Pts',(97.2728613021965,1.3118258888579,-6.27337021186679));
#21065=CARTESIAN_POINT('Ctrl Pts',(97.2289954580633,1.33899088859419,-6.27070193171292));
#21066=CARTESIAN_POINT('Ctrl Pts',(97.1838316157734,1.36391240691739,-6.26803365155905));
#21067=CARTESIAN_POINT('Ctrl Pts',(97.1376256759733,1.38647900074749,-6.26536537140518));
#21068=CARTESIAN_POINT('Ctrl Pts',(97.0861889261889,1.41160027834394,-6.26239502475228));
#21069=CARTESIAN_POINT('Ctrl Pts',(97.0332453252879,1.43390757435751,-6.25942467809939));
#21070=CARTESIAN_POINT('Ctrl Pts',(96.9791343172436,1.45321976459452,-6.25645433144649));
#21071=CARTESIAN_POINT('Ctrl Pts',(96.9251189641295,1.47249781563735,-6.25348923563464));
#21072=CARTESIAN_POINT('Ctrl Pts',(96.8699407869667,1.48879109626221,-6.25052413982279));
#21073=CARTESIAN_POINT('Ctrl Pts',(96.8139611609895,1.50196562548541,-6.24755904401093));
#21074=CARTESIAN_POINT('Ctrl Pts',(96.7580368325766,1.51512714069926,-6.24459687716785));
#21075=CARTESIAN_POINT('Ctrl Pts',(96.7013131288064,1.52517588971202,-6.24163471032476));
#21076=CARTESIAN_POINT('Ctrl Pts',(96.6441669333127,1.53202756482351,-6.23867254348168));
#21077=CARTESIAN_POINT('Ctrl Pts',(96.5870551945963,1.53887510866009,-6.23571216270191));
#21078=CARTESIAN_POINT('Ctrl Pts',(96.5295219856489,1.54252933805977,-6.23275178192214));
#21079=CARTESIAN_POINT('Ctrl Pts',(96.4719525472493,1.542957356004,-6.22979140114237));
#21080=CARTESIAN_POINT('Ctrl Pts',(96.4143956660283,1.54338528058796,-6.22683166608768));
#21081=CARTESIAN_POINT('Ctrl Pts',(96.3568030920146,1.540588387079,-6.22387193103298));
#21082=CARTESIAN_POINT('Ctrl Pts',(96.299561093711,1.53458587247116,-6.22091219597828));
#21083=CARTESIAN_POINT('Ctrl Pts',(96.2422675842191,1.52857795629333,-6.21794979750382));
#21084=CARTESIAN_POINT('Ctrl Pts',(96.1853258005499,1.5193587082637,-6.21498739902936));
#21085=CARTESIAN_POINT('Ctrl Pts',(96.1291165203249,1.50699920870132,-6.2120250005549));
#21086=CARTESIAN_POINT('Ctrl Pts',(96.072883566014,1.49463450359544,-6.20906135438476));
#21087=CARTESIAN_POINT('Ctrl Pts',(96.0173842335257,1.47912704977739,-6.20609770821463));
#21088=CARTESIAN_POINT('Ctrl Pts',(95.9629855749006,1.46059828569512,-6.20313406204449));
#21089=CARTESIAN_POINT('Ctrl Pts',(95.9084827210883,1.44203403161937,-6.20016473930668));
#21090=CARTESIAN_POINT('Ctrl Pts',(95.855085238972,1.42043709890194,-6.19719541656887));
#21091=CARTESIAN_POINT('Ctrl Pts',(95.8031406644171,1.39597734562772,-6.19422609383106));
#21092=CARTESIAN_POINT('Ctrl Pts',(95.756805226356,1.37415883248101,-6.19157740778482));
#21093=CARTESIAN_POINT('Ctrl Pts',(95.7116257642638,1.35006318764398,-6.18892872173859));
#21094=CARTESIAN_POINT('Ctrl Pts',(95.6678300253879,1.32384044068091,-6.18628003569235));
#21095=CARTESIAN_POINT('Ctrl Pts',(95.6169550468038,1.29337899113337,-6.18320321019889));
#21096=CARTESIAN_POINT('Ctrl Pts',(95.5677292674599,1.25991516398024,-6.18012638470542));
#21097=CARTESIAN_POINT('Ctrl Pts',(95.5205266553345,1.22365637526844,-6.17704955921195));
#21098=CARTESIAN_POINT('Origin',(96.460480949577,-1.62868768791465E-15,
-6.49999999999999));
#21099=CARTESIAN_POINT('',(96.0195573809006,-1.18513571230711,-5.34780246104806));
#21100=CARTESIAN_POINT('',(96.0195573765031,-1.18513571067102,-5.20989040793544));
#21101=CARTESIAN_POINT('',(96.0195573765031,-1.18513571067102,-6.49999999999999));
#21102=CARTESIAN_POINT('',(97.7249794730849,-0.00193236804568257,-5.05658136948322));
#21103=CARTESIAN_POINT('Ctrl Pts',(96.019557376503,-1.18513571067102,-5.20989040793544));
#21104=CARTESIAN_POINT('Ctrl Pts',(96.0659867832952,-1.20240952982453,-5.20677992089892));
#21105=CARTESIAN_POINT('Ctrl Pts',(96.1134623860598,-1.21696187683096,-5.20366943386241));
#21106=CARTESIAN_POINT('Ctrl Pts',(96.1616345923433,-1.22867860108661,-5.20055894682589));
#21107=CARTESIAN_POINT('Ctrl Pts',(96.2097989355969,-1.24039341285038,-5.19744896750647));
#21108=CARTESIAN_POINT('Ctrl Pts',(96.2586591240462,-1.24927339216687,-5.19433898818704));
#21109=CARTESIAN_POINT('Ctrl Pts',(96.3078529130282,-1.25525492727942,-5.19122900886762));
#21110=CARTESIAN_POINT('Ctrl Pts',(96.3570953780928,-1.2612423809785,-5.18811595229773));
#21111=CARTESIAN_POINT('Ctrl Pts',(96.4066715574073,-1.26432559872759,-5.18500289572785));
#21112=CARTESIAN_POINT('Ctrl Pts',(96.4562133814324,-1.26449279865966,-5.18188983915796));
#21113=CARTESIAN_POINT('Ctrl Pts',(96.5057819011462,-1.26466008868767,-5.17877510511271));
#21114=CARTESIAN_POINT('Ctrl Pts',(96.5553154807588,-1.2619082622699,-5.17566037106747));
#21115=CARTESIAN_POINT('Ctrl Pts',(96.6044489378048,-1.25627762392141,-5.17254563702222));
#21116=CARTESIAN_POINT('Ctrl Pts',(96.6536755227132,-1.25063631322573,-5.16942499929055));
#21117=CARTESIAN_POINT('Ctrl Pts',(96.7024999308461,-1.24210539354816,-5.16630436155888));
#21118=CARTESIAN_POINT('Ctrl Pts',(96.7505665543627,-1.23077641832143,-5.16318372382721));
#21119=CARTESIAN_POINT('Ctrl Pts',(96.7763049368317,-1.22471005717443,-5.16151270636002));
#21120=CARTESIAN_POINT('Ctrl Pts',(96.801826286488,-1.21784226493739,-5.15984168889283));
#21121=CARTESIAN_POINT('Ctrl Pts',(96.8270781716263,-1.21019284694042,-5.15817067142564));
#21122=CARTESIAN_POINT('Ctrl Pts',(96.8739312376288,-1.19599989919293,-5.15507021808312));
#21123=CARTESIAN_POINT('Ctrl Pts',(96.9200694895639,-1.17904840191129,-5.15196976474061));
#21124=CARTESIAN_POINT('Ctrl Pts',(96.9651428358136,-1.15942944182909,-5.1488693113981));
#21125=CARTESIAN_POINT('Ctrl Pts',(97.0101340164064,-1.13984624578211,-5.145774509972));
#21126=CARTESIAN_POINT('Ctrl Pts',(97.0540636334913,-1.11760544580946,-5.1426797085459));
#21127=CARTESIAN_POINT('Ctrl Pts',(97.0965975601529,-1.09284761414818,-5.13958490711981));
#21128=CARTESIAN_POINT('Ctrl Pts',(97.1390890137287,-1.06811450490481,-5.13649319606832));
#21129=CARTESIAN_POINT('Ctrl Pts',(97.1801870556191,-1.04086961515804,-5.13340148501682));
#21130=CARTESIAN_POINT('Ctrl Pts',(97.2195804340792,-1.0113002633385,-5.13030977396533));
#21131=CARTESIAN_POINT('Ctrl Pts',(97.2589518291673,-0.981747412618484,
-5.12721978823511));
#21132=CARTESIAN_POINT('Ctrl Pts',(97.2966200000278,-0.949873001577503,
-5.12412980250489));
#21133=CARTESIAN_POINT('Ctrl Pts',(97.3323033642146,-0.915907160871423,
-5.12103981677467));
#21134=CARTESIAN_POINT('Ctrl Pts',(97.3679825338018,-0.881945312869059,
-5.11795019427402));
#21135=CARTESIAN_POINT('Ctrl Pts',(97.4016769579563,-0.845892907767278,
-5.11486057177336));
#21136=CARTESIAN_POINT('Ctrl Pts',(97.4331408293932,-0.808017950416858,
-5.11177094927271));
#21137=CARTESIAN_POINT('Ctrl Pts',(97.46463910441,-0.770101579404974,-5.1086779484823));
#21138=CARTESIAN_POINT('Ctrl Pts',(97.4939016034476,-0.730359108388724,
-5.10558494769189));
#21139=CARTESIAN_POINT('Ctrl Pts',(97.520723106248,-0.689091299624146,-5.10249194690149));
#21140=CARTESIAN_POINT('Ctrl Pts',(97.5475607781688,-0.647798612903396,
-5.09939708152121));
#21141=CARTESIAN_POINT('Ctrl Pts',(97.5719542521659,-0.604979243727851,
-5.09630221614094));
#21142=CARTESIAN_POINT('Ctrl Pts',(97.593743870321,-0.560959359015282,-5.09320735076066));
#21143=CARTESIAN_POINT('Ctrl Pts',(97.6155773230675,-0.516850918658907,
-5.09010625938052));
#21144=CARTESIAN_POINT('Ctrl Pts',(97.6347962528238,-0.471537656915443,
-5.08700516800038));
#21145=CARTESIAN_POINT('Ctrl Pts',(97.65128945544,-0.425364963724596,-5.08390407662024));
#21146=CARTESIAN_POINT('Ctrl Pts',(97.6598323048649,-0.401449271020396,
-5.0822978296511));
#21147=CARTESIAN_POINT('Ctrl Pts',(97.6676447099899,-0.377303239195462,
-5.08069158268195));
#21148=CARTESIAN_POINT('Ctrl Pts',(97.6747166060384,-0.35297594900736,-5.07908533571281));
#21149=CARTESIAN_POINT('Ctrl Pts',(97.6926205914113,-0.291386320893395,
-5.07501878523703));
#21150=CARTESIAN_POINT('Ctrl Pts',(97.705839977151,-0.22841490933399,-5.07095223476125));
#21151=CARTESIAN_POINT('Ctrl Pts',(97.7142116855971,-0.164679967083339,
-5.06688568428547));
#21152=CARTESIAN_POINT('Ctrl Pts',(97.7212827662567,-0.110846879083575,
-5.06345091268472));
#21153=CARTESIAN_POINT('Ctrl Pts',(97.7248961315897,-0.0564691825175074,
-5.06001614108397));
#21154=CARTESIAN_POINT('Ctrl Pts',(97.7249794730849,-0.00193236804568257,
-5.05658136948322));
#21155=CARTESIAN_POINT('',(97.4185971022994,0.825211298936501,-4.99999999999999));
#21156=CARTESIAN_POINT('Ctrl Pts',(97.7249794131076,-0.0019712252134486,
-5.05599185435273));
#21157=CARTESIAN_POINT('Ctrl Pts',(97.7250886418092,0.0680966313148683,
-5.05116780817991));
#21158=CARTESIAN_POINT('Ctrl Pts',(97.7193739476589,0.138060871914648,-5.04642730973536));
#21159=CARTESIAN_POINT('Ctrl Pts',(97.7015947191016,0.245097279283364,-5.03934388598835));
#21160=CARTESIAN_POINT('Ctrl Pts',(97.6935756686832,0.282690592057035,-5.03688714426543));
#21161=CARTESIAN_POINT('Ctrl Pts',(97.6733133589011,0.360187379727602,-5.0318677559316));
#21162=CARTESIAN_POINT('Ctrl Pts',(97.6607824801873,0.399967703886956,-5.0293170680671));
#21163=CARTESIAN_POINT('Ctrl Pts',(97.6293133272092,0.484960679704296,-5.02386746605508));
#21164=CARTESIAN_POINT('Ctrl Pts',(97.6096667059248,0.529838199790481,-5.02099038870329));
#21165=CARTESIAN_POINT('Ctrl Pts',(97.5529429615142,0.641312849549861,-5.01367877086113));
#21166=CARTESIAN_POINT('Ctrl Pts',(97.5123652844107,0.705898724599613,-5.00928432305277));
#21167=CARTESIAN_POINT('Ctrl Pts',(97.4509415607018,0.786501315358406,-5.00314001166332));
#21168=CARTESIAN_POINT('Ctrl Pts',(97.4350564634794,0.80610106640531,-5.00158722299082));
#21169=CARTESIAN_POINT('Ctrl Pts',(97.4185971022994,0.825211298936494,-4.99999999999999));
#21170=CARTESIAN_POINT('',(95.5154707437297,0.840188050881734,-4.99999999999999));
#21171=CARTESIAN_POINT('Origin',(96.460480949577,-1.44499066804254E-15,
-4.99999999999999));
#21172=CARTESIAN_POINT('Ctrl Pts',(95.5154707437297,0.840188050881728,-5.00000000000008));
#21173=CARTESIAN_POINT('Ctrl Pts',(95.5225653642979,0.848167798792328,-5.00069948174956));
#21174=CARTESIAN_POINT('Ctrl Pts',(95.5297607391518,0.856057327215644,-5.00140476782242));
#21175=CARTESIAN_POINT('Ctrl Pts',(95.6012645399553,0.932492002900971,-5.00836574119585));
#21176=CARTESIAN_POINT('Ctrl Pts',(95.6729242985494,0.993754826969376,-5.01494261410443));
#21177=CARTESIAN_POINT('Ctrl Pts',(95.8008995005763,1.08055089023169,-5.02546961385795));
#21178=CARTESIAN_POINT('Ctrl Pts',(95.8534778851055,1.11093969294436,-5.02951681756359));
#21179=CARTESIAN_POINT('Ctrl Pts',(95.9394869817854,1.15271315299406,-5.03568910567018));
#21180=CARTESIAN_POINT('Ctrl Pts',(95.9715545445553,1.16667634308418,-5.03790068992543));
#21181=CARTESIAN_POINT('Ctrl Pts',(96.041998665254,1.19393414997956,-5.04258437551926));
#21182=CARTESIAN_POINT('Ctrl Pts',(96.080520081999,1.20674621808099,-5.04503831417902));
#21183=CARTESIAN_POINT('Ctrl Pts',(96.213858882752,1.24407395621109,-5.05325544409173));
#21184=CARTESIAN_POINT('Ctrl Pts',(96.310864231887,1.25942725862804,-5.05874252092699));
#21185=CARTESIAN_POINT('Ctrl Pts',(96.440525397292,1.26474445598386,-5.06628278241473));
#21186=CARTESIAN_POINT('Ctrl Pts',(96.4724174834013,1.26484545460788,-5.0681567189018));
#21187=CARTESIAN_POINT('Ctrl Pts',(96.529406746253,1.26287043739154,-5.07159134821271));
#21188=CARTESIAN_POINT('Ctrl Pts',(96.5545027279978,1.26125025259789,-5.07313385778599));
#21189=CARTESIAN_POINT('Ctrl Pts',(96.6011390478585,1.25683992959629,-5.07608386292141));
#21190=CARTESIAN_POINT('Ctrl Pts',(96.6226871690055,1.25424088503172,-5.07748205493465));
#21191=CARTESIAN_POINT('Ctrl Pts',(96.7472870107203,1.23594820818855,-5.08573551993887));
#21192=CARTESIAN_POINT('Ctrl Pts',(96.8481467377453,1.20811437538997,-5.09304584406037));
#21193=CARTESIAN_POINT('Ctrl Pts',(96.9843978543938,1.15166901369871,-5.10307174950027));
#21194=CARTESIAN_POINT('Ctrl Pts',(97.0234783199235,1.13307766806414,-5.1059724254529));
#21195=CARTESIAN_POINT('Ctrl Pts',(97.095312182274,1.09426856446604,-5.11133259843523));
#21196=CARTESIAN_POINT('Ctrl Pts',(97.1282458624499,1.07448821477941,-5.11380250988762));
#21197=CARTESIAN_POINT('Ctrl Pts',(97.1898933542052,1.03353083741832,-5.11845965731787));
#21198=CARTESIAN_POINT('Ctrl Pts',(97.2187116403285,1.01257842015142,-5.12065238746011));
#21199=CARTESIAN_POINT('Ctrl Pts',(97.309501894184,0.940516391970181,-5.12765366954388));
#21200=CARTESIAN_POINT('Ctrl Pts',(97.3674990342575,0.884718984450137,-5.13226403185193));
#21201=CARTESIAN_POINT('Ctrl Pts',(97.4545673120993,0.783324805870413,-5.13991283324053));
#21202=CARTESIAN_POINT('Ctrl Pts',(97.4867201248125,0.74070102000269,-5.14295588062998));
#21203=CARTESIAN_POINT('Ctrl Pts',(97.5348262778599,0.667758395396185,-5.14809815860554));
#21204=CARTESIAN_POINT('Ctrl Pts',(97.5524116952355,0.638596875353117,-5.15013905273329));
#21205=CARTESIAN_POINT('Ctrl Pts',(97.5784666262472,0.591161262615176,-5.15349297607473));
#21206=CARTESIAN_POINT('Ctrl Pts',(97.5877128783719,0.573333833101893,-5.15476225805567));
#21207=CARTESIAN_POINT('Ctrl Pts',(97.6100278594998,0.527680517658497,-5.15803964687414));
#21208=CARTESIAN_POINT('Ctrl Pts',(97.6225120280938,0.49958808510192,-5.16007661248045));
#21209=CARTESIAN_POINT('Ctrl Pts',(97.6659179821178,0.391460251440093,-5.16792017719288));
#21210=CARTESIAN_POINT('Ctrl Pts',(97.6896921504058,0.308804017477303,-5.17390485661856));
#21211=CARTESIAN_POINT('Ctrl Pts',(97.7123961087576,0.182883262210213,-5.18259731786388));
#21212=CARTESIAN_POINT('Ctrl Pts',(97.7177980508486,0.141039475040924,-5.18542213923926));
#21213=CARTESIAN_POINT('Ctrl Pts',(97.7240536048506,0.0613846348084678,
-5.19066241450169));
#21214=CARTESIAN_POINT('Ctrl Pts',(97.7253228300527,0.0236525481661949,
-5.1930872464048));
#21215=CARTESIAN_POINT('Ctrl Pts',(97.724508896298,-0.049423421546514,-5.19768168968038));
#21216=CARTESIAN_POINT('Ctrl Pts',(97.722633830023,-0.0847337891276406,
-5.199855764321));
#21217=CARTESIAN_POINT('Ctrl Pts',(97.7116857605549,-0.19965364530648,-5.20682154140594));
#21218=CARTESIAN_POINT('Ctrl Pts',(97.6965321583009,-0.27848573892177,-5.21141410574877));
#21219=CARTESIAN_POINT('Ctrl Pts',(97.6590052371654,-0.406638089032292,
-5.2190452990109));
#21220=CARTESIAN_POINT('Ctrl Pts',(97.6407558255838,-0.456908756842203,
-5.22208874196325));
#21221=CARTESIAN_POINT('Ctrl Pts',(97.6057743355483,-0.537047928321703,
-5.22722850472882));
#21222=CARTESIAN_POINT('Ctrl Pts',(97.5909142954068,-0.567659607035057,
-5.22926569331807));
#21223=CARTESIAN_POINT('Ctrl Pts',(97.5653842407371,-0.615263561106463,
-5.23261055451799));
#21224=CARTESIAN_POINT('Ctrl Pts',(97.5555133475847,-0.632664578468388,
-5.23387410625749));
#21225=CARTESIAN_POINT('Ctrl Pts',(97.5296039548488,-0.675915083501862,
-5.23712341030891));
#21226=CARTESIAN_POINT('Ctrl Pts',(97.5130399457795,-0.701430270279938,
-5.23913720139458));
#21227=CARTESIAN_POINT('Ctrl Pts',(97.4463125762333,-0.796524620269645,
-5.24695058384691));
#21228=CARTESIAN_POINT('Ctrl Pts',(97.3900374604782,-0.861533870346743,
-5.25293176224602));
#21229=CARTESIAN_POINT('Ctrl Pts',(97.2966549355382,-0.949517074658011,
-5.2616499081229));
#21230=CARTESIAN_POINT('Ctrl Pts',(97.2642409619749,-0.97710799575487,-5.264500792442));
#21231=CARTESIAN_POINT('Ctrl Pts',(97.2003540777347,-1.0261539395934,-5.26978474217415));
#21232=CARTESIAN_POINT('Ctrl Pts',(97.1691831023805,-1.04792457598888,-5.27222743626958));
#21233=CARTESIAN_POINT('Ctrl Pts',(97.1070407871836,-1.08728313143618,-5.276853122785));
#21234=CARTESIAN_POINT('Ctrl Pts',(97.0762148323405,-1.10503230963672,-5.27904070096637));
#21235=CARTESIAN_POINT('Ctrl Pts',(96.9894653531937,-1.1502224079078,-5.28494476461941));
#21236=CARTESIAN_POINT('Ctrl Pts',(96.9322000730558,-1.17486949744465,-5.28856368211066));
#21237=CARTESIAN_POINT('Ctrl Pts',(96.8118973729564,-1.21642647252748,-5.29587426582507));
#21238=CARTESIAN_POINT('Ctrl Pts',(96.74890536976,-1.23288178663247,-5.29955174558859));
#21239=CARTESIAN_POINT('Ctrl Pts',(96.6479723017219,-1.25108656976633,-5.30555088141909));
#21240=CARTESIAN_POINT('Ctrl Pts',(96.6107387393857,-1.25610216849582,-5.30778747009319));
#21241=CARTESIAN_POINT('Ctrl Pts',(96.5533600376612,-1.26124390004,-5.31134397830249));
#21242=CARTESIAN_POINT('Ctrl Pts',(96.5333431143548,-1.26255840877144,-5.31260619177808));
#21243=CARTESIAN_POINT('Ctrl Pts',(96.4848206225441,-1.26458704372851,-5.31572651623737));
#21244=CARTESIAN_POINT('Ctrl Pts',(96.4563103700845,-1.26481426615795,-5.31760638510492));
#21245=CARTESIAN_POINT('Ctrl Pts',(96.338870680238,-1.26177984091943,-5.32547815892105));
#21246=CARTESIAN_POINT('Ctrl Pts',(96.2504141362109,-1.25009988050842,-5.33168995699856));
#21247=CARTESIAN_POINT('Ctrl Pts',(96.122477221436,-1.21923369593521,-5.34063361393174));
#21248=CARTESIAN_POINT('Ctrl Pts',(96.0815680163989,-1.20714659420612,-5.34349100484987));
#21249=CARTESIAN_POINT('Ctrl Pts',(96.0340575203261,-1.19045493739913,-5.34679512413616));
#21250=CARTESIAN_POINT('Ctrl Pts',(96.0267949549122,-1.18782841401933,-5.34729983970381));
#21251=CARTESIAN_POINT('Ctrl Pts',(96.0195573809006,-1.1851357123071,-5.34780246104807));
#21252=CARTESIAN_POINT('Origin',(96.460480949577,-1.62868768791465E-15,
-6.49999999999999));
#21253=CARTESIAN_POINT('',(96.0195573766758,-1.18513571073528,-5.84684438197146));
#21254=CARTESIAN_POINT('',(96.0195573765031,-1.18513571067102,-5.70991346827675));
#21255=CARTESIAN_POINT('',(96.0195573765031,-1.18513571067102,-6.49999999999999));
#21256=CARTESIAN_POINT('',(97.7249809164252,0.000289553175782366,-5.55658032643166));
#21257=CARTESIAN_POINT('Ctrl Pts',(96.019557376503,-1.18513571067102,-5.70991346827675));
#21258=CARTESIAN_POINT('Ctrl Pts',(96.0672300587458,-1.20287208398524,-5.70669551900282));
#21259=CARTESIAN_POINT('Ctrl Pts',(96.1160769577919,-1.21776546375623,-5.7034775697289));
#21260=CARTESIAN_POINT('Ctrl Pts',(96.1657252529368,-1.22966634877033,-5.70025962045498));
#21261=CARTESIAN_POINT('Ctrl Pts',(96.2137887264982,-1.24118734602841,-5.69714439123315));
#21262=CARTESIAN_POINT('Ctrl Pts',(96.2626026199803,-1.24990389543441,-5.69402916201133));
#21263=CARTESIAN_POINT('Ctrl Pts',(96.3118102439555,-1.25572977638105,-5.6909139327895));
#21264=CARTESIAN_POINT('Ctrl Pts',(96.3609731670002,-1.26155036501162,-5.68780153348779));
#21265=CARTESIAN_POINT('Ctrl Pts',(96.4105285703443,-1.26448542032649,-5.68468913418607));
#21266=CARTESIAN_POINT('Ctrl Pts',(96.4601105045368,-1.26449994573763,-5.68157673488436));
#21267=CARTESIAN_POINT('Ctrl Pts',(96.5096684816013,-1.26451446413035,-5.67846583943983));
#21268=CARTESIAN_POINT('Ctrl Pts',(96.5592524169426,-1.26161124898055,-5.67535494399531));
#21269=CARTESIAN_POINT('Ctrl Pts',(96.6084947901584,-1.25580737097548,-5.67224404855078));
#21270=CARTESIAN_POINT('Ctrl Pts',(96.6577343084241,-1.25000382946479,-5.66913333346822));
#21271=CARTESIAN_POINT('Ctrl Pts',(96.7066317603219,-1.24130002598907,-5.66602261838567));
#21272=CARTESIAN_POINT('Ctrl Pts',(96.7548257830587,-1.22976476165267,-5.66291190330311));
#21273=CARTESIAN_POINT('Ctrl Pts',(96.8030700054266,-1.2182174820085,-5.65979794805214));
#21274=CARTESIAN_POINT('Ctrl Pts',(96.8506088036549,-1.20383298721585,-5.65668399280118));
#21275=CARTESIAN_POINT('Ctrl Pts',(96.897093860719,-1.18673055738196,-5.65357003755021));
#21276=CARTESIAN_POINT('Ctrl Pts',(96.9436083605024,-1.16961729520598,-5.65045410998134));
#21277=CARTESIAN_POINT('Ctrl Pts',(96.9890672892405,-1.1497828924537,-5.64733818241247));
#21278=CARTESIAN_POINT('Ctrl Pts',(97.0331435518692,-1.12739424955777,-5.6442222548436));
#21279=CARTESIAN_POINT('Ctrl Pts',(97.0772978810094,-1.10496595259083,-5.64110080844031));
#21280=CARTESIAN_POINT('Ctrl Pts',(97.1200641889183,-1.07997467101853,-5.63797936203702));
#21281=CARTESIAN_POINT('Ctrl Pts',(97.1611427340333,-1.05263161352988,-5.63485791563373));
#21282=CARTESIAN_POINT('Ctrl Pts',(97.1706848147781,-1.04628013098259,-5.63413283899001));
#21283=CARTESIAN_POINT('Ctrl Pts',(97.1801359668656,-1.03980192374125,-5.6334077623463));
#21284=CARTESIAN_POINT('Ctrl Pts',(97.1894926961252,-1.03319994357083,-5.63268268570258));
#21285=CARTESIAN_POINT('Ctrl Pts',(97.2304118859496,-1.00432792298384,-5.62951175406629));
#21286=CARTESIAN_POINT('Ctrl Pts',(97.2697102211182,-0.972952719807752,
-5.62634082243));
#21287=CARTESIAN_POINT('Ctrl Pts',(97.3070638328496,-0.939285724234015,
-5.62316989079372));
#21288=CARTESIAN_POINT('Ctrl Pts',(97.3435475108083,-0.906402804285653,
-5.62007280745198));
#21289=CARTESIAN_POINT('Ctrl Pts',(97.3781756233914,-0.871334071940765,
-5.61697572411024));
#21290=CARTESIAN_POINT('Ctrl Pts',(97.4106760157132,-0.834319834530179,
-5.6138786407685));
#21291=CARTESIAN_POINT('Ctrl Pts',(97.4431443732015,-0.797342081138584,
-5.61078461014527));
#21292=CARTESIAN_POINT('Ctrl Pts',(97.4734887958835,-0.758423032899424,
-5.60769057952203));
#21293=CARTESIAN_POINT('Ctrl Pts',(97.5014737604642,-0.717839966622951,
-5.6045965488988));
#21294=CARTESIAN_POINT('Ctrl Pts',(97.5294434203483,-0.677279094818499,
-5.60150421036989));
#21295=CARTESIAN_POINT('Ctrl Pts',(97.5550558631182,-0.635056463904144,
-5.59841187184098));
#21296=CARTESIAN_POINT('Ctrl Pts',(97.5781173633259,-0.591480427962307,
-5.59531953331207));
#21297=CARTESIAN_POINT('Ctrl Pts',(97.6021925688477,-0.545988937310035,
-5.59209126607204));
#21298=CARTESIAN_POINT('Ctrl Pts',(97.6234869621405,-0.499022814786495,
-5.588862998832));
#21299=CARTESIAN_POINT('Ctrl Pts',(97.6418336145739,-0.450961340809636,
-5.58563473159197));
#21300=CARTESIAN_POINT('Ctrl Pts',(97.6594234474501,-0.404882455404688,
-5.58253963392015));
#21301=CARTESIAN_POINT('Ctrl Pts',(97.6743038976555,-0.357797411132342,
-5.57944453624833));
#21302=CARTESIAN_POINT('Ctrl Pts',(97.6863783994627,-0.310057562984182,
-5.5763494385765));
#21303=CARTESIAN_POINT('Ctrl Pts',(97.6984605247094,-0.262287573481037,
-5.57325238676278));
#21304=CARTESIAN_POINT('Ctrl Pts',(97.7077330754251,-0.213862503409765,
-5.57015533494906));
#21305=CARTESIAN_POINT('Ctrl Pts',(97.7141507901325,-0.165142910479476,
-5.56705828313533));
#21306=CARTESIAN_POINT('Ctrl Pts',(97.7205794615709,-0.116340140358935,
-5.56395594383761));
#21307=CARTESIAN_POINT('Ctrl Pts',(97.7241435458509,-0.0672423976822919,
-5.5608536045399));
#21308=CARTESIAN_POINT('Ctrl Pts',(97.7248497887175,-0.018212320294003,
-5.55775126524218));
#21309=CARTESIAN_POINT('Ctrl Pts',(97.7249386428695,-0.0120437256748006,
-5.55736095230534));
#21310=CARTESIAN_POINT('Ctrl Pts',(97.7249823282973,-0.0058761959988108,
-5.5569706393685));
#21311=CARTESIAN_POINT('Ctrl Pts',(97.7249809164252,0.000289553175783053,
-5.55658032643166));
#21312=CARTESIAN_POINT('Ctrl Pts',(97.724980916425,0.00028955398282956,
-5.55658032638057));
#21313=CARTESIAN_POINT('Ctrl Pts',(97.7249773196589,0.0159968514554625,
-5.55558600091696));
#21314=CARTESIAN_POINT('Ctrl Pts',(97.7246810658307,0.0317004476496653,
-5.55459167545336));
#21315=CARTESIAN_POINT('Ctrl Pts',(97.7240925016085,0.0473929907538893,
-5.55359734998976));
#21316=CARTESIAN_POINT('Ctrl Pts',(97.7222443974738,0.0966679087703951,
-5.55047514695516));
#21317=CARTESIAN_POINT('Ctrl Pts',(97.7175057083344,0.145942192786499,-5.54735294392056));
#21318=CARTESIAN_POINT('Ctrl Pts',(97.7098783470884,0.194849667928159,-5.54423074088596));
#21319=CARTESIAN_POINT('Ctrl Pts',(97.7022649183057,0.243667806590612,-5.54111424100053));
#21320=CARTESIAN_POINT('Ctrl Pts',(97.6917733667566,0.292119928404832,-5.53799774111509));
#21321=CARTESIAN_POINT('Ctrl Pts',(97.6784574996112,0.339843160247207,-5.53488124122966));
#21322=CARTESIAN_POINT('Ctrl Pts',(97.6651550390072,0.387518343886712,-5.5317678790659));
#21323=CARTESIAN_POINT('Ctrl Pts',(97.6490340389043,0.434465565284101,-5.52865451690213));
#21324=CARTESIAN_POINT('Ctrl Pts',(97.6301992689561,0.480332492455985,-5.52554115473836));
#21325=CARTESIAN_POINT('Ctrl Pts',(97.6113754586339,0.526172730458223,-5.52242960418605));
#21326=CARTESIAN_POINT('Ctrl Pts',(97.5898412146458,0.570933413838964,-5.51931805363375));
#21327=CARTESIAN_POINT('Ctrl Pts',(97.5657501871831,0.614280198607817,-5.51620650308144));
#21328=CARTESIAN_POINT('Ctrl Pts',(97.5416629416409,0.657620178598667,-5.51309544099467));
#21329=CARTESIAN_POINT('Ctrl Pts',(97.5150199764645,0.699546222686597,-5.50998437890791));
#21330=CARTESIAN_POINT('Ctrl Pts',(97.4860206310223,0.739749019452612,-5.50687331682114));
#21331=CARTESIAN_POINT('Ctrl Pts',(97.4569931298087,0.779990849539505,-5.50375923417126));
#21332=CARTESIAN_POINT('Ctrl Pts',(97.4256050027741,0.818505647624967,-5.50064515152139));
#21333=CARTESIAN_POINT('Ctrl Pts',(97.3920975747538,0.855015037115848,-5.49753106887151));
#21334=CARTESIAN_POINT('Ctrl Pts',(97.3585719136484,0.891544293210746,-5.49441529169188));
#21335=CARTESIAN_POINT('Ctrl Pts',(97.322925049016,0.92606558632132,-5.49129951451225));
#21336=CARTESIAN_POINT('Ctrl Pts',(97.2854345824381,0.95833801637487,-5.48818373733262));
#21337=CARTESIAN_POINT('Ctrl Pts',(97.2478753372162,0.990669652252652,-5.48506224406171));
#21338=CARTESIAN_POINT('Ctrl Pts',(97.2084661758971,1.02074385925813,-5.4819407507908));
#21339=CARTESIAN_POINT('Ctrl Pts',(97.1675157658607,1.04836158769895,-5.47881925751989));
#21340=CARTESIAN_POINT('Ctrl Pts',(97.1486804028236,1.06106451157642,-5.47738350977222));
#21341=CARTESIAN_POINT('Ctrl Pts',(97.129519342501,1.07324837335567,-5.47594776202456));
#21342=CARTESIAN_POINT('Ctrl Pts',(97.1100642892041,1.08489710796872,-5.4745120142769));
#21343=CARTESIAN_POINT('Ctrl Pts',(97.0677616465199,1.11022586191971,-5.47139015575371));
#21344=CARTESIAN_POINT('Ctrl Pts',(97.0238829786064,1.13313200228666,-5.46826829723051));
#21345=CARTESIAN_POINT('Ctrl Pts',(96.9787361896904,1.15341742491392,-5.46514643870732));
#21346=CARTESIAN_POINT('Ctrl Pts',(96.933671681372,1.17366587710011,-5.46203026981104));
#21347=CARTESIAN_POINT('Ctrl Pts',(96.8873441317738,1.19130286203269,-5.45891410091476));
#21348=CARTESIAN_POINT('Ctrl Pts',(96.8400869848865,1.20617557095001,-5.45579793201849));
#21349=CARTESIAN_POINT('Ctrl Pts',(96.7928772909562,1.22103334553333,-5.45268489220295));
#21350=CARTESIAN_POINT('Ctrl Pts',(96.7447403678977,1.23313217566415,-5.44957185238742));
#21351=CARTESIAN_POINT('Ctrl Pts',(96.6960286204964,1.24236771719344,-5.44645881257189));
#21352=CARTESIAN_POINT('Ctrl Pts',(96.6473450773759,1.25159791131024,-5.44334757521785));
#21353=CARTESIAN_POINT('Ctrl Pts',(96.5980879066095,1.25796799945789,-5.44023633786381));
#21354=CARTESIAN_POINT('Ctrl Pts',(96.5486210950282,1.26142441896446,-5.43712510050977));
#21355=CARTESIAN_POINT('Ctrl Pts',(96.4991618960032,1.26488030655505,-5.43401434195088));
#21356=CARTESIAN_POINT('Ctrl Pts',(96.4494936665463,1.26542337874327,-5.43090358339198));
#21357=CARTESIAN_POINT('Ctrl Pts',(96.3999843288109,1.26305202144483,-5.42779282483309));
#21358=CARTESIAN_POINT('Ctrl Pts',(96.3504266505215,1.26067834877054,-5.42467902895238));
#21359=CARTESIAN_POINT('Ctrl Pts',(96.3010287218844,1.2553845929793,-5.42156523307166));
#21360=CARTESIAN_POINT('Ctrl Pts',(96.2521554339637,1.24722120313296,-5.41845143719094));
#21361=CARTESIAN_POINT('Ctrl Pts',(96.2032554051967,1.23905334671679,-5.41533593760784));
#21362=CARTESIAN_POINT('Ctrl Pts',(96.154881123348,1.22801285186346,-5.41222043802474));
#21363=CARTESIAN_POINT('Ctrl Pts',(96.1073858474992,1.21420101255461,-5.40910493844164));
#21364=CARTESIAN_POINT('Ctrl Pts',(96.0598031697776,1.20036375638901,-5.40598370564627));
#21365=CARTESIAN_POINT('Ctrl Pts',(96.0131032424064,1.1837451619834,-5.4028624728509));
#21366=CARTESIAN_POINT('Ctrl Pts',(95.9676211855102,1.16449538554863,-5.39974124005553));
#21367=CARTESIAN_POINT('Ctrl Pts',(95.9466641743868,1.15562556288895,-5.39830305289172));
#21368=CARTESIAN_POINT('Ctrl Pts',(95.9259654073852,1.14619775605937,-5.39686486572792));
#21369=CARTESIAN_POINT('Ctrl Pts',(95.9055557978332,1.13622987373246,-5.39542667856412));
#21370=CARTESIAN_POINT('Ctrl Pts',(95.8612893983061,1.11461053503822,-5.3923073946099));
#21371=CARTESIAN_POINT('Ctrl Pts',(95.818190521751,1.09035270442906,-5.38918811065567));
#21372=CARTESIAN_POINT('Ctrl Pts',(95.7765928412365,1.06360580351487,-5.38606882670145));
#21373=CARTESIAN_POINT('Ctrl Pts',(95.7350712395224,1.03690782052367,-5.38295524766581));
#21374=CARTESIAN_POINT('Ctrl Pts',(95.6950458466465,1.00773009012625,-5.37984166863018));
#21375=CARTESIAN_POINT('Ctrl Pts',(95.656826359082,0.976268174825118,-5.37672808959454));
#21376=CARTESIAN_POINT('Ctrl Pts',(95.6186453699179,0.944837951037592,-5.37361764685978));
#21377=CARTESIAN_POINT('Ctrl Pts',(95.5822671067884,0.911128444320484,-5.37050720412501));
#21378=CARTESIAN_POINT('Ctrl Pts',(95.5479710293874,0.87537757313946,-5.36739676139025));
#21379=CARTESIAN_POINT('Ctrl Pts',(95.5136948509245,0.83964744498297,-5.36428812336647));
#21380=CARTESIAN_POINT('Ctrl Pts',(95.4814988442001,0.80187869411898,-5.36117948534269));
#21381=CARTESIAN_POINT('Ctrl Pts',(95.4516262505552,0.762346670656862,-5.35807084731891));
#21382=CARTESIAN_POINT('Ctrl Pts',(95.4217582318716,0.722820701489285,-5.3549626853803));
#21383=CARTESIAN_POINT('Ctrl Pts',(95.3942132496516,0.681532434250401,-5.35185452344169));
#21384=CARTESIAN_POINT('Ctrl Pts',(95.3691931651421,0.638788870866742,-5.34874636150309));
#21385=CARTESIAN_POINT('Ctrl Pts',(95.3441484327452,0.596003199769932,-5.34563513763934));
#21386=CARTESIAN_POINT('Ctrl Pts',(95.3216338405391,0.551759845614649,-5.34252391377559));
#21387=CARTESIAN_POINT('Ctrl Pts',(95.3018059666686,0.506391680403736,-5.33941268991184));
#21388=CARTESIAN_POINT('Ctrl Pts',(95.2819671688355,0.460998520070124,-5.33629975195139));
#21389=CARTESIAN_POINT('Ctrl Pts',(95.2648182263788,0.414479830365957,-5.33318681399095));
#21390=CARTESIAN_POINT('Ctrl Pts',(95.250466754593,0.367186462083226,-5.3300738760305));
#21391=CARTESIAN_POINT('Ctrl Pts',(95.2360886407396,0.319805298406776,-5.32695515921302));
#21392=CARTESIAN_POINT('Ctrl Pts',(95.2245184892159,0.271647120120269,-5.32383644239554));
#21393=CARTESIAN_POINT('Ctrl Pts',(95.2158130647497,0.223074217424636,-5.32071772557806));
#21394=CARTESIAN_POINT('Ctrl Pts',(95.2117410621182,0.200354017121378,-5.3192589313358));
#21395=CARTESIAN_POINT('Ctrl Pts',(95.2082951045729,0.177543161626589,-5.31780013709354));
#21396=CARTESIAN_POINT('Ctrl Pts',(95.2054770925123,0.154678921487683,-5.31634134285128));
#21397=CARTESIAN_POINT('Ctrl Pts',(95.1994370883039,0.105672705868238,-5.31321462686395));
#21398=CARTESIAN_POINT('Ctrl Pts',(95.1962587973972,0.0562066151787424,
-5.31008791087661));
#21399=CARTESIAN_POINT('Ctrl Pts',(95.1959984009778,0.00664336421897154,
-5.30696119488927));
#21400=CARTESIAN_POINT('Ctrl Pts',(95.1957384816704,-0.0428290743508711,
-5.30384020783509));
#21401=CARTESIAN_POINT('Ctrl Pts',(95.1983858545174,-0.0923977783162371,
-5.3007192207809));
#21402=CARTESIAN_POINT('Ctrl Pts',(95.2039449368609,-0.141695090766752,
-5.29759823372672));
#21403=CARTESIAN_POINT('Ctrl Pts',(95.2094983944853,-0.190942523845796,
-5.29448040450944));
#21404=CARTESIAN_POINT('Ctrl Pts',(95.2179576673769,-0.239918569063965,
-5.29136257529216));
#21405=CARTESIAN_POINT('Ctrl Pts',(95.2292751844159,-0.288257894660407,
-5.28824474607488));
#21406=CARTESIAN_POINT('Ctrl Pts',(95.2405860216583,-0.336568689541037,
-5.28512875705496));
#21407=CARTESIAN_POINT('Ctrl Pts',(95.2547516361753,-0.384242978755336,
-5.28201276803504));
#21408=CARTESIAN_POINT('Ctrl Pts',(95.2716733384852,-0.430925415600221,
-5.27889677901512));
#21409=CARTESIAN_POINT('Ctrl Pts',(95.288592186744,-0.477599978883804,-5.27578131554469));
#21410=CARTESIAN_POINT('Ctrl Pts',(95.3082660128915,-0.52328250925045,-5.27266585207425));
#21411=CARTESIAN_POINT('Ctrl Pts',(95.3305470313202,-0.567635085572367,
-5.26955038860382));
#21412=CARTESIAN_POINT('Ctrl Pts',(95.3528490062695,-0.612029377926409,
-5.26643199486901));
#21413=CARTESIAN_POINT('Ctrl Pts',(95.3777628229908,-0.655090730421877,
-5.2633136011342));
#21414=CARTESIAN_POINT('Ctrl Pts',(95.4050943116575,-0.696505057053423,
-5.2601952073994));
#21415=CARTESIAN_POINT('Ctrl Pts',(95.4324402504819,-0.737941279438834,
-5.25707516496987));
#21416=CARTESIAN_POINT('Ctrl Pts',(95.4622060799938,-0.777728303751934,
-5.25395512254034));
#21417=CARTESIAN_POINT('Ctrl Pts',(95.4941558127478,-0.81558321459684,-5.25083508011081));
#21418=CARTESIAN_POINT('Ctrl Pts',(95.5261628610009,-0.853506034401186,
-5.24770944055188));
#21419=CARTESIAN_POINT('Ctrl Pts',(95.5603612553392,-0.889489427160365,
-5.24458380099294));
#21420=CARTESIAN_POINT('Ctrl Pts',(95.5964776307581,-0.923286800008501,
-5.241458161434));
#21421=CARTESIAN_POINT('Ctrl Pts',(95.6126627537539,-0.938432689653773,
-5.24005744333549));
#21422=CARTESIAN_POINT('Ctrl Pts',(95.6292326148829,-0.953140105703813,
-5.23865672523698));
#21423=CARTESIAN_POINT('Ctrl Pts',(95.6461606096548,-0.967389597829645,
-5.23725600713846));
#21424=CARTESIAN_POINT('Ctrl Pts',(95.6838682375086,-0.999130778839254,
-5.23413586458772));
#21425=CARTESIAN_POINT('Ctrl Pts',(95.7235161537926,-1.02873270917244,-5.23101572203697));
#21426=CARTESIAN_POINT('Ctrl Pts',(95.764832046977,-1.05595116094986,-5.22789557948622));
#21427=CARTESIAN_POINT('Ctrl Pts',(95.8060827129411,-1.0831266417587,-5.22478036284194));
#21428=CARTESIAN_POINT('Ctrl Pts',(95.8489956849724,-1.10792579976192,-5.22166514619765));
#21429=CARTESIAN_POINT('Ctrl Pts',(95.8932660745554,-1.13014491794379,-5.21854992955337));
#21430=CARTESIAN_POINT('Ctrl Pts',(95.9342862709442,-1.15073277813646,-5.21566342234739));
#21431=CARTESIAN_POINT('Ctrl Pts',(95.9764712566442,-1.16910574402079,-5.21277691514142));
#21432=CARTESIAN_POINT('Ctrl Pts',(96.019557376503,-1.18513571067102,-5.20989040793544));
#21433=CARTESIAN_POINT('Ctrl Pts',(96.0195573809006,-1.1851357123071,-5.34780246104807));
#21434=CARTESIAN_POINT('Ctrl Pts',(95.9911569000717,-1.17456946134598,-5.34977476389832));
#21435=CARTESIAN_POINT('Ctrl Pts',(95.9631412136764,-1.16298419416518,-5.35171447379949));
#21436=CARTESIAN_POINT('Ctrl Pts',(95.90327232285,-1.13566663154017,-5.35585319061882));
#21437=CARTESIAN_POINT('Ctrl Pts',(95.8716126124167,-1.11957787589962,-5.35803753528189));
#21438=CARTESIAN_POINT('Ctrl Pts',(95.7789345827735,-1.06746016986719,-5.3644562136911));
#21439=CARTESIAN_POINT('Ctrl Pts',(95.7202229885252,-1.02761682618313,-5.36854852764157));
#21440=CARTESIAN_POINT('Ctrl Pts',(95.6189843420318,-0.945711492749465,
-5.37600713338699));
#21441=CARTESIAN_POINT('Ctrl Pts',(95.5755077621782,-0.90515664375042,-5.37937733454893));
#21442=CARTESIAN_POINT('Ctrl Pts',(95.5105522626955,-0.83539656903172,-5.38496567420744));
#21443=CARTESIAN_POINT('Ctrl Pts',(95.4871955589494,-0.808063728116267,
-5.38711171708948));
#21444=CARTESIAN_POINT('Ctrl Pts',(95.4526231581329,-0.763929410360917,
-5.39057770429406));
#21445=CARTESIAN_POINT('Ctrl Pts',(95.4405921891734,-0.747791615837261,
-5.39184654568825));
#21446=CARTESIAN_POINT('Ctrl Pts',(95.4119352009272,-0.707373664449688,
-5.39503503107707));
#21447=CARTESIAN_POINT('Ctrl Pts',(95.3957641140544,-0.68279091753971,-5.39697912929723));
#21448=CARTESIAN_POINT('Ctrl Pts',(95.3360646053247,-0.584753256546981,
-5.40468531555168));
#21449=CARTESIAN_POINT('Ctrl Pts',(95.2991616379038,-0.507529482456535,
-5.41063881200647));
#21450=CARTESIAN_POINT('Ctrl Pts',(95.25568171314,-0.386389557460924,-5.41939549697864));
#21451=CARTESIAN_POINT('Ctrl Pts',(95.2431477106545,-0.344874589527996,
-5.4223044136229));
#21452=CARTESIAN_POINT('Ctrl Pts',(95.2235853959167,-0.265557153639341,
-5.42767121299091));
#21453=CARTESIAN_POINT('Ctrl Pts',(95.2160996080811,-0.227918425065709,
-5.43013994231391));
#21454=CARTESIAN_POINT('Ctrl Pts',(95.2050354991081,-0.155117492968852,
-5.43477567850614));
#21455=CARTESIAN_POINT('Ctrl Pts',(95.2011964767379,-0.120032138127394,
-5.4369490404489));
#21456=CARTESIAN_POINT('Ctrl Pts',(95.1945281719033,-0.0208555097307459,
-5.44295631467797));
#21457=CARTESIAN_POINT('Ctrl Pts',(95.1950984234687,0.0433559873195874,
-5.44668207222266));
#21458=CARTESIAN_POINT('Ctrl Pts',(95.2060335266596,0.171814811897757,-5.45408280060719));
#21459=CARTESIAN_POINT('Ctrl Pts',(95.2164833048842,0.235855473965022,-5.45774685108397));
#21460=CARTESIAN_POINT('Ctrl Pts',(95.2382788696431,0.325477382579932,-5.46314058223971));
#21461=CARTESIAN_POINT('Ctrl Pts',(95.2456302431665,0.351924731694582,-5.46476713914104));
#21462=CARTESIAN_POINT('Ctrl Pts',(95.2606510269022,0.399859856810959,-5.46781380157456));
#21463=CARTESIAN_POINT('Ctrl Pts',(95.2680526852936,0.421419520839781,-5.46922165092735));
#21464=CARTESIAN_POINT('Ctrl Pts',(95.2839999685176,0.46408033147565,-5.47210512927408));
#21465=CARTESIAN_POINT('Ctrl Pts',(95.2925410006007,0.485174355205833,-5.47358010934124));
#21466=CARTESIAN_POINT('Ctrl Pts',(95.3275518094054,0.565351795659446,-5.47934656150149));
#21467=CARTESIAN_POINT('Ctrl Pts',(95.3579736012902,0.622597227349399,-5.48379989415675));
#21468=CARTESIAN_POINT('Ctrl Pts',(95.4369365650063,0.747099177359437,-5.49393907156166));
#21469=CARTESIAN_POINT('Ctrl Pts',(95.4879838728063,0.812436735179592,-5.49959040755326));
#21470=CARTESIAN_POINT('Ctrl Pts',(95.5707645980753,0.899307558863883,-5.50744234627463));
#21471=CARTESIAN_POINT('Ctrl Pts',(95.5976575433849,0.925140810355008,-5.50983214883126));
#21472=CARTESIAN_POINT('Ctrl Pts',(95.6526545435528,0.97348289400719,-5.51442692831463));
#21473=CARTESIAN_POINT('Ctrl Pts',(95.6806554955213,0.996054770724119,-5.51663337792311));
#21474=CARTESIAN_POINT('Ctrl Pts',(95.7933515840982,1.07923043364241,-5.52506688512126));
#21475=CARTESIAN_POINT('Ctrl Pts',(95.884432419787,1.13047301025196,-5.53091475101771));
#21476=CARTESIAN_POINT('Ctrl Pts',(96.0305736855713,1.19039386961959,-5.54000351161491));
#21477=CARTESIAN_POINT('Ctrl Pts',(96.0816266759806,1.20761168217657,-5.54313883687816));
#21478=CARTESIAN_POINT('Ctrl Pts',(96.1540553835878,1.22699281191022,-5.54772527459907));
#21479=CARTESIAN_POINT('Ctrl Pts',(96.1746291829358,1.23194833939761,-5.54904367072386));
#21480=CARTESIAN_POINT('Ctrl Pts',(96.219963501988,1.24167103994746,-5.55199977182372));
#21481=CARTESIAN_POINT('Ctrl Pts',(96.2447599762878,1.24621822194121,-5.55364699100465));
#21482=CARTESIAN_POINT('Ctrl Pts',(96.3682399093674,1.26506661771489,-5.56194546564313));
#21483=CARTESIAN_POINT('Ctrl Pts',(96.4682380348751,1.26840149237045,-5.56893398562525));
#21484=CARTESIAN_POINT('Ctrl Pts',(96.6087947827134,1.2564526695749,-5.57850074490316));
#21485=CARTESIAN_POINT('Ctrl Pts',(96.6498052997827,1.25093051067384,-5.58126580767854));
#21486=CARTESIAN_POINT('Ctrl Pts',(96.7272659469987,1.2366025684872,-5.58642331452262));
#21487=CARTESIAN_POINT('Ctrl Pts',(96.763739664481,1.22816724521475,-5.58882377700623));
#21488=CARTESIAN_POINT('Ctrl Pts',(96.8343130364044,1.20850908797719,-5.59342303737393));
#21489=CARTESIAN_POINT('Ctrl Pts',(96.8684150080584,1.19742842961825,-5.59562401266924));
#21490=CARTESIAN_POINT('Ctrl Pts',(96.9550254467938,1.16515566383876,-5.60119219493759));
#21491=CARTESIAN_POINT('Ctrl Pts',(97.0066647780769,1.14186082303937,-5.60448845585805));
#21492=CARTESIAN_POINT('Ctrl Pts',(97.1166070746032,1.08309390435397,-5.61165866907361));
#21493=CARTESIAN_POINT('Ctrl Pts',(97.1739479409225,1.0462112655269,-5.61550121643613));
#21494=CARTESIAN_POINT('Ctrl Pts',(97.2585360174733,0.981601246340045,-5.62171816321294));
#21495=CARTESIAN_POINT('Ctrl Pts',(97.2879535081073,0.95693337407692,-5.62400001451163));
#21496=CARTESIAN_POINT('Ctrl Pts',(97.3311109753079,0.91726426748031,-5.62761572486773));
#21497=CARTESIAN_POINT('Ctrl Pts',(97.3456866604919,0.903206045813647,-5.62888890415512));
#21498=CARTESIAN_POINT('Ctrl Pts',(97.3797282065796,0.868757099131709,-5.63199914778414));
#21499=CARTESIAN_POINT('Ctrl Pts',(97.3988589496941,0.848057111250292,-5.63385644742696));
#21500=CARTESIAN_POINT('Ctrl Pts',(97.4932599148953,0.738805001983189,-5.64352554337023));
#21501=CARTESIAN_POINT('Ctrl Pts',(97.5567590509556,0.640815893675838,-5.65170272432219));
#21502=CARTESIAN_POINT('Ctrl Pts',(97.624608990299,0.495681461212182,-5.66237780665581));
#21503=CARTESIAN_POINT('Ctrl Pts',(97.6411439949906,0.454895306835878,-5.66524761896211));
#21504=CARTESIAN_POINT('Ctrl Pts',(97.666693488182,0.381024614454803,-5.67022208190327));
#21505=CARTESIAN_POINT('Ctrl Pts',(97.6765520425905,0.348281354497011,-5.67235299087159));
#21506=CARTESIAN_POINT('Ctrl Pts',(97.6974434641501,0.267109409052004,-5.67747840266826));
#21507=CARTESIAN_POINT('Ctrl Pts',(97.7069746336448,0.218352953423642,-5.68042208732178));
#21508=CARTESIAN_POINT('Ctrl Pts',(97.7247682415555,0.0865364592984473,
-5.68816673857076));
#21509=CARTESIAN_POINT('Ctrl Pts',(97.7277224927789,0.00301850559099509,
-5.69284191243654));
#21510=CARTESIAN_POINT('Ctrl Pts',(97.7197790382627,-0.122003240281741,
-5.70012514228139));
#21511=CARTESIAN_POINT('Ctrl Pts',(97.7150445459317,-0.163664092197564,
-5.70260338958254));
#21512=CARTESIAN_POINT('Ctrl Pts',(97.7049333509116,-0.225205217198401,
-5.70643980817995));
#21513=CARTESIAN_POINT('Ctrl Pts',(97.7011258855457,-0.245314622744633,
-5.70772265893581));
#21514=CARTESIAN_POINT('Ctrl Pts',(97.6910712438335,-0.29216676648176,-5.71079259891487));
#21515=CARTESIAN_POINT('Ctrl Pts',(97.6844388985957,-0.318811171856491,
-5.71259729145879));
#21516=CARTESIAN_POINT('Ctrl Pts',(97.6540060586253,-0.426049695415381,
-5.72004548788207));
#21517=CARTESIAN_POINT('Ctrl Pts',(97.6230676157072,-0.504393161237666,
-5.72590078850343));
#21518=CARTESIAN_POINT('Ctrl Pts',(97.5551479600919,-0.63623666745809,-5.73602116168861));
#21519=CARTESIAN_POINT('Ctrl Pts',(97.5213891236651,-0.691063609654764,
-5.74032580274532));
#21520=CARTESIAN_POINT('Ctrl Pts',(97.4630779210482,-0.771348987121128,
-5.74673990758684));
#21521=CARTESIAN_POINT('Ctrl Pts',(97.4413912258913,-0.798746123787804,
-5.7489525405346));
#21522=CARTESIAN_POINT('Ctrl Pts',(97.3929295453079,-0.855012681242475,
-5.7535629459878));
#21523=CARTESIAN_POINT('Ctrl Pts',(97.3658850299456,-0.883601158678016,
-5.75594614704933));
#21524=CARTESIAN_POINT('Ctrl Pts',(97.3048552130503,-0.942365258674599,
-5.76098159174631));
#21525=CARTESIAN_POINT('Ctrl Pts',(97.2704882598381,-0.972064181601018,
-5.76361472503132));
#21526=CARTESIAN_POINT('Ctrl Pts',(97.1680173257085,-1.05140028897219,-5.77106291245415));
#21527=CARTESIAN_POINT('Ctrl Pts',(97.0964618159717,-1.09616428050218,-5.77579065737659));
#21528=CARTESIAN_POINT('Ctrl Pts',(96.9964450239804,-1.14562340095486,-5.78244751105435));
#21529=CARTESIAN_POINT('Ctrl Pts',(96.9715069925848,-1.15696265706459,-5.78411223895859));
#21530=CARTESIAN_POINT('Ctrl Pts',(96.927585730249,-1.17523650367237,-5.78708560849603));
#21531=CARTESIAN_POINT('Ctrl Pts',(96.9087692567348,-1.1825417965678,-5.78837421224998));
#21532=CARTESIAN_POINT('Ctrl Pts',(96.8521939510208,-1.20296240868748,-5.79228437359231));
#21533=CARTESIAN_POINT('Ctrl Pts',(96.8139819051272,-1.21474033511454,-5.79496791798944));
#21534=CARTESIAN_POINT('Ctrl Pts',(96.7031121126548,-1.2432388238697,-5.8027595527477));
#21535=CARTESIAN_POINT('Ctrl Pts',(96.6294443888879,-1.25537434724787,-5.80793410682928));
#21536=CARTESIAN_POINT('Ctrl Pts',(96.4987825688458,-1.26518244348814,-5.81681911679945));
#21537=CARTESIAN_POINT('Ctrl Pts',(96.442205178669,-1.26563072099937,-5.82057393355728));
#21538=CARTESIAN_POINT('Ctrl Pts',(96.3513241613236,-1.26025253574166,-5.82643669795251));
#21539=CARTESIAN_POINT('Ctrl Pts',(96.3169631995085,-1.25680336256803,-5.82861523157875));
#21540=CARTESIAN_POINT('Ctrl Pts',(96.2422089631943,-1.24619302269063,-5.83328648687228));
#21541=CARTESIAN_POINT('Ctrl Pts',(96.2019356704957,-1.2384646074627,-5.83575855646203));
#21542=CARTESIAN_POINT('Ctrl Pts',(96.1145052424056,-1.21723474422539,-5.84108183283655));
#21543=CARTESIAN_POINT('Ctrl Pts',(96.0676147706023,-1.2029198833253,-5.84390774147123));
#21544=CARTESIAN_POINT('Ctrl Pts',(96.0209661975241,-1.18565914050278,-5.84675826449389));
#21545=CARTESIAN_POINT('Ctrl Pts',(96.0202616618289,-1.1853977363609,-5.84680132585598));
#21546=CARTESIAN_POINT('Ctrl Pts',(96.0195573766758,-1.18513571073528,-5.84684438197146));
#21547=CARTESIAN_POINT('Origin',(96.460480949577,-1.62868768791465E-15,
-6.49999999999999));
#21548=CARTESIAN_POINT('',(96.0195573796018,-1.18513571182388,-6.34560991122238));
#21549=CARTESIAN_POINT('',(96.0195573765031,-1.18513571067102,-6.20996462145127));
#21550=CARTESIAN_POINT('',(96.0195573765031,-1.18513571067102,-6.49999999999999));
#21551=CARTESIAN_POINT('',(95.5023647968546,0.825211298936472,-6.49999999999999));
#21552=CARTESIAN_POINT('Ctrl Pts',(96.0195573796018,-1.18513571182389,-6.34560991122238));
#21553=CARTESIAN_POINT('Ctrl Pts',(96.0042740283813,-1.17944962059055,-6.34669630916491));
#21554=CARTESIAN_POINT('Ctrl Pts',(95.9891013983046,-1.1734681624746,-6.34779485622615));
#21555=CARTESIAN_POINT('Ctrl Pts',(95.8749001292853,-1.12587434226586,-6.35619519895383));
#21556=CARTESIAN_POINT('Ctrl Pts',(95.7814167343244,-1.07208871018347,-6.36378134632822));
#21557=CARTESIAN_POINT('Ctrl Pts',(95.6595252904877,-0.979545956375136,
-6.37406645688343));
#21558=CARTESIAN_POINT('Ctrl Pts',(95.6247163845456,-0.950020376918963,
-6.37706580422017));
#21559=CARTESIAN_POINT('Ctrl Pts',(95.5676186247547,-0.896015886562431,
-6.38209833101502));
#21560=CARTESIAN_POINT('Ctrl Pts',(95.5445557459024,-0.872427050716327,
-6.38416743703659));
#21561=CARTESIAN_POINT('Ctrl Pts',(95.4935501700806,-0.816003097838945,
-6.3888484446704));
#21562=CARTESIAN_POINT('Ctrl Pts',(95.466310880474,-0.782587158110073,-6.39142875336817));
#21563=CARTESIAN_POINT('Ctrl Pts',(95.3729586430953,-0.655305243335814,
-6.40070552326952));
#21564=CARTESIAN_POINT('Ctrl Pts',(95.3180106426798,-0.553973072196473,
-6.40701751053078));
#21565=CARTESIAN_POINT('Ctrl Pts',(95.2678495498594,-0.421111348337773,
-6.41549320788654));
#21566=CARTESIAN_POINT('Ctrl Pts',(95.2590433970342,-0.395287199291953,
-6.41715199240577));
#21567=CARTESIAN_POINT('Ctrl Pts',(95.2451667610324,-0.349831138929065,
-6.42012514201814));
#21568=CARTESIAN_POINT('Ctrl Pts',(95.2397209063265,-0.330325748199002,
-6.42141960070249));
#21569=CARTESIAN_POINT('Ctrl Pts',(95.225408013026,-0.273860241682951,-6.42521202014989));
#21570=CARTESIAN_POINT('Ctrl Pts',(95.2177364137455,-0.236622123974852,
-6.42776497095821));
#21571=CARTESIAN_POINT('Ctrl Pts',(95.2016561848986,-0.135768792923902,
-6.4347300985314));
#21572=CARTESIAN_POINT('Ctrl Pts',(95.1963912129465,-0.0717630770358149,
-6.43919968672181));
#21573=CARTESIAN_POINT('Ctrl Pts',(95.1955571551129,0.0663688831531573,
-6.44871677454101));
#21574=CARTESIAN_POINT('Ctrl Pts',(95.2016076488731,0.140278435494044,-6.45372531453812));
#21575=CARTESIAN_POINT('Ctrl Pts',(95.2205944501537,0.251254509108818,-6.46106008424667));
#21576=CARTESIAN_POINT('Ctrl Pts',(95.2288335269183,0.288950656981483,-6.46352043213571));
#21577=CARTESIAN_POINT('Ctrl Pts',(95.2500298226118,0.368332320856639,-6.46865690033929));
#21578=CARTESIAN_POINT('Ctrl Pts',(95.263447158062,0.409843039809312,-6.4713155981658));
#21579=CARTESIAN_POINT('Ctrl Pts',(95.2978654715237,0.500093500750323,-6.47710355914663));
#21580=CARTESIAN_POINT('Ctrl Pts',(95.3198421132795,0.548371911951468,-6.48020434912742));
#21581=CARTESIAN_POINT('Ctrl Pts',(95.3765892482316,0.654756327765499,-6.48724330232058));
#21582=CARTESIAN_POINT('Ctrl Pts',(95.413120951706,0.711732229437045,-6.49116523286909));
#21583=CARTESIAN_POINT('Ctrl Pts',(95.469531735161,0.785898167737987,-6.49681222101937));
#21584=CARTESIAN_POINT('Ctrl Pts',(95.485652209214,0.805807056419567,-6.49838835766165));
#21585=CARTESIAN_POINT('Ctrl Pts',(95.5023647968546,0.825211298936453,-6.49999999999997));
#21586=CARTESIAN_POINT('',(97.4187254286765,0.825062281452326,-6.49999885521441));
#21587=CARTESIAN_POINT('Origin',(96.460480949577,-1.62868768791465E-15,
-6.49999999999999));
#21588=CARTESIAN_POINT('Ctrl Pts',(97.4187254286765,0.825062281452326,-6.49999885521441));
#21589=CARTESIAN_POINT('Ctrl Pts',(97.3858967656753,0.863190172866516,-6.49681290469843));
#21590=CARTESIAN_POINT('Ctrl Pts',(97.3507105028266,0.899446588913635,-6.49362695418244));
#21591=CARTESIAN_POINT('Ctrl Pts',(97.3134115668534,0.933525367685571,-6.49044100366646));
#21592=CARTESIAN_POINT('Ctrl Pts',(97.2771416397765,0.966663975763241,-6.48734294765305));
#21593=CARTESIAN_POINT('Ctrl Pts',(97.2388745424285,0.997743144397279,-6.48424489163965));
#21594=CARTESIAN_POINT('Ctrl Pts',(97.1988758698889,1.0265150713251,-6.48114683562624));
#21595=CARTESIAN_POINT('Ctrl Pts',(97.1589169072214,1.05525843406648,-6.4780518553001));
#21596=CARTESIAN_POINT('Ctrl Pts',(97.1172302197181,1.08169876539954,-6.47495687497397));
#21597=CARTESIAN_POINT('Ctrl Pts',(97.0741146672841,1.1056282876686,-6.47186189464784));
#21598=CARTESIAN_POINT('Ctrl Pts',(97.0310230292357,1.12954453723697,-6.46876863097727));
#21599=CARTESIAN_POINT('Ctrl Pts',(96.9865045804255,1.15095246716872,-6.46567536730671));
#21600=CARTESIAN_POINT('Ctrl Pts',(96.9408850876952,1.16968889627921,-6.46258210363614));
#21601=CARTESIAN_POINT('Ctrl Pts',(96.8928974367663,1.18939795409635,-6.45932826523569));
#21602=CARTESIAN_POINT('Ctrl Pts',(96.8436918788377,1.20615022387415,-6.45607442683525));
#21603=CARTESIAN_POINT('Ctrl Pts',(96.7936713798052,1.21981325915255,-6.45282058843481));
#21604=CARTESIAN_POINT('Ctrl Pts',(96.7460773488615,1.23281350777867,-6.4497245920231));
#21605=CARTESIAN_POINT('Ctrl Pts',(96.6977462137278,1.24301728061555,-6.44662859561139));
#21606=CARTESIAN_POINT('Ctrl Pts',(96.6490372721396,1.25036265268188,-6.44353259919968));
#21607=CARTESIAN_POINT('Ctrl Pts',(96.6002978581226,1.2577126200303,-6.44043466592531));
#21608=CARTESIAN_POINT('Ctrl Pts',(96.5511807201814,1.26220058097111,-6.43733673265095));
#21609=CARTESIAN_POINT('Ctrl Pts',(96.5020493292532,1.26381656889404,-6.43423879937658));
#21610=CARTESIAN_POINT('Ctrl Pts',(96.4528335652593,1.26543533194407,-6.43113554603856));
#21611=CARTESIAN_POINT('Ctrl Pts',(96.4036040526838,1.26417230827103,-6.42803229270053));
#21612=CARTESIAN_POINT('Ctrl Pts',(96.3547213014283,1.26006950079092,-6.4249290393625));
#21613=CARTESIAN_POINT('Ctrl Pts',(96.347407095385,1.25945560778172,-6.42446470718527));
#21614=CARTESIAN_POINT('Ctrl Pts',(96.3401006350908,1.25877823000001,-6.42400037500805));
#21615=CARTESIAN_POINT('Ctrl Pts',(96.3328031071444,1.25803760617549,-6.42353604283083));
#21616=CARTESIAN_POINT('Ctrl Pts',(96.2836700641156,1.25305110903481,-6.4204097714399));
#21617=CARTESIAN_POINT('Ctrl Pts',(96.2347256224352,1.24517140652293,-6.41728350004898));
#21618=CARTESIAN_POINT('Ctrl Pts',(96.1863359402262,1.23442487169048,-6.41415722865805));
#21619=CARTESIAN_POINT('Ctrl Pts',(96.1380323097693,1.22369744750535,-6.41103651674011));
#21620=CARTESIAN_POINT('Ctrl Pts',(96.0902820109455,1.2101134209591,-6.40791580482216));
#21621=CARTESIAN_POINT('Ctrl Pts',(96.0434444403454,1.19375072773503,-6.40479509290421));
#21622=CARTESIAN_POINT('Ctrl Pts',(95.9966526848103,1.17740403999209,-6.40167743357028));
#21623=CARTESIAN_POINT('Ctrl Pts',(95.9507724029185,1.15828424662825,-6.39855977423634));
#21624=CARTESIAN_POINT('Ctrl Pts',(95.9061490746303,1.1365194333658,-6.39544211490241));
#21625=CARTESIAN_POINT('Ctrl Pts',(95.8615505829259,1.11476673402734,-6.39232619080451));
#21626=CARTESIAN_POINT('Ctrl Pts',(95.8182081485231,1.09037217084127,-6.3892102667066));
#21627=CARTESIAN_POINT('Ctrl Pts',(95.7764460648763,1.06351141343782,-6.3860943426087));
#21628=CARTESIAN_POINT('Ctrl Pts',(95.7346896203363,1.03665428302482,-6.38297883925198));
#21629=CARTESIAN_POINT('Ctrl Pts',(95.694513561082,1.00733191603579,-6.37986333589527));
#21630=CARTESIAN_POINT('Ctrl Pts',(95.6562141965028,0.975763926315942,-6.37674783253855));
#21631=CARTESIAN_POINT('Ctrl Pts',(95.6178768828815,0.9441646573573,-6.37362924217584));
#21632=CARTESIAN_POINT('Ctrl Pts',(95.5814203974895,0.910315672587025,-6.37051065181313));
#21633=CARTESIAN_POINT('Ctrl Pts',(95.5471074406779,0.87447646237127,-6.36739206145042));
#21634=CARTESIAN_POINT('Ctrl Pts',(95.5127753534812,0.838617270843461,-6.36427173239071));
#21635=CARTESIAN_POINT('Ctrl Pts',(95.4805895286139,0.800766060685597,-6.36115140333101));
#21636=CARTESIAN_POINT('Ctrl Pts',(95.4507729140603,0.761216088251567,-6.3580310742713));
#21637=CARTESIAN_POINT('Ctrl Pts',(95.4209015349594,0.721593473890639,-6.35490501406435));
#21638=CARTESIAN_POINT('Ctrl Pts',(95.3934083529415,0.680266325213899,-6.3517789538574));
#21639=CARTESIAN_POINT('Ctrl Pts',(95.3684725476981,0.637556193778903,-6.34865289365045));
#21640=CARTESIAN_POINT('Ctrl Pts',(95.3572992818796,0.618418586350414,-6.3472521648063));
#21641=CARTESIAN_POINT('Ctrl Pts',(95.3466388518098,0.599003620967653,-6.34585143596215));
#21642=CARTESIAN_POINT('Ctrl Pts',(95.3365042561199,0.57934155950119,-6.344450707118));
#21643=CARTESIAN_POINT('Ctrl Pts',(95.3139346980989,0.535554510598412,-6.34133130976981));
#21644=CARTESIAN_POINT('Ctrl Pts',(95.2938776347594,0.490349461827888,-6.33821191242163));
#21645=CARTESIAN_POINT('Ctrl Pts',(95.2765114333301,0.444045532122585,-6.33509251507345));
#21646=CARTESIAN_POINT('Ctrl Pts',(95.2591772324271,0.397826926207398,-6.33197886580769));
#21647=CARTESIAN_POINT('Ctrl Pts',(95.2445242506752,0.350513965059787,-6.32886521654193));
#21648=CARTESIAN_POINT('Ctrl Pts',(95.232684067834,0.302448453760651,-6.32575156727617));
#21649=CARTESIAN_POINT('Ctrl Pts',(95.220855913153,0.254431771071159,-6.32264108109264));
#21650=CARTESIAN_POINT('Ctrl Pts',(95.2118350314374,0.205664582037257,-6.31953059490911));
#21651=CARTESIAN_POINT('Ctrl Pts',(95.2057034563715,0.156504608701772,-6.31642010872558));
#21652=CARTESIAN_POINT('Ctrl Pts',(95.1995754915037,0.107373580171323,-6.31331145395916));
#21653=CARTESIAN_POINT('Ctrl Pts',(95.1963335310209,0.05785076914855,-6.31020279919274));
#21654=CARTESIAN_POINT('Ctrl Pts',(95.1960082049391,0.00830229292427632,
-6.30709414442632));
#21655=CARTESIAN_POINT('Ctrl Pts',(95.1956829314711,-0.0412381699983763,
-6.30398599241175));
#21656=CARTESIAN_POINT('Ctrl Pts',(95.1982733584799,-0.0908037412840867,
-6.30087784039718));
#21657=CARTESIAN_POINT('Ctrl Pts',(95.2037580231822,-0.140027626822785,
-6.29776968838261));
#21658=CARTESIAN_POINT('Ctrl Pts',(95.2092480204707,-0.189299371369654,
-6.29465851439871));
#21659=CARTESIAN_POINT('Ctrl Pts',(95.2176378114134,-0.238228220506546,
-6.29154734041481));
#21660=CARTESIAN_POINT('Ctrl Pts',(95.2288541630233,-0.286453676260998,
-6.2884361664309));
#21661=CARTESIAN_POINT('Ctrl Pts',(95.2400766117048,-0.334705346783249,
-6.28532330125088));
#21662=CARTESIAN_POINT('Ctrl Pts',(95.2541285246363,-0.382252335743913,
-6.28221043607086));
#21663=CARTESIAN_POINT('Ctrl Pts',(95.270886658549,-0.428748962393644,-6.27909757089083));
#21664=CARTESIAN_POINT('Ctrl Pts',(95.2876757185828,-0.475331395751545,
-6.27597896110667));
#21665=CARTESIAN_POINT('Ctrl Pts',(95.3071807497549,-0.520859093903896,
-6.2728603513225));
#21666=CARTESIAN_POINT('Ctrl Pts',(95.3292308904484,-0.56500756961433,-6.26974174153834));
#21667=CARTESIAN_POINT('Ctrl Pts',(95.3395452702353,-0.585658873015048,
-6.26828295149395));
#21668=CARTESIAN_POINT('Ctrl Pts',(95.3504158959013,-0.60600876625644,-6.26682416144957));
#21669=CARTESIAN_POINT('Ctrl Pts',(95.3618220279849,-0.626026216708281,
-6.26536537140518));
#21670=CARTESIAN_POINT('Ctrl Pts',(95.3862264404441,-0.668855294403235,
-6.26224416312234));
#21671=CARTESIAN_POINT('Ctrl Pts',(95.4131923737913,-0.710348849357345,
-6.25912295483949));
#21672=CARTESIAN_POINT('Ctrl Pts',(95.4425490824497,-0.75018328686182,-6.25600174655665));
#21673=CARTESIAN_POINT('Ctrl Pts',(95.4718610012655,-0.789956948541213,
-6.25288530033449));
#21674=CARTESIAN_POINT('Ctrl Pts',(95.5035561501367,-0.828076067984123,
-6.24976885411233));
#21675=CARTESIAN_POINT('Ctrl Pts',(95.5374191234865,-0.864243666574703,
-6.24665240789017));
#21676=CARTESIAN_POINT('Ctrl Pts',(95.5712482049335,-0.900375066668326,
-6.24353908077665));
#21677=CARTESIAN_POINT('Ctrl Pts',(95.6072404428918,-0.934558414240511,
-6.24042575366312));
#21678=CARTESIAN_POINT('Ctrl Pts',(95.6451400881149,-0.966529632049719,
-6.2373124265496));
#21679=CARTESIAN_POINT('Ctrl Pts',(95.6830156252808,-0.99848051288896,-6.23420107983107));
#21680=CARTESIAN_POINT('Ctrl Pts',(95.7227957457026,-1.02822170148917,-6.23108973311255));
#21681=CARTESIAN_POINT('Ctrl Pts',(95.7641896991281,-1.05552770903858,-6.22797838639403));
#21682=CARTESIAN_POINT('Ctrl Pts',(95.8055977453848,-1.0828430130897,-6.22486598039799));
#21683=CARTESIAN_POINT('Ctrl Pts',(95.8486202712027,-1.1077211674086,-6.22175357440194));
#21684=CARTESIAN_POINT('Ctrl Pts',(95.8929370890279,-1.12997974156752,-6.21864116840589));
#21685=CARTESIAN_POINT('Ctrl Pts',(95.9341181936383,-1.15066337175352,-6.21574898608768));
#21686=CARTESIAN_POINT('Ctrl Pts',(95.9764163061855,-1.16908529998863,-6.21285680376948));
#21687=CARTESIAN_POINT('Ctrl Pts',(96.019557376503,-1.18513571067102,-6.20996462145127));
#21688=CARTESIAN_POINT('Origin',(96.460480949577,-1.62868768791465E-15,
-6.49999999999999));
#21689=CARTESIAN_POINT('',(97.7249806670019,0.000845359370495013,-6.05658032632427));
#21690=CARTESIAN_POINT('Ctrl Pts',(96.019557376503,-1.18513571067102,-6.20996462145127));
#21691=CARTESIAN_POINT('Ctrl Pts',(96.0660267857944,-1.20242441254618,-6.20684930690527));
#21692=CARTESIAN_POINT('Ctrl Pts',(96.1134739318379,-1.21696085111713,-6.20373399235928));
#21693=CARTESIAN_POINT('Ctrl Pts',(96.161542157495,-1.22865611486231,-6.20061867781328));
#21694=CARTESIAN_POINT('Ctrl Pts',(96.2096996992633,-1.24037310970873,-6.19749757466625));
#21695=CARTESIAN_POINT('Ctrl Pts',(96.2584800847753,-1.24923829350367,-6.19437647151922));
#21696=CARTESIAN_POINT('Ctrl Pts',(96.3075178516391,-1.25521414135965,-6.19125536837219));
#21697=CARTESIAN_POINT('Ctrl Pts',(96.3335747928904,-1.25838949632519,-6.18959692414558));
#21698=CARTESIAN_POINT('Ctrl Pts',(96.3597043403319,-1.26074993511101,-6.18793847991896));
#21699=CARTESIAN_POINT('Ctrl Pts',(96.3858516941013,-1.26229581486558,-6.18628003569235));
#21700=CARTESIAN_POINT('Ctrl Pts',(96.435076212288,-1.26520605912065,-6.18315787967173));
#21701=CARTESIAN_POINT('Ctrl Pts',(96.4845785340075,-1.26523899914194,-6.18003572365111));
#21702=CARTESIAN_POINT('Ctrl Pts',(96.5339939915407,-1.2623613122483,-6.1769135676305));
#21703=CARTESIAN_POINT('Ctrl Pts',(96.5833194667269,-1.25948886543608,-6.17379709685374));
#21704=CARTESIAN_POINT('Ctrl Pts',(96.6325578489456,-1.25371633546162,-6.17068062607698));
#21705=CARTESIAN_POINT('Ctrl Pts',(96.6813427647009,-1.24506237137752,-6.16756415530021));
#21706=CARTESIAN_POINT('Ctrl Pts',(96.7300787368613,-1.23641708940561,-6.16445081113095));
#21707=CARTESIAN_POINT('Ctrl Pts',(96.7783616064132,-1.22489619169181,-6.16133746696168));
#21708=CARTESIAN_POINT('Ctrl Pts',(96.8258305919044,-1.21057006771655,-6.15822412279241));
#21709=CARTESIAN_POINT('Ctrl Pts',(96.8732721248406,-1.19625222891322,-6.15511257915144));
#21710=CARTESIAN_POINT('Ctrl Pts',(96.9199001827917,-1.17913253598975,-6.15200103551048));
#21711=CARTESIAN_POINT('Ctrl Pts',(96.965367188887,-1.15933176241982,-6.14888949186952));
#21712=CARTESIAN_POINT('Ctrl Pts',(97.0108272190594,-1.13953402684777,-6.14577842562723));
#21713=CARTESIAN_POINT('Ctrl Pts',(97.0551260495896,-1.11705624700979,-6.14266735938494));
#21714=CARTESIAN_POINT('Ctrl Pts',(97.0979366269534,-1.09206708098938,-6.13955629314265));
#21715=CARTESIAN_POINT('Ctrl Pts',(97.1407889975127,-1.0670535196637,-6.13644218976777));
#21716=CARTESIAN_POINT('Ctrl Pts',(97.18214974099,-1.03952395519453,-6.13332808639288));
#21717=CARTESIAN_POINT('Ctrl Pts',(97.2217185565937,-1.00969181221967,-6.130213983018));
#21718=CARTESIAN_POINT('Ctrl Pts',(97.2613090242038,-0.979843345133546,
-6.12709817560965));
#21719=CARTESIAN_POINT('Ctrl Pts',(97.2991051938811,-0.947690145919837,
-6.12398236820129));
#21720=CARTESIAN_POINT('Ctrl Pts',(97.3348405799922,-0.913485351114174,
-6.12086656079294));
#21721=CARTESIAN_POINT('Ctrl Pts',(97.3706416870465,-0.87921765027555,-6.11774502310366));
#21722=CARTESIAN_POINT('Ctrl Pts',(97.4043740742807,-0.842891225610397,
-6.11462348541437));
#21723=CARTESIAN_POINT('Ctrl Pts',(97.4358099246297,-0.804794160281114,
-6.11150194772509));
#21724=CARTESIAN_POINT('Ctrl Pts',(97.450268823739,-0.787271439634474,-6.11006619847657));
#21725=CARTESIAN_POINT('Ctrl Pts',(97.4642424724161,-0.769374560283098,
-6.10863044922805));
#21726=CARTESIAN_POINT('Ctrl Pts',(97.4777118314382,-0.751133532062002,
-6.10719469997953));
#21727=CARTESIAN_POINT('Ctrl Pts',(97.5071324118337,-0.711290386119013,
-6.10405865051165));
#21728=CARTESIAN_POINT('Ctrl Pts',(97.5342734560223,-0.669628381785422,
-6.10092260104378));
#21729=CARTESIAN_POINT('Ctrl Pts',(97.5589058189251,-0.626436793617297,
-6.0977865515759));
#21730=CARTESIAN_POINT('Ctrl Pts',(97.5834971366913,-0.583317175996531,
-6.09465572773659));
#21731=CARTESIAN_POINT('Ctrl Pts',(97.6055877889655,-0.538673489737358,
-6.09152490389727));
#21732=CARTESIAN_POINT('Ctrl Pts',(97.6249909763388,-0.492825169376669,
-6.08839408005796));
#21733=CARTESIAN_POINT('Ctrl Pts',(97.6443683868088,-0.447037757963643,
-6.08526741548083));
#21734=CARTESIAN_POINT('Ctrl Pts',(97.6610652036555,-0.400049382221009,
-6.08214075090371));
#21735=CARTESIAN_POINT('Ctrl Pts',(97.6749410183884,-0.352203054022458,
-6.07901408632658));
#21736=CARTESIAN_POINT('Ctrl Pts',(97.6888061404595,-0.304393596062708,
-6.07588983114792));
#21737=CARTESIAN_POINT('Ctrl Pts',(97.6998544203136,-0.255728014784932,
-6.07276557596926));
#21738=CARTESIAN_POINT('Ctrl Pts',(97.7079947697202,-0.206566014996665,
-6.06964132079059));
#21739=CARTESIAN_POINT('Ctrl Pts',(97.7161336663075,-0.157412789218061,
-6.06651762320205));
#21740=CARTESIAN_POINT('Ctrl Pts',(97.7213655669361,-0.10776385298261,-6.0633939256135));
#21741=CARTESIAN_POINT('Ctrl Pts',(97.7236506113726,-0.0579884084902515,
-6.06027022802495));
#21742=CARTESIAN_POINT('Ctrl Pts',(97.7245503558778,-0.0383891473287692,
-6.05904026081016));
#21743=CARTESIAN_POINT('Ctrl Pts',(97.7249937807201,-0.0187703344427737,
-6.05781029359537));
#21744=CARTESIAN_POINT('Ctrl Pts',(97.7249806670025,0.000845358472601678,
-6.05658032638057));
#21745=CARTESIAN_POINT('Ctrl Pts',(97.7249806670019,0.000845359370495876,
-6.05658032632427));
#21746=CARTESIAN_POINT('Ctrl Pts',(97.724942949461,0.0572637554750245,-6.05304271091496));
#21747=CARTESIAN_POINT('Ctrl Pts',(97.7211253245776,0.113535642676729,-6.04950509550565));
#21748=CARTESIAN_POINT('Ctrl Pts',(97.7136104799324,0.169194060626093,-6.04596748009634));
#21749=CARTESIAN_POINT('Ctrl Pts',(97.7060297300186,0.225340603502209,-6.04239883976166));
#21750=CARTESIAN_POINT('Ctrl Pts',(97.6946867557502,0.28086263516355,-6.03883019942699));
#21751=CARTESIAN_POINT('Ctrl Pts',(97.6797160394721,0.335299933743501,-6.03526155909232));
#21752=CARTESIAN_POINT('Ctrl Pts',(97.6697147066154,0.371667301397188,-6.03287749415044));
#21753=CARTESIAN_POINT('Ctrl Pts',(97.6580953183572,0.407550950286845,-6.03049342920857));
#21754=CARTESIAN_POINT('Ctrl Pts',(97.6449097088553,0.442819110014967,-6.02810936426669));
#21755=CARTESIAN_POINT('Ctrl Pts',(97.6276440753,0.489000298829028,-6.02498759794618));
#21756=CARTESIAN_POINT('Ctrl Pts',(97.6076357168921,0.534271180751997,-6.02186583162567));
#21757=CARTESIAN_POINT('Ctrl Pts',(97.5850016737362,0.578284870056729,-6.01874406530516));
#21758=CARTESIAN_POINT('Ctrl Pts',(97.5624089541461,0.622218202415255,-6.01562799847524));
#21759=CARTESIAN_POINT('Ctrl Pts',(97.5372003063184,0.664898411212142,-6.01251193164533));
#21760=CARTESIAN_POINT('Ctrl Pts',(97.5095409883672,0.705998077202455,-6.00939586481541));
#21761=CARTESIAN_POINT('Ctrl Pts',(97.4819094985138,0.747056392732514,-6.00628293306688));
#21762=CARTESIAN_POINT('Ctrl Pts',(97.4518325243324,0.786536861185324,-6.00317000131835));
#21763=CARTESIAN_POINT('Ctrl Pts',(97.4195203777163,0.824138110558106,-6.00005706956981));
#21764=CARTESIAN_POINT('Ctrl Pts',(97.3872270000227,0.861717518765506,-5.9969459460074));
#21765=CARTESIAN_POINT('Ctrl Pts',(97.3527013785607,0.897419455662145,-5.99383482244498));
#21766=CARTESIAN_POINT('Ctrl Pts',(97.3161945573899,0.930975011159725,-5.99072369888257));
#21767=CARTESIAN_POINT('Ctrl Pts',(97.2796934185691,0.96452534367694,-5.98761305957193));
#21768=CARTESIAN_POINT('Ctrl Pts',(97.2412120962563,0.995929588346935,-5.98450242026129));
#21769=CARTESIAN_POINT('Ctrl Pts',(97.201037118162,1.02495698015608,-5.98139178095065));
#21770=CARTESIAN_POINT('Ctrl Pts',(97.1608230043676,1.05401264845363,-5.97827811146916));
#21771=CARTESIAN_POINT('Ctrl Pts',(97.118912386629,1.08068652087937,-5.97516444198767));
#21772=CARTESIAN_POINT('Ctrl Pts',(97.0756219020843,1.10479041385615,-5.97205077250619));
#21773=CARTESIAN_POINT('Ctrl Pts',(97.0323077895788,1.12890746274567,-5.96893540358287));
#21774=CARTESIAN_POINT('Ctrl Pts',(96.9876128046395,1.15045150098152,-5.96582003465955));
#21775=CARTESIAN_POINT('Ctrl Pts',(96.9418762119936,1.16928133967957,-5.96270466573624));
#21776=CARTESIAN_POINT('Ctrl Pts',(96.8960555227066,1.18814580111831,-5.95958356853175));
#21777=CARTESIAN_POINT('Ctrl Pts',(96.8491899218098,1.2042859250473,-5.95646247132727));
#21778=CARTESIAN_POINT('Ctrl Pts',(96.8016349782304,1.21761002736243,-5.95334137412279));
#21779=CARTESIAN_POINT('Ctrl Pts',(96.7797077400948,1.22375367389878,-5.95190225893315));
#21780=CARTESIAN_POINT('Ctrl Pts',(96.7576340950581,1.22929933041793,-5.95046314374352));
#21781=CARTESIAN_POINT('Ctrl Pts',(96.7354494469325,1.23424170058463,-5.94902402855388));
#21782=CARTESIAN_POINT('Ctrl Pts',(96.687325890964,1.24496282746424,-5.94590225984332));
#21783=CARTESIAN_POINT('Ctrl Pts',(96.6384691452877,1.2528886495232,-5.94278049113275));
#21784=CARTESIAN_POINT('Ctrl Pts',(96.5892337875813,1.25792804114776,-5.93965872242218));
#21785=CARTESIAN_POINT('Ctrl Pts',(96.5400882948944,1.26295823480874,-5.93654265160474));
#21786=CARTESIAN_POINT('Ctrl Pts',(96.4905661015313,1.26511239186726,-5.93342658078729));
#21787=CARTESIAN_POINT('Ctrl Pts',(96.4410317718191,1.26435041799516,-5.93031050996984));
#21788=CARTESIAN_POINT('Ctrl Pts',(96.391547262928,1.26358921050395,-5.92719757324562));
#21789=CARTESIAN_POINT('Ctrl Pts',(96.3420511871433,1.25991768706299,-5.92408463652139));
#21790=CARTESIAN_POINT('Ctrl Pts',(96.2929108537378,1.25334772229435,-5.92097169979716));
#21791=CARTESIAN_POINT('Ctrl Pts',(96.2437990486393,1.24678157170357,-5.91786057028115));
#21792=CARTESIAN_POINT('Ctrl Pts',(96.1950431188634,1.23732038594117,-5.91474944076514));
#21793=CARTESIAN_POINT('Ctrl Pts',(96.1470053850065,1.22502788556717,-5.91163831124912));
#21794=CARTESIAN_POINT('Ctrl Pts',(96.0989751133304,1.21273729471001,-5.90852766501593));
#21795=CARTESIAN_POINT('Ctrl Pts',(96.0516633463213,1.19761639932997,-5.90541701878273));
#21796=CARTESIAN_POINT('Ctrl Pts',(96.0054197897736,1.17977946703543,-5.90230637254954));
#21797=CARTESIAN_POINT('Ctrl Pts',(95.9591311650348,1.16192515116717,-5.89919269473293));
#21798=CARTESIAN_POINT('Ctrl Pts',(95.9139133408995,1.14134971247037,-5.89607901691631));
#21799=CARTESIAN_POINT('Ctrl Pts',(95.8700967587827,1.1182158813307,-5.8929653390997));
#21800=CARTESIAN_POINT('Ctrl Pts',(95.8262562500839,1.09506941767883,-5.88984996102113));
#21801=CARTESIAN_POINT('Ctrl Pts',(95.7838189760765,1.06936206392372,-5.88673458294256));
#21802=CARTESIAN_POINT('Ctrl Pts',(95.7430883335839,1.04130114977296,-5.88361920486399));
#21803=CARTESIAN_POINT('Ctrl Pts',(95.7022827840257,1.01318862924908,-5.88049809734401));
#21804=CARTESIAN_POINT('Ctrl Pts',(95.6631905617938,0.982714247378316,-5.87737698982404));
#21805=CARTESIAN_POINT('Ctrl Pts',(95.6260824662031,0.950126002666643,-5.87425588230406));
#21806=CARTESIAN_POINT('Ctrl Pts',(95.6089728688084,0.935100393350445,-5.87281681914972));
#21807=CARTESIAN_POINT('Ctrl Pts',(95.5922845603638,0.919625915480621,-5.87137775599538));
#21808=CARTESIAN_POINT('Ctrl Pts',(95.5760412892255,0.903729349527431,-5.86993869284105));
#21809=CARTESIAN_POINT('Ctrl Pts',(95.5408058308823,0.86924597590934,-5.86681702791309));
#21810=CARTESIAN_POINT('Ctrl Pts',(95.5075130071989,0.83262338358838,-5.86369536298514));
#21811=CARTESIAN_POINT('Ctrl Pts',(95.476432611124,0.794109008630289,-5.86057369805718));
#21812=CARTESIAN_POINT('Ctrl Pts',(95.4454089666294,0.755664959405491,-5.85745773316656));
#21813=CARTESIAN_POINT('Ctrl Pts',(95.416590078647,0.715336401819541,-5.85434176827594));
#21814=CARTESIAN_POINT('Ctrl Pts',(95.3902084202193,0.673406981625764,-5.85122580338532));
#21815=CARTESIAN_POINT('Ctrl Pts',(95.363853307394,0.631519751414812,-5.84811297382317));
#21816=CARTESIAN_POINT('Ctrl Pts',(95.3399308595048,0.588035309205129,-5.84500014426103));
#21817=CARTESIAN_POINT('Ctrl Pts',(95.3186314929228,0.543267952615101,-5.84188731469889));
#21818=CARTESIAN_POINT('Ctrl Pts',(95.2973444990861,0.49852660126295,-5.83877629337112));
#21819=CARTESIAN_POINT('Ctrl Pts',(95.2786778027759,0.452504305890089,-5.83566527204336));
#21820=CARTESIAN_POINT('Ctrl Pts',(95.2627756474578,0.405539466976549,-5.8325542507156));
#21821=CARTESIAN_POINT('Ctrl Pts',(95.2468759666513,0.358581936194128,-5.82944371348939));
#21822=CARTESIAN_POINT('Ctrl Pts',(95.2337401473019,0.310682672174865,-5.82633317626319));
#21823=CARTESIAN_POINT('Ctrl Pts',(95.2234631880207,0.262197077776006,-5.82322263903698));
#21824=CARTESIAN_POINT('Ctrl Pts',(95.2131762138703,0.213664234295621,-5.82010907060061));
#21825=CARTESIAN_POINT('Ctrl Pts',(95.2057537744342,0.164544457014021,-5.81699550216423));
#21826=CARTESIAN_POINT('Ctrl Pts',(95.2012397426371,0.115203440679689,-5.81388193372785));
#21827=CARTESIAN_POINT('Ctrl Pts',(95.1967232463436,0.0658354859542773,
-5.81076666539694));
#21828=CARTESIAN_POINT('Ctrl Pts',(95.1951183372384,0.0162465998345455,
-5.80765139706602));
#21829=CARTESIAN_POINT('Ctrl Pts',(95.1964167562349,-0.0331958598393275,
-5.80453612873511));
#21830=CARTESIAN_POINT('Ctrl Pts',(95.1977175635096,-0.0827292626881025,
-5.80141513026062));
#21831=CARTESIAN_POINT('Ctrl Pts',(95.2019323095765,-0.132115155493617,
-5.79829413178612));
#21832=CARTESIAN_POINT('Ctrl Pts',(95.2090008683741,-0.180991315682097,
-5.79517313331163));
#21833=CARTESIAN_POINT('Ctrl Pts',(95.2122620674417,-0.203541158245179,
-5.79373320791717));
#21834=CARTESIAN_POINT('Ctrl Pts',(95.2161300120375,-0.225982649975628,
-5.7922932825227));
#21835=CARTESIAN_POINT('Ctrl Pts',(95.2205951934307,-0.248281214967158,
-5.79085335712823));
#21836=CARTESIAN_POINT('Ctrl Pts',(95.230275754311,-0.296624741675626,-5.7877315835167));
#21837=CARTESIAN_POINT('Ctrl Pts',(95.2428091104538,-0.344506970635032,
-5.78460980990517));
#21838=CARTESIAN_POINT('Ctrl Pts',(95.2581350348987,-0.391566790543403,
-5.78148803629364));
#21839=CARTESIAN_POINT('Ctrl Pts',(95.2734329771468,-0.438540688251809,
-5.77837196244162));
#21840=CARTESIAN_POINT('Ctrl Pts',(95.29151320669,-0.484694638242805,-5.77525588858961));
#21841=CARTESIAN_POINT('Ctrl Pts',(95.3122647913799,-0.529679057595407,
-5.7721398147376));
#21842=CARTESIAN_POINT('Ctrl Pts',(95.33299549677,-0.574618215673058,-5.76902687613724));
#21843=CARTESIAN_POINT('Ctrl Pts',(95.356392007711,-0.618389677535496,-5.76591393753689));
#21844=CARTESIAN_POINT('Ctrl Pts',(95.3822947611965,-0.660662389716154,
-5.76280099893653));
#21845=CARTESIAN_POINT('Ctrl Pts',(95.4081824672949,-0.702910544899029,
-5.7596898686996));
#21846=CARTESIAN_POINT('Ctrl Pts',(95.4365732457597,-0.743661208963535,
-5.75657873846266));
#21847=CARTESIAN_POINT('Ctrl Pts',(95.4672621461119,-0.782608879609272,
-5.75346760822573));
#21848=CARTESIAN_POINT('Ctrl Pts',(95.4979462678733,-0.821550485685259,
-5.75035696242511));
#21849=CARTESIAN_POINT('Ctrl Pts',(95.5309274612286,-0.858689226303311,
-5.7472463166245));
#21850=CARTESIAN_POINT('Ctrl Pts',(95.5659596632987,-0.893751597702029,
-5.74413567082388));
#21851=CARTESIAN_POINT('Ctrl Pts',(95.6010259877152,-0.928848120833089,
-5.74102199516709));
#21852=CARTESIAN_POINT('Ctrl Pts',(95.6381469203801,-0.961863849577999,
-5.73790831951029));
#21853=CARTESIAN_POINT('Ctrl Pts',(95.6770398840342,-0.992562515321442,
-5.73479464385349));
#21854=CARTESIAN_POINT('Ctrl Pts',(95.7159540733096,-1.02327793469302,-5.73167926892531));
#21855=CARTESIAN_POINT('Ctrl Pts',(95.7566417695088,-1.0516734592561,-5.72856389399714));
#21856=CARTESIAN_POINT('Ctrl Pts',(95.7987905632667,-1.07755560537013,-5.72544851906896));
#21857=CARTESIAN_POINT('Ctrl Pts',(95.8410168522527,-1.10348533867793,-5.72232741617875));
#21858=CARTESIAN_POINT('Ctrl Pts',(95.8847091167622,-1.12689221264401,-5.71920631328853));
#21859=CARTESIAN_POINT('Ctrl Pts',(95.9295309575404,-1.14762901495052,-5.71608521039832));
#21860=CARTESIAN_POINT('Ctrl Pts',(95.9501971946589,-1.15719023925783,-5.71464614740402));
#21861=CARTESIAN_POINT('Ctrl Pts',(95.9711033049277,-1.16618451330883,-5.71320708440971));
#21862=CARTESIAN_POINT('Ctrl Pts',(95.9922151859794,-1.17460096400538,-5.71176802141541));
#21863=CARTESIAN_POINT('Ctrl Pts',(96.0012843060533,-1.17821645434352,-5.71114983703585));
#21864=CARTESIAN_POINT('Ctrl Pts',(96.01039921241,-1.18172846338418,-5.7105316526563));
#21865=CARTESIAN_POINT('Ctrl Pts',(96.019557376503,-1.18513571067102,-5.70991346827675));
#21866=CARTESIAN_POINT('Ctrl Pts',(96.0195573766758,-1.18513571073528,-5.84684438197146));
#21867=CARTESIAN_POINT('Ctrl Pts',(95.9377838466584,-1.15471229449914,-5.85184356523696));
#21868=CARTESIAN_POINT('Ctrl Pts',(95.8593871237074,-1.11591032677119,-5.85675766807886));
#21869=CARTESIAN_POINT('Ctrl Pts',(95.7666978890307,-1.05741469043846,-5.8634180233614));
#21870=CARTESIAN_POINT('Ctrl Pts',(95.7480997743689,-1.04497545225213,-5.86480253184938));
#21871=CARTESIAN_POINT('Ctrl Pts',(95.7109005660367,-1.01864033194169,-5.86769259545907));
#21872=CARTESIAN_POINT('Ctrl Pts',(95.6923328699123,-1.00471250834484,-5.86919957672916));
#21873=CARTESIAN_POINT('Ctrl Pts',(95.6261344841347,-0.952148598586737,
-5.87478053896405));
#21874=CARTESIAN_POINT('Ctrl Pts',(95.5809499334651,-0.910573991331859,
-5.87899390296784));
#21875=CARTESIAN_POINT('Ctrl Pts',(95.4774791070059,-0.800455833223651,
-5.88938625455785));
#21876=CARTESIAN_POINT('Ctrl Pts',(95.4231293829763,-0.728648634844923,
-5.89552426270106));
#21877=CARTESIAN_POINT('Ctrl Pts',(95.3582414461938,-0.620750264390375,
-5.90372158879092));
#21878=CARTESIAN_POINT('Ctrl Pts',(95.3409726780465,-0.589036907625956,
-5.90602447030197));
#21879=CARTESIAN_POINT('Ctrl Pts',(95.3087872286146,-0.52338538632302,-5.91059300222629));
#21880=CARTESIAN_POINT('Ctrl Pts',(95.2939579424961,-0.489443754131257,
-5.91285390519707));
#21881=CARTESIAN_POINT('Ctrl Pts',(95.2660535381213,-0.417069615502774,
-5.91750072706743));
#21882=CARTESIAN_POINT('Ctrl Pts',(95.2532957123027,-0.378560547984007,
-5.91987519370583));
#21883=CARTESIAN_POINT('Ctrl Pts',(95.2172438834632,-0.249213356459102,
-5.92764290854262));
#21884=CARTESIAN_POINT('Ctrl Pts',(95.2021975041997,-0.156414919864184,
-5.93286805880145));
#21885=CARTESIAN_POINT('Ctrl Pts',(95.1961020405665,-0.0338615463724993,
-5.94015787448968));
#21886=CARTESIAN_POINT('Ctrl Pts',(95.1956581871163,-0.00486958004534194,
-5.94191245365027));
#21887=CARTESIAN_POINT('Ctrl Pts',(95.1965952834404,0.0442708302043974,
-5.94497541410896));
#21888=CARTESIAN_POINT('Ctrl Pts',(95.197461846205,0.0644161774360809,-5.94625847331155));
#21889=CARTESIAN_POINT('Ctrl Pts',(95.2012630394973,0.121150615412437,-5.94994548629421));
#21890=CARTESIAN_POINT('Ctrl Pts',(95.2053093715755,0.157642023163297,-5.95239915052863));
#21891=CARTESIAN_POINT('Ctrl Pts',(95.2204363873285,0.255123649668902,-5.95909101875221));
#21892=CARTESIAN_POINT('Ctrl Pts',(95.2344229438567,0.315563431192348,-5.96338255967212));
#21893=CARTESIAN_POINT('Ctrl Pts',(95.2727827406317,0.439189877247954,-5.9722399254486));
#21894=CARTESIAN_POINT('Ctrl Pts',(95.2979127922853,0.501948616771625,-5.97677995814351));
#21895=CARTESIAN_POINT('Ctrl Pts',(95.3436918443134,0.594135635105346,-5.98345564412554));
#21896=CARTESIAN_POINT('Ctrl Pts',(95.3607743043712,0.625188582668533,-5.98570740020361));
#21897=CARTESIAN_POINT('Ctrl Pts',(95.3989251941076,0.688125293286197,-5.99029053299647));
#21898=CARTESIAN_POINT('Ctrl Pts',(95.4201794543918,0.71985435728773,-5.99261207810089));
#21899=CARTESIAN_POINT('Ctrl Pts',(95.468313267508,0.785114926358987,-5.997450063231));
#21900=CARTESIAN_POINT('Ctrl Pts',(95.4955311572602,0.818336401419655,-5.99995141032774));
#21901=CARTESIAN_POINT('Ctrl Pts',(95.5819243249958,0.91346759310317,-6.00735903496852));
#21902=CARTESIAN_POINT('Ctrl Pts',(95.6457396576691,0.97081369771625,-6.0121541974527));
#21903=CARTESIAN_POINT('Ctrl Pts',(95.7390211249825,1.03891846894308,-6.01900113372312));
#21904=CARTESIAN_POINT('Ctrl Pts',(95.763808204436,1.05570006645382,-6.02080853851395));
#21905=CARTESIAN_POINT('Ctrl Pts',(95.8062295325529,1.08227576279618,-6.02392352745981));
#21906=CARTESIAN_POINT('Ctrl Pts',(95.8235436910789,1.09255503491885,-6.02520255811905));
#21907=CARTESIAN_POINT('Ctrl Pts',(95.8719328175188,1.1197421330204,-6.02879632178875));
#21908=CARTESIAN_POINT('Ctrl Pts',(95.9034804230934,1.13576462552936,-6.03115591766485));
#21909=CARTESIAN_POINT('Ctrl Pts',(95.9880121159412,1.17432757435207,-6.0374468266035));
#21910=CARTESIAN_POINT('Ctrl Pts',(96.0419377967847,1.19461016973284,-6.04142594787677));
#21911=CARTESIAN_POINT('Ctrl Pts',(96.1671680275022,1.23218750924559,-6.05038958391888));
#21912=CARTESIAN_POINT('Ctrl Pts',(96.2389831311708,1.24710070499728,-6.05533117020251));
#21913=CARTESIAN_POINT('Ctrl Pts',(96.3469719648906,1.25989599374294,-6.06238661115841));
#21914=CARTESIAN_POINT('Ctrl Pts',(96.3824122021595,1.26258777491013,-6.0646455922689));
#21915=CARTESIAN_POINT('Ctrl Pts',(96.455951841438,1.26506428838531,-6.06922918432197));
#21916=CARTESIAN_POINT('Ctrl Pts',(96.4940227306363,1.26462783763334,-6.07154456956882));
#21917=CARTESIAN_POINT('Ctrl Pts',(96.5745983377002,1.26006201217088,-6.07636138045156));
#21918=CARTESIAN_POINT('Ctrl Pts',(96.6170303053683,1.25549661871334,-6.07884816573145));
#21919=CARTESIAN_POINT('Ctrl Pts',(96.7470579101663,1.23481042456195,-6.08643997120845));
#21920=CARTESIAN_POINT('Ctrl Pts',(96.8332323465718,1.211584461685,-6.09141822937776));
#21921=CARTESIAN_POINT('Ctrl Pts',(96.9428302335981,1.16923549102459,-6.09840733162763));
#21922=CARTESIAN_POINT('Ctrl Pts',(96.9690569000964,1.15806851391745,-6.10013441287575));
#21923=CARTESIAN_POINT('Ctrl Pts',(97.0131263763159,1.13751858671315,-6.10316734832646));
#21924=CARTESIAN_POINT('Ctrl Pts',(97.0311617532308,1.12857819228048,-6.1044494106973));
#21925=CARTESIAN_POINT('Ctrl Pts',(97.0818731551988,1.10191353999248,-6.10816764326997));
#21926=CARTESIAN_POINT('Ctrl Pts',(97.1139890613338,1.08317511718216,-6.11065552838991));
#21927=CARTESIAN_POINT('Ctrl Pts',(97.1987493423038,1.02857804891638,-6.11750267408036));
#21928=CARTESIAN_POINT('Ctrl Pts',(97.2495884526673,0.990112297282799,-6.12191768364368));
#21929=CARTESIAN_POINT('Ctrl Pts',(97.3464868594598,0.90457495238809,-6.13075922085882));
#21930=CARTESIAN_POINT('Ctrl Pts',(97.3922129356389,0.857403063605749,-6.13516772027039));
#21931=CARTESIAN_POINT('Ctrl Pts',(97.4565573496004,0.779764804595199,-6.14170750247376));
#21932=CARTESIAN_POINT('Ctrl Pts',(97.477895688305,0.751710716185097,-6.14394683067393));
#21933=CARTESIAN_POINT('Ctrl Pts',(97.5197265934111,0.691663803997951,-6.14850393876889));
#21934=CARTESIAN_POINT('Ctrl Pts',(97.5400058417601,0.659565469658199,-6.15081201112935));
#21935=CARTESIAN_POINT('Ctrl Pts',(97.5799267063304,0.589590556856843,-6.15561839570102));
#21936=CARTESIAN_POINT('Ctrl Pts',(97.5991580455471,0.551534862638533,-6.15810190201137));
#21937=CARTESIAN_POINT('Ctrl Pts',(97.6511395788588,0.434307741591374,-6.16549311347615));
#21938=CARTESIAN_POINT('Ctrl Pts',(97.6778046639425,0.352720868597642,-6.1702873132448));
#21939=CARTESIAN_POINT('Ctrl Pts',(97.7024407616585,0.239595895572774,-6.17714447244319));
#21940=CARTESIAN_POINT('Ctrl Pts',(97.7078027341326,0.209900946158523,-6.17896487835704));
#21941=CARTESIAN_POINT('Ctrl Pts',(97.7149602514241,0.16014426766828,-6.18209117907099));
#21942=CARTESIAN_POINT('Ctrl Pts',(97.7173474675812,0.140181650018631,-6.18336751754647));
#21943=CARTESIAN_POINT('Ctrl Pts',(97.7225664287677,0.0855135013051155,
-6.18692143025161));
#21944=CARTESIAN_POINT('Ctrl Pts',(97.724442004365,0.0507376283597556,-6.18924197574226));
#21945=CARTESIAN_POINT('Ctrl Pts',(97.7255820254749,-0.0397354676565079,
-6.19536405909827));
#21946=CARTESIAN_POINT('Ctrl Pts',(97.7226063916071,-0.0953872984476596,
-6.19921099590677));
#21947=CARTESIAN_POINT('Ctrl Pts',(97.7068658677574,-0.226557147900269,
-6.20827732408373));
#21948=CARTESIAN_POINT('Ctrl Pts',(97.6908937181905,-0.301481694010448,
-6.21344744300113));
#21949=CARTESIAN_POINT('Ctrl Pts',(97.6576854221984,-0.408574855025839,
-6.22072325557859));
#21950=CARTESIAN_POINT('Ctrl Pts',(97.6456866098355,-0.442176346821572,
-6.22299125162701));
#21951=CARTESIAN_POINT('Ctrl Pts',(97.617888710023,-0.510719390393977,-6.22759943193466));
#21952=CARTESIAN_POINT('Ctrl Pts',(97.6018893822474,-0.545540344791768,
-6.22993004210697));
#21953=CARTESIAN_POINT('Ctrl Pts',(97.5646035255323,-0.617840052266742,
-6.23478583766901));
#21954=CARTESIAN_POINT('Ctrl Pts',(97.5429330567653,-0.655065524087496,
-6.23729592838875));
#21955=CARTESIAN_POINT('Ctrl Pts',(97.4726103156454,-0.762813743163785,
-6.24471738087989));
#21956=CARTESIAN_POINT('Ctrl Pts',(97.4186589182231,-0.829568245543577,
-6.24951843919097));
#21957=CARTESIAN_POINT('Ctrl Pts',(97.3373178329375,-0.91159879349207,-6.25637095018362));
#21958=CARTESIAN_POINT('Ctrl Pts',(97.3155072984659,-0.932086318659482,
-6.25817867576091));
#21959=CARTESIAN_POINT('Ctrl Pts',(97.2776214913067,-0.965224658932037,
-6.26131178079223));
#21960=CARTESIAN_POINT('Ctrl Pts',(97.2619296914768,-0.978292919070695,
-6.26260962424126));
#21961=CARTESIAN_POINT('Ctrl Pts',(97.2166900299023,-1.01414991250018,-6.26634822695243));
#21962=CARTESIAN_POINT('Ctrl Pts',(97.1864425977976,-1.0360170729478,-6.26883956726225));
#21963=CARTESIAN_POINT('Ctrl Pts',(97.1015948146238,-1.09181555285675,-6.2757169391872));
#21964=CARTESIAN_POINT('Ctrl Pts',(97.045301538233,-1.12297512068837,-6.28015755047713));
#21965=CARTESIAN_POINT('Ctrl Pts',(96.9301258788272,-1.17570859017423,-6.28878601985194));
#21966=CARTESIAN_POINT('Ctrl Pts',(96.8715153220139,-1.19745966678565,-6.292965596508));
#21967=CARTESIAN_POINT('Ctrl Pts',(96.7773748366626,-1.22466425812783,-6.29931090150239));
#21968=CARTESIAN_POINT('Ctrl Pts',(96.7428156740292,-1.23309034363115,-6.30156745581243));
#21969=CARTESIAN_POINT('Ctrl Pts',(96.6699170171589,-1.24763794538777,-6.30618972399131));
#21970=CARTESIAN_POINT('Ctrl Pts',(96.6315583150243,-1.25347393923124,-6.30854417833269));
#21971=CARTESIAN_POINT('Ctrl Pts',(96.5492967749851,-1.26214190166454,-6.31346999376593));
#21972=CARTESIAN_POINT('Ctrl Pts',(96.505392398636,-1.26446582306308,-6.31602491438671));
#21973=CARTESIAN_POINT('Ctrl Pts',(96.3760774890712,-1.26456530719757,-6.32346611019265));
#21974=CARTESIAN_POINT('Ctrl Pts',(96.2909218307323,-1.25598436430066,-6.32824871607656));
#21975=CARTESIAN_POINT('Ctrl Pts',(96.1785977465977,-1.23302863673213,-6.33505754105091));
#21976=CARTESIAN_POINT('Ctrl Pts',(96.150122379193,-1.22617087271748,-6.33682981368999));
#21977=CARTESIAN_POINT('Ctrl Pts',(96.1031907638755,-1.21312883842954,-6.3398668267478));
#21978=CARTESIAN_POINT('Ctrl Pts',(96.0845945013905,-1.20749621547019,-6.34110276829313));
#21979=CARTESIAN_POINT('Ctrl Pts',(96.0505020436517,-1.19630608524143,-6.34343061982689));
#21980=CARTESIAN_POINT('Ctrl Pts',(96.0349733858114,-1.1908711566551,-6.34451408366555));
#21981=CARTESIAN_POINT('Ctrl Pts',(96.0195573796018,-1.18513571182389,-6.34560991122238));
#21982=CARTESIAN_POINT('Origin',(96.460480949577,-1.76391462320204E-15,
-7.60421172358872));
#21983=CARTESIAN_POINT('',(98.0034803719728,-0.00133509777570635,-5.85421172355731));
#21984=CARTESIAN_POINT('Ctrl Pts',(95.5205266553345,1.22365637526844,-6.17704955921195));
#21985=CARTESIAN_POINT('Ctrl Pts',(95.4750360039568,1.18871263291183,-6.17408432509521));
#21986=CARTESIAN_POINT('Ctrl Pts',(95.431424748673,1.15117353037341,-6.17111909097847));
#21987=CARTESIAN_POINT('Ctrl Pts',(95.3900012076878,1.11127049911566,-6.16815385686173));
#21988=CARTESIAN_POINT('Ctrl Pts',(95.3486178575488,1.07140618344223,-6.16519149973874));
#21989=CARTESIAN_POINT('Ctrl Pts',(95.309418389521,1.02918284333066,-6.16222914261575));
#21990=CARTESIAN_POINT('Ctrl Pts',(95.2726777313522,0.984871826571724,-6.15926678549276));
#21991=CARTESIAN_POINT('Ctrl Pts',(95.2359585877192,0.940586757387131,-6.15630616306211));
#21992=CARTESIAN_POINT('Ctrl Pts',(95.2016957315978,0.894216835472797,-6.15334554063147));
#21993=CARTESIAN_POINT('Ctrl Pts',(95.1701253722669,0.846068250263889,-6.15038491820082));
#21994=CARTESIAN_POINT('Ctrl Pts',(95.1385613565695,0.797929339857214,-6.14742489066692));
#21995=CARTESIAN_POINT('Ctrl Pts',(95.109689048867,0.748012911522314,-6.14446486313301));
#21996=CARTESIAN_POINT('Ctrl Pts',(95.0837014019618,0.696654202074729,-6.14150483559911));
#21997=CARTESIAN_POINT('Ctrl Pts',(95.057689999433,0.645248545007449,-6.13854210226811));
#21998=CARTESIAN_POINT('Ctrl Pts',(95.0345687627803,0.592398438366997,-6.13557936893711));
#21999=CARTESIAN_POINT('Ctrl Pts',(95.0144840397897,0.538462567766447,-6.13261663560611));
#22000=CARTESIAN_POINT('Ctrl Pts',(94.9943905569729,0.484503173373546,-6.12965261009752));
#22001=CARTESIAN_POINT('Ctrl Pts',(94.9773363829618,0.429457569615514,-6.12668858458892));
#22002=CARTESIAN_POINT('Ctrl Pts',(94.9634180905899,0.373700142148047,-6.12372455908032));
#22003=CARTESIAN_POINT('Ctrl Pts',(94.9494732659501,0.317836424988612,-6.12075488328669));
#22004=CARTESIAN_POINT('Ctrl Pts',(94.9386763655485,0.261258686260434,-6.11778520749305));
#22005=CARTESIAN_POINT('Ctrl Pts',(94.9310726844337,0.204351066822466,-6.11481553169941));
#22006=CARTESIAN_POINT('Ctrl Pts',(94.9245684531917,0.155671971700926,-6.11227525445945));
#22007=CARTESIAN_POINT('Ctrl Pts',(94.920399894136,0.106751803719814,-6.10973497721949));
#22008=CARTESIAN_POINT('Ctrl Pts',(94.9185650739381,0.0578310682319644,
-6.10719469997953));
#22009=CARTESIAN_POINT('Ctrl Pts',(94.9164199209303,0.000636110926563641,
-6.10422477226208));
#22010=CARTESIAN_POINT('Ctrl Pts',(94.9174569443836,-0.0567975521573849,
-6.10125484454463));
#22011=CARTESIAN_POINT('Ctrl Pts',(94.921704385593,-0.114086310017802,-6.09828491682718));
#22012=CARTESIAN_POINT('Ctrl Pts',(94.9259443171463,-0.171273778927885,
-6.09532024006772));
#22013=CARTESIAN_POINT('Ctrl Pts',(94.9333833618724,-0.228316335375274,
-6.09235556330827));
#22014=CARTESIAN_POINT('Ctrl Pts',(94.9439977754811,-0.284829392240432,
-6.08939088654881));
#22015=CARTESIAN_POINT('Ctrl Pts',(94.9546017033752,-0.341286621265306,
-6.08642913851963));
#22016=CARTESIAN_POINT('Ctrl Pts',(94.9683746892567,-0.397214877187807,
-6.08346739049045));
#22017=CARTESIAN_POINT('Ctrl Pts',(94.9852412891601,-0.452235496542447,
-6.08050564246127));
#22018=CARTESIAN_POINT('Ctrl Pts',(95.0020977234071,-0.507222954458717,
-6.07754567950514));
#22019=CARTESIAN_POINT('Ctrl Pts',(95.0220439230071,-0.561303362708368,
-6.07458571654901));
#22020=CARTESIAN_POINT('Ctrl Pts',(95.044954050569,-0.61411122623253,-6.07162575359288));
#22021=CARTESIAN_POINT('Ctrl Pts',(95.0678591936993,-0.666907600637633,
-6.06866643461976));
#22022=CARTESIAN_POINT('Ctrl Pts',(95.0937267770205,-0.718431501928402,
-6.06570711564663));
#22023=CARTESIAN_POINT('Ctrl Pts',(95.1223829126007,-0.768337584295006,
-6.06274779667351));
#22024=CARTESIAN_POINT('Ctrl Pts',(95.1510648986118,-0.818288686469972,
-6.05978580812652));
#22025=CARTESIAN_POINT('Ctrl Pts',(95.1825402040583,-0.866618599759192,
-6.05682381957954));
#22026=CARTESIAN_POINT('Ctrl Pts',(95.2165897224079,-0.913008003782919,
-6.05386183103255));
#22027=CARTESIAN_POINT('Ctrl Pts',(95.2506536148954,-0.959416991275864,
-6.05089859207046));
#22028=CARTESIAN_POINT('Ctrl Pts',(95.2872935552373,-1.00388343251831,-6.04793535310837));
#22029=CARTESIAN_POINT('Ctrl Pts',(95.3262499490834,-1.0461209478446,-6.04497211414628));
#22030=CARTESIAN_POINT('Ctrl Pts',(95.365281100693,-1.08843951744378,-6.04200318869488));
#22031=CARTESIAN_POINT('Ctrl Pts',(95.40663721333,-1.12852024946172,-6.03903426324348));
#22032=CARTESIAN_POINT('Ctrl Pts',(95.4500223219213,-1.16611421473036,-6.03606533779207));
#22033=CARTESIAN_POINT('Ctrl Pts',(95.4887760484797,-1.19969500541112,-6.03341334661695));
#22034=CARTESIAN_POINT('Ctrl Pts',(95.529148010317,-1.23129202170489,-6.03076135544183));
#22035=CARTESIAN_POINT('Ctrl Pts',(95.5709078972908,-1.26075722668808,-6.0281093642667));
#22036=CARTESIAN_POINT('Ctrl Pts',(95.6176788115735,-1.29375814399077,-6.0251391442561));
#22037=CARTESIAN_POINT('Ctrl Pts',(95.666385876195,-1.32422155670154,-6.02216892424549));
#22038=CARTESIAN_POINT('Ctrl Pts',(95.7167228900047,-1.35191454937851,-6.01919870423488));
#22039=CARTESIAN_POINT('Ctrl Pts',(95.7669710054558,-1.37955863447417,-6.01623372982118));
#22040=CARTESIAN_POINT('Ctrl Pts',(95.8188429034369,-1.40444176173788,-6.01326875540748));
#22041=CARTESIAN_POINT('Ctrl Pts',(95.872003214868,-1.42637405884705,-6.01030378099378));
#22042=CARTESIAN_POINT('Ctrl Pts',(95.9251110704837,-1.44828471431229,-6.00734173226178));
#22043=CARTESIAN_POINT('Ctrl Pts',(95.9795043411007,-1.46725011089183,-6.00437968352979));
#22044=CARTESIAN_POINT('Ctrl Pts',(96.0348244283148,-1.48312694193954,-6.0014176347978));
#22045=CARTESIAN_POINT('Ctrl Pts',(96.090111223882,-1.49899421830504,-5.99845736862772));
#22046=CARTESIAN_POINT('Ctrl Pts',(96.1463232303117,-1.51177647021289,-5.99549710245764));
#22047=CARTESIAN_POINT('Ctrl Pts',(96.203085403343,-1.52137981213729,-5.99253683628756));
#22048=CARTESIAN_POINT('Ctrl Pts',(96.259835266122,-1.53098107134435,-5.98957721212291));
#22049=CARTESIAN_POINT('Ctrl Pts',(96.3171345448594,-1.53740470253106,-5.98661758795826));
#22050=CARTESIAN_POINT('Ctrl Pts',(96.3745988768833,-1.5406080843582,-5.98365796379361));
#22051=CARTESIAN_POINT('Ctrl Pts',(96.432115053852,-1.54381435631123,-5.98069566942388));
#22052=CARTESIAN_POINT('Ctrl Pts',(96.4897960600159,-1.54379454334605,-5.97773337505415));
#22053=CARTESIAN_POINT('Ctrl Pts',(96.5472546827378,-1.54055811939484,-5.97477108068442));
#22054=CARTESIAN_POINT('Ctrl Pts',(96.6047375755878,-1.53732032840034,-5.97180753506187));
#22055=CARTESIAN_POINT('Ctrl Pts',(96.661997378546,-1.53086327533476,-5.96884398943931));
#22056=CARTESIAN_POINT('Ctrl Pts',(96.7186524035503,-1.52124833618752,-5.96588044381675));
#22057=CARTESIAN_POINT('Ctrl Pts',(96.7754160898408,-1.51161495610494,-5.96291121427333));
#22058=CARTESIAN_POINT('Ctrl Pts',(96.8315721702688,-1.49881170294986,-5.95994198472991));
#22059=CARTESIAN_POINT('Ctrl Pts',(96.8867505062524,-1.48295086400454,-5.95697275518648));
#22060=CARTESIAN_POINT('Ctrl Pts',(96.9359885888775,-1.46879753218377,-5.95432317964228));
#22061=CARTESIAN_POINT('Ctrl Pts',(96.984448079226,-1.45221031159443,-5.95167360409808));
#22062=CARTESIAN_POINT('Ctrl Pts',(97.031879979471,-1.43330113675956,-5.94902402855388));
#22063=CARTESIAN_POINT('Ctrl Pts',(97.085052000573,-1.41210360855282,-5.94605380627688));
#22064=CARTESIAN_POINT('Ctrl Pts',(97.1371534399318,-1.3878991580331,-5.94308358399989));
#22065=CARTESIAN_POINT('Ctrl Pts',(97.1878220574034,-1.3608173694019,-5.94011336172289));
#22066=CARTESIAN_POINT('Ctrl Pts',(97.2384012160943,-1.33378339545187,-5.93714838356891));
#22067=CARTESIAN_POINT('Ctrl Pts',(97.2875521180855,-1.30388241050893,-5.93418340541494));
#22068=CARTESIAN_POINT('Ctrl Pts',(97.3349326881829,-1.27129192432311,-5.93121842726096));
#22069=CARTESIAN_POINT('Ctrl Pts',(97.3822665199763,-1.23873358684393,-5.92825637389345));
#22070=CARTESIAN_POINT('Ctrl Pts',(97.4278330525774,-1.20349129864964,-5.92529432052594));
#22071=CARTESIAN_POINT('Ctrl Pts',(97.4713165676437,-1.16578743913617,-5.92233226715843));
#22072=CARTESIAN_POINT('Ctrl Pts',(97.5147739273687,-1.12810625850026,-5.91937199546649));
#22073=CARTESIAN_POINT('Ctrl Pts',(97.5561503602495,-1.08796678250313,-5.91641172377456));
#22074=CARTESIAN_POINT('Ctrl Pts',(97.5951625982189,-1.0456321323655,-5.91345145208262));
#22075=CARTESIAN_POINT('Ctrl Pts',(97.6341663870328,-1.00330665094165,-5.91049182151761));
#22076=CARTESIAN_POINT('Ctrl Pts',(97.6708066445105,-0.95878732250894,-5.90753219095259));
#22077=CARTESIAN_POINT('Ctrl Pts',(97.7048379854176,-0.912373041772958,
-5.90457256038758));
#22078=CARTESIAN_POINT('Ctrl Pts',(97.7389000450271,-0.865916864760098,
-5.90161025828485));
#22079=CARTESIAN_POINT('Ctrl Pts',(97.7703481726039,-0.817562738317025,
-5.89864795618211));
#22080=CARTESIAN_POINT('Ctrl Pts',(97.7989790905744,-0.767640362765306,
-5.89568565407938));
#22081=CARTESIAN_POINT('Ctrl Pts',(97.8276221092052,-0.717696887865466,
-5.89272209998007));
#22082=CARTESIAN_POINT('Ctrl Pts',(97.8534453095478,-0.666184309021905,
-5.88975854588076));
#22083=CARTESIAN_POINT('Ctrl Pts',(97.8762919280009,-0.613456007692871,
-5.88679499178145));
#22084=CARTESIAN_POINT('Ctrl Pts',(97.8991823737796,-0.560626556145983,
-5.88382575261103));
#22085=CARTESIAN_POINT('Ctrl Pts',(97.9190846462876,-0.50657721251163,-5.88085651344061));
#22086=CARTESIAN_POINT('Ctrl Pts',(97.9358909518878,-0.45167944947849,-5.87788727427019));
#22087=CARTESIAN_POINT('Ctrl Pts',(97.9508876430623,-0.402692788283397,
-5.87523774712714));
#22088=CARTESIAN_POINT('Ctrl Pts',(97.9634198405777,-0.35303104463705,-5.8725882199841));
#22089=CARTESIAN_POINT('Ctrl Pts',(97.9734455377117,-0.302963950083964,
-5.86993869284106));
#22090=CARTESIAN_POINT('Ctrl Pts',(97.9895138161738,-0.222720949889708,
-5.86569227093558));
#22091=CARTESIAN_POINT('Ctrl Pts',(97.9992020858234,-0.141160850084212,
-5.8614458490301));
#22092=CARTESIAN_POINT('Ctrl Pts',(98.0023478318077,-0.0591229014857949,
-5.85719942712462));
#22093=CARTESIAN_POINT('Ctrl Pts',(98.0030855946121,-0.0398827761472533,
-5.85620352594598));
#22094=CARTESIAN_POINT('Ctrl Pts',(98.003463688527,-0.0206164838043829,
-5.85520762476735));
#22095=CARTESIAN_POINT('Ctrl Pts',(98.0034803719723,-0.00133509838387759,
-5.85421172358872));
#22096=CARTESIAN_POINT('Ctrl Pts',(98.0034803719729,-0.00133509777570635,
-5.85421172355731));
#22097=CARTESIAN_POINT('Ctrl Pts',(98.003529319685,0.0552347602601169,-5.85128983868941));
#22098=CARTESIAN_POINT('Ctrl Pts',(98.0004630541371,0.111904542497342,-5.84836795382152));
#22099=CARTESIAN_POINT('Ctrl Pts',(97.9942751962306,0.16829797661396,-5.84544606895362));
#22100=CARTESIAN_POINT('Ctrl Pts',(97.9880929098134,0.224640634610309,-5.84252681492351));
#22101=CARTESIAN_POINT('Ctrl Pts',(97.9787946528756,0.280706904815718,-5.8396075608934));
#22102=CARTESIAN_POINT('Ctrl Pts',(97.9664260609476,0.336122479966725,-5.83668830686329));
#22103=CARTESIAN_POINT('Ctrl Pts',(97.9540635171348,0.391510957467202,-5.8337704803186));
#22104=CARTESIAN_POINT('Ctrl Pts',(97.9386337296698,0.446248846150917,-5.83085265377392));
#22105=CARTESIAN_POINT('Ctrl Pts',(97.9202335485138,0.499971349076287,-5.82793482722923));
#22106=CARTESIAN_POINT('Ctrl Pts',(97.9018347962476,0.553689680111704,-5.82501722727211));
#22107=CARTESIAN_POINT('Ctrl Pts',(97.8804662849714,0.606392274179094,-5.82209962731498));
#22108=CARTESIAN_POINT('Ctrl Pts',(97.8562741596734,0.657731187225284,-5.81918202735786));
#22109=CARTESIAN_POINT('Ctrl Pts',(97.8320584704108,0.709120106143976,-5.81626158555772));
#22110=CARTESIAN_POINT('Ctrl Pts',(97.80501391234,0.759142208116028,-5.81334114375759));
#22111=CARTESIAN_POINT('Ctrl Pts',(97.7753333147438,0.807472759797698,-5.81042070195745));
#22112=CARTESIAN_POINT('Ctrl Pts',(97.7456350511605,0.855832077979083,-5.80749852190096));
#22113=CARTESIAN_POINT('Ctrl Pts',(97.7132979367514,0.902497403768863,-5.80457634184448));
#22114=CARTESIAN_POINT('Ctrl Pts',(97.6785570974921,0.947174481223082,-5.801654161788));
#22115=CARTESIAN_POINT('Ctrl Pts',(97.6437576822231,0.991926888029769,-5.7987270546874));
#22116=CARTESIAN_POINT('Ctrl Pts',(97.6065468178134,1.0346839619332,-5.7957999475868));
#22117=CARTESIAN_POINT('Ctrl Pts',(97.5671975262562,1.07518715529138,-5.7928728404862));
#22118=CARTESIAN_POINT('Ctrl Pts',(97.558148177449,1.08450187253272,-5.79219967936688));
#22119=CARTESIAN_POINT('Ctrl Pts',(97.548985869182,1.09369755351201,-5.79152651824756));
#22120=CARTESIAN_POINT('Ctrl Pts',(97.539714160954,1.10277136137139,-5.79085335712823));
#22121=CARTESIAN_POINT('Ctrl Pts',(97.4988040775081,1.14280823780976,-5.78788313018766));
#22122=CARTESIAN_POINT('Ctrl Pts',(97.4555779765147,1.18064881807926,-5.78491290324709));
#22123=CARTESIAN_POINT('Ctrl Pts',(97.4103009999711,1.21601433867756,-5.78194267630652));
#22124=CARTESIAN_POINT('Ctrl Pts',(97.3651039890387,1.25131739871226,-5.77897769521121));
#22125=CARTESIAN_POINT('Ctrl Pts',(97.3178636995138,1.28415375726168,-5.7760127141159));
#22126=CARTESIAN_POINT('Ctrl Pts',(97.2688809318777,1.31428249193853,-5.77304773302059));
#22127=CARTESIAN_POINT('Ctrl Pts',(97.2199465003075,1.34438149565954,-5.7700856777608));
#22128=CARTESIAN_POINT('Ctrl Pts',(97.1692734392942,1.37177789762699,-5.76712362250101));
#22129=CARTESIAN_POINT('Ctrl Pts',(97.1171929069576,1.39627304100358,-5.76416156724122));
#22130=CARTESIAN_POINT('Ctrl Pts',(97.0651437194437,1.42075344190551,-5.76120129470317));
#22131=CARTESIAN_POINT('Ctrl Pts',(97.0116892106127,1.44233582423702,-5.75824102216512));
#22132=CARTESIAN_POINT('Ctrl Pts',(96.9571846549207,1.4608676973285,-5.75528074962707));
#22133=CARTESIAN_POINT('Ctrl Pts',(96.9026919228934,1.47939555030363,-5.75232111926048));
#22134=CARTESIAN_POINT('Ctrl Pts',(96.847150089584,1.49487404023915,-5.74936148889388));
#22135=CARTESIAN_POINT('Ctrl Pts',(96.7909318034718,1.50719979868635,-5.74640185852729));
#22136=CARTESIAN_POINT('Ctrl Pts',(96.7346628023357,1.51953667631163,-5.7434395582514));
#22137=CARTESIAN_POINT('Ctrl Pts',(96.677716639199,1.52871502645337,-5.74047725797551));
#22138=CARTESIAN_POINT('Ctrl Pts',(96.6204770833966,1.53468245482991,-5.73751495769962));
#22139=CARTESIAN_POINT('Ctrl Pts',(96.5632133529976,1.5406524034946,-5.73455140632363));
#22140=CARTESIAN_POINT('Ctrl Pts',(96.5056565046217,1.5434087009063,-5.73158785494763));
#22141=CARTESIAN_POINT('Ctrl Pts',(96.4481931303532,1.54295107164768,-5.72862430357164));
#22142=CARTESIAN_POINT('Ctrl Pts',(96.3906195508084,1.5424925647316,-5.72565506859278));
#22143=CARTESIAN_POINT('Ctrl Pts',(96.333140325593,1.53880784726999,-5.72268583361393));
#22144=CARTESIAN_POINT('Ctrl Pts',(96.2761387637044,1.53194874539186,-5.71971659863507));
#22145=CARTESIAN_POINT('Ctrl Pts',(96.2252747847625,1.52582819006092,-5.71706707289519));
#22146=CARTESIAN_POINT('Ctrl Pts',(96.1747913058088,1.51718083018387,-5.7144175471553));
#22147=CARTESIAN_POINT('Ctrl Pts',(96.1249519726324,1.5060774567168,-5.71176802141541));
#22148=CARTESIAN_POINT('Ctrl Pts',(96.0690995587969,1.4936344690135,-5.70879883224972));
#22149=CARTESIAN_POINT('Ctrl Pts',(96.0138241261216,1.47805450256403,-5.70582964308403));
#22150=CARTESIAN_POINT('Ctrl Pts',(95.9595035514066,1.45940763548859,-5.70286045391834));
#22151=CARTESIAN_POINT('Ctrl Pts',(95.9052573561847,1.44078630099503,-5.6998953303721));
#22152=CARTESIAN_POINT('Ctrl Pts',(95.8519639179068,1.41910655099664,-5.69693020682586));
#22153=CARTESIAN_POINT('Ctrl Pts',(95.7999893008411,1.39448907559369,-5.69396508327963));
#22154=CARTESIAN_POINT('Ctrl Pts',(95.7480668880911,1.36989632646156,-5.69100293796112));
#22155=CARTESIAN_POINT('Ctrl Pts',(95.6974611404136,1.34237192135134,-5.68804079264261));
#22156=CARTESIAN_POINT('Ctrl Pts',(95.6485192377665,1.31208505004585,-5.6850786473241));
#22157=CARTESIAN_POINT('Ctrl Pts',(95.6044256191205,1.2847984575536,-5.68240993812024));
#22158=CARTESIAN_POINT('Ctrl Pts',(95.5616825337404,1.25527035238062,-5.67974122891638));
#22159=CARTESIAN_POINT('Ctrl Pts',(95.5205266553345,1.22365637526844,-5.67707251971253));
#22160=CARTESIAN_POINT('',(98.0034806047664,0.00103154524370014,-5.89578827637723));
#22161=CARTESIAN_POINT('Ctrl Pts',(98.0034806047663,0.00103154524370189,
-5.89578827637723));
#22162=CARTESIAN_POINT('Ctrl Pts',(98.0034368144072,0.0665337706066547,
-5.89242239470813));
#22163=CARTESIAN_POINT('Ctrl Pts',(97.9992179907216,0.131874306095174,-5.88905651303903));
#22164=CARTESIAN_POINT('Ctrl Pts',(97.9909097815011,0.196561925141776,-5.88569063136993));
#22165=CARTESIAN_POINT('Ctrl Pts',(97.9825300313629,0.261806560930387,-5.88229576652803));
#22166=CARTESIAN_POINT('Ctrl Pts',(97.9699902874583,0.326386762739351,-5.87890090168612));
#22167=CARTESIAN_POINT('Ctrl Pts',(97.9534281470382,0.389817477279625,-5.87550603684422));
#22168=CARTESIAN_POINT('Ctrl Pts',(97.9401116843809,0.440817693439974,-5.87277646266194));
#22169=CARTESIAN_POINT('Ctrl Pts',(97.9241958691204,0.49107513427045,-5.87004688847967));
#22170=CARTESIAN_POINT('Ctrl Pts',(97.9057744059364,0.540347874063355,-5.86731731429739));
#22171=CARTESIAN_POINT('Ctrl Pts',(97.8857288623146,0.593964616936417,-5.86434709429949));
#22172=CARTESIAN_POINT('Ctrl Pts',(97.8626540129301,0.646575917569546,-5.8613768743016));
#22173=CARTESIAN_POINT('Ctrl Pts',(97.836671590467,0.697816824049706,-5.8584066543037));
#22174=CARTESIAN_POINT('Ctrl Pts',(97.8107350546114,0.748967235836129,-5.85544167990288));
#22175=CARTESIAN_POINT('Ctrl Pts',(97.7819013717319,0.798751596087378,-5.85247670550206));
#22176=CARTESIAN_POINT('Ctrl Pts',(97.7503406242082,0.846824078401311,-5.84951173110124));
#22177=CARTESIAN_POINT('Ctrl Pts',(97.718811019181,0.894849125301756,-5.84654968238222));
#22178=CARTESIAN_POINT('Ctrl Pts',(97.6845599658042,0.941165207505367,-5.8435876336632));
#22179=CARTESIAN_POINT('Ctrl Pts',(97.6478029747452,0.985451880383085,-5.84062558494418));
#22180=CARTESIAN_POINT('Ctrl Pts',(97.6110681040566,1.0297119015252,-5.83766531878714));
#22181=CARTESIAN_POINT('Ctrl Pts',(97.5718306174779,1.07194453405626,-5.8347050526301));
#22182=CARTESIAN_POINT('Ctrl Pts',(97.5303474586884,1.11186089628237,-5.83174478647306));
#22183=CARTESIAN_POINT('Ctrl Pts',(97.4888732965275,1.15176860167767,-5.82878516232149));
#22184=CARTESIAN_POINT('Ctrl Pts',(97.4451548046207,1.18936067291497,-5.82582553816993));
#22185=CARTESIAN_POINT('Ctrl Pts',(97.3994855097825,1.22438532983422,-5.82286591401837));
#22186=CARTESIAN_POINT('Ctrl Pts',(97.3537750116096,1.25944158638005,-5.8199036196617));
#22187=CARTESIAN_POINT('Ctrl Pts',(97.3061106076032,1.29192548128931,-5.81694132530502));
#22188=CARTESIAN_POINT('Ctrl Pts',(97.2568175320717,1.32162666717219,-5.81397903094835));
#22189=CARTESIAN_POINT('Ctrl Pts',(97.2075036354831,1.35134039863232,-5.81101548533885));
#22190=CARTESIAN_POINT('Ctrl Pts',(97.1565601572544,1.37826883282067,-5.80805193972935));
#22191=CARTESIAN_POINT('Ctrl Pts',(97.1043370116834,1.40224761411417,-5.80508839411985));
#22192=CARTESIAN_POINT('Ctrl Pts',(97.0520137049289,1.42627238542005,-5.80211916458932));
#22193=CARTESIAN_POINT('Ctrl Pts',(96.9984063130631,1.44733600738197,-5.79914993505879));
#22194=CARTESIAN_POINT('Ctrl Pts',(96.9438838946454,1.4653226923443,-5.79618070552826));
#22195=CARTESIAN_POINT('Ctrl Pts',(96.8952311143135,1.48137301178664,-5.79353112988036));
#22196=CARTESIAN_POINT('Ctrl Pts',(96.8458501985461,1.49497387408799,-5.79088155423246));
#22197=CARTESIAN_POINT('Ctrl Pts',(96.7960099265794,1.50607745670391,-5.78823197858457));
#22198=CARTESIAN_POINT('Ctrl Pts',(96.7401574615112,1.51852045582324,-5.78526278669454));
#22199=CARTESIAN_POINT('Ctrl Pts',(96.6834957764216,1.52787820917547,-5.78229359480452));
#22200=CARTESIAN_POINT('Ctrl Pts',(96.6263967605175,1.53405376166546,-5.7793244029145));
#22201=CARTESIAN_POINT('Ctrl Pts',(96.569378102475,1.54022062303907,-5.77635938969389));
#22202=CARTESIAN_POINT('Ctrl Pts',(96.5119238464598,1.54321410043556,-5.77339437647328));
#22203=CARTESIAN_POINT('Ctrl Pts',(96.4544166265746,1.54298808290489,-5.77042936325266));
#22204=CARTESIAN_POINT('Ctrl Pts',(96.3969681978041,1.54276229643778,-5.76746738124157));
#22205=CARTESIAN_POINT('Ctrl Pts',(96.3394674311735,1.53932354061843,-5.76450539923047));
#22206=CARTESIAN_POINT('Ctrl Pts',(96.2823004289469,1.53267762496487,-5.76154341721937));
#22207=CARTESIAN_POINT('Ctrl Pts',(96.2251698629896,1.52603594518802,-5.75858332307313));
#22208=CARTESIAN_POINT('Ctrl Pts',(96.1683731561569,1.51619122001913,-5.75562322892688));
#22209=CARTESIAN_POINT('Ctrl Pts',(96.1122925199385,1.50320118994959,-5.75266313478064));
#22210=CARTESIAN_POINT('Ctrl Pts',(96.0561991149433,1.49020820223183,-5.74970236666235));
#22211=CARTESIAN_POINT('Ctrl Pts',(96.0008226179281,1.47406858140213,-5.74674159854406));
#22212=CARTESIAN_POINT('Ctrl Pts',(95.946534597265,1.45489111171426,-5.74378083042577));
#22213=CARTESIAN_POINT('Ctrl Pts',(95.8922431486712,1.4357124310956,-5.74081987535449));
#22214=CARTESIAN_POINT('Ctrl Pts',(95.8390408011915,1.41349570508005,-5.73785892028321));
#22215=CARTESIAN_POINT('Ctrl Pts',(95.7872807856092,1.3883985520137,-5.73489796521193));
#22216=CARTESIAN_POINT('Ctrl Pts',(95.7354547427195,1.36326938393691,-5.73193323301871));
#22217=CARTESIAN_POINT('Ctrl Pts',(95.6850751706515,1.33525269038501,-5.72896850082549));
#22218=CARTESIAN_POINT('Ctrl Pts',(95.6364710924078,1.30455231987372,-5.72600376863226));
#22219=CARTESIAN_POINT('Ctrl Pts',(95.5965714697968,1.27935004793117,-5.72356998735451));
#22220=CARTESIAN_POINT('Ctrl Pts',(95.5578679692882,1.25234018643704,-5.72113620607676));
#22221=CARTESIAN_POINT('Ctrl Pts',(95.5205266553345,1.22365637526844,-5.71870242479901));
#22222=CARTESIAN_POINT('Ctrl Pts',(95.5205266553345,1.22365637526844,-6.21868058178697));
#22223=CARTESIAN_POINT('Ctrl Pts',(95.4747790085359,1.18851522132283,-6.2157136542204));
#22224=CARTESIAN_POINT('Ctrl Pts',(95.4310162232319,1.15081399765501,-6.21274672665382));
#22225=CARTESIAN_POINT('Ctrl Pts',(95.3895264706737,1.11081299241457,-6.20977979908725));
#22226=CARTESIAN_POINT('Ctrl Pts',(95.348019423428,1.07079531305955,-6.20681163477949));
#22227=CARTESIAN_POINT('Ctrl Pts',(95.3087876529973,1.02847632164036,-6.20384347047174));
#22228=CARTESIAN_POINT('Ctrl Pts',(95.2720813174728,0.984152078905769,-6.20087530616399));
#22229=CARTESIAN_POINT('Ctrl Pts',(95.2353040281644,0.93974215688186,-6.19790140435927));
#22230=CARTESIAN_POINT('Ctrl Pts',(95.201062239961,0.893319656152468,-6.19492750255455));
#22231=CARTESIAN_POINT('Ctrl Pts',(95.1695642023373,0.845211779198604,-6.19195360074983));
#22232=CARTESIAN_POINT('Ctrl Pts',(95.1402789442497,0.800483545348947,-6.18918861954945));
#22233=CARTESIAN_POINT('Ctrl Pts',(95.113365174356,0.754299010827867,-6.18642363834907));
#22234=CARTESIAN_POINT('Ctrl Pts',(95.0889538337176,0.70693873175991,-6.18365865714869));
#22235=CARTESIAN_POINT('Ctrl Pts',(95.0627503898425,0.656101605161792,-6.18069069112123));
#22236=CARTESIAN_POINT('Ctrl Pts',(95.0393219794477,0.6036983292004,-6.17772272509376));
#22237=CARTESIAN_POINT('Ctrl Pts',(95.0188572007958,0.550063602640737,-6.1747547590663));
#22238=CARTESIAN_POINT('Ctrl Pts',(94.9984289007308,0.496524480292817,-6.17179208345552));
#22239=CARTESIAN_POINT('Ctrl Pts',(94.9809539321004,0.441758747919574,-6.16882940784474));
#22240=CARTESIAN_POINT('Ctrl Pts',(94.9665742703897,0.386124117195004,-6.16586673223397));
#22241=CARTESIAN_POINT('Ctrl Pts',(94.9522089333496,0.330544908341546,-6.16290700796885));
#22242=CARTESIAN_POINT('Ctrl Pts',(94.9409329242954,0.274099019051727,-6.15994728370373));
#22243=CARTESIAN_POINT('Ctrl Pts',(94.9328389151162,0.217160803434828,-6.15698755943861));
#22244=CARTESIAN_POINT('Ctrl Pts',(94.9247498396805,0.160257294790163,-6.15402963928812));
#22245=CARTESIAN_POINT('Ctrl Pts',(94.9198389927644,0.102862570642138,-6.15107171913764));
#22246=CARTESIAN_POINT('Ctrl Pts',(94.9181478388104,0.0453605052125778,
-6.14811379898715));
#22247=CARTESIAN_POINT('Ctrl Pts',(94.916457061906,-0.0121287399019599,
-6.14515653831677));
#22248=CARTESIAN_POINT('Ctrl Pts',(94.9179845681433,-0.0697247570523037,
-6.14219927764639));
#22249=CARTESIAN_POINT('Ctrl Pts',(94.9227197642528,-0.127041477126066,
-6.13924201697601));
#22250=CARTESIAN_POINT('Ctrl Pts',(94.9274592224977,-0.184409787801061,
-6.13628209448451));
#22251=CARTESIAN_POINT('Ctrl Pts',(94.935412097954,-0.241497777290012,-6.133322171993));
#22252=CARTESIAN_POINT('Ctrl Pts',(94.946515804449,-0.297923713956436,-6.1303622495015));
#22253=CARTESIAN_POINT('Ctrl Pts',(94.9576241731273,-0.354373342536782,
-6.12740108420868));
#22254=CARTESIAN_POINT('Ctrl Pts',(94.9718858815279,-0.410159856896842,
-6.12443991891585));
#22255=CARTESIAN_POINT('Ctrl Pts',(94.9891876960229,-0.464914144811771,
-6.12147875362302));
#22256=CARTESIAN_POINT('Ctrl Pts',(95.0065228181682,-0.519773839976079,
-6.11851188780335));
#22257=CARTESIAN_POINT('Ctrl Pts',(95.0269095559865,-0.573596847731523,
-6.11554502198367));
#22258=CARTESIAN_POINT('Ctrl Pts',(95.050185840517,-0.626032511425179,-6.11257815616399));
#22259=CARTESIAN_POINT('Ctrl Pts',(95.0711195825055,-0.673191011026923,
-6.10990987792128));
#22260=CARTESIAN_POINT('Ctrl Pts',(95.0943897497026,-0.719227411779942,
-6.10724159967858));
#22261=CARTESIAN_POINT('Ctrl Pts',(95.1198477222013,-0.763905458585111,
-6.10457332143587));
#22262=CARTESIAN_POINT('Ctrl Pts',(95.1481877206498,-0.813641382261066,
-6.10160297486713));
#22263=CARTESIAN_POINT('Ctrl Pts',(95.1793581390997,-0.86190156408254,-6.0986326282984));
#22264=CARTESIAN_POINT('Ctrl Pts',(95.2131805995963,-0.908345108941542,
-6.09566228172966));
#22265=CARTESIAN_POINT('Ctrl Pts',(95.2469432703009,-0.95470655303541,-6.09269718600315));
#22266=CARTESIAN_POINT('Ctrl Pts',(95.2833483732805,-0.999257316401485,
-6.08973209027663));
#22267=CARTESIAN_POINT('Ctrl Pts',(95.3221728492778,-1.04168309422453,-6.08676699455011));
#22268=CARTESIAN_POINT('Ctrl Pts',(95.360958973831,-1.08406696317938,-6.08380482779301));
#22269=CARTESIAN_POINT('Ctrl Pts',(95.4021593860605,-1.12432962298756,-6.08084266103592));
#22270=CARTESIAN_POINT('Ctrl Pts',(95.445510226097,-1.16218906830109,-6.07788049427882));
#22271=CARTESIAN_POINT('Ctrl Pts',(95.4888349273732,-1.20002568593778,-6.07492011358554));
#22272=CARTESIAN_POINT('Ctrl Pts',(95.5343070942845,-1.23546161940882,-6.07195973289227));
#22273=CARTESIAN_POINT('Ctrl Pts',(95.5816269954335,-1.26825262754952,-6.06899935219899));
#22274=CARTESIAN_POINT('Ctrl Pts',(95.6289365750507,-1.30103648323592,-6.06603961723114));
#22275=CARTESIAN_POINT('Ctrl Pts',(95.6780926604554,-1.33117626234097,-6.06307988226328));
#22276=CARTESIAN_POINT('Ctrl Pts',(95.7287653189123,-1.35847018216852,-6.06012014729543));
#22277=CARTESIAN_POINT('Ctrl Pts',(95.7794835769142,-1.38578866337424,-6.05715774890766));
#22278=CARTESIAN_POINT('Ctrl Pts',(95.8317206755153,-1.41025591932714,-6.05419535051988));
#22279=CARTESIAN_POINT('Ctrl Pts',(95.8851219847079,-1.43171612463671,-6.0512329521321));
#22280=CARTESIAN_POINT('Ctrl Pts',(95.9385457853317,-1.45318536850242,-6.04826930604871));
#22281=CARTESIAN_POINT('Ctrl Pts',(95.9931342796287,-1.47164486852846,-6.04530565996532));
#22282=CARTESIAN_POINT('Ctrl Pts',(96.0485158027972,-1.48698813641492,-6.04234201388192));
#22283=CARTESIAN_POINT('Ctrl Pts',(96.1040034037539,-1.50236079280185,-6.03937269122982));
#22284=CARTESIAN_POINT('Ctrl Pts',(96.1602865579545,-1.51460517806133,-6.03640336857772));
#22285=CARTESIAN_POINT('Ctrl Pts',(96.2169824419505,-1.52366580219669,-6.03343404592562));
#22286=CARTESIAN_POINT('Ctrl Pts',(96.2675561428979,-1.53174803432927,-6.03078535919143));
#22287=CARTESIAN_POINT('Ctrl Pts',(96.3184578788774,-1.5372976770742,-6.02813667245723));
#22288=CARTESIAN_POINT('Ctrl Pts',(96.369414962073,-1.54031035376639,-6.02548798572304));
#22289=CARTESIAN_POINT('Ctrl Pts',(96.4265650355648,-1.54368917146097,-6.02251739494305));
#22290=CARTESIAN_POINT('Ctrl Pts',(96.4840219219422,-1.54389003411547,-6.01954680416306));
#22291=CARTESIAN_POINT('Ctrl Pts',(96.5414025287611,-1.5408766005175,-6.01657621338308));
#22292=CARTESIAN_POINT('Ctrl Pts',(96.5986820643019,-1.53786847483804,-6.01361085505745));
#22293=CARTESIAN_POINT('Ctrl Pts',(96.6558850707543,-1.53165731786393,-6.01064549673183));
#22294=CARTESIAN_POINT('Ctrl Pts',(96.712626384826,-1.52225874262003,-6.00768013840621));
#22295=CARTESIAN_POINT('Ctrl Pts',(96.7693118646023,-1.51286941571369,-6.0047176980372));
#22296=CARTESIAN_POINT('Ctrl Pts',(96.8255360405538,-1.50029896973757,-6.00175525766819));
#22297=CARTESIAN_POINT('Ctrl Pts',(96.8809185815599,-1.48461483139992,-5.99879281729918));
#22298=CARTESIAN_POINT('Ctrl Pts',(96.9362679290057,-1.46894009336032,-5.99583215247064));
#22299=CARTESIAN_POINT('Ctrl Pts',(96.9907761410612,-1.45015550416919,-5.9928714876421));
#22300=CARTESIAN_POINT('Ctrl Pts',(97.0440749858331,-1.42837915164229,-5.98991082281356));
#22301=CARTESIAN_POINT('Ctrl Pts',(97.0973623869221,-1.40660747467026,-5.98695079366315));
#22302=CARTESIAN_POINT('Ctrl Pts',(97.149440454119,-1.3818455068257,-5.98399076451273));
#22303=CARTESIAN_POINT('Ctrl Pts',(97.1999600800918,-1.35425980355805,-5.98103073536232));
#22304=CARTESIAN_POINT('Ctrl Pts',(97.2505253930866,-1.32664915337898,-5.97806802933307));
#22305=CARTESIAN_POINT('Ctrl Pts',(97.299528989743,-1.29620991462818,-5.97510532330383));
#22306=CARTESIAN_POINT('Ctrl Pts',(97.3466468187319,-1.26315440558351,-5.97214261727459));
#22307=CARTESIAN_POINT('Ctrl Pts',(97.3937846159362,-1.23008488783888,-5.96917865567068));
#22308=CARTESIAN_POINT('Ctrl Pts',(97.4390346416185,-1.19439721201901,-5.96621469406677));
#22309=CARTESIAN_POINT('Ctrl Pts',(97.4821049123582,-1.15634487877593,-5.96325073246286));
#22310=CARTESIAN_POINT('Ctrl Pts',(97.5252578058132,-1.11821954884524,-5.96028108502155));
#22311=CARTESIAN_POINT('Ctrl Pts',(97.5662222164714,-1.0777208642979,-5.95731143758024));
#22312=CARTESIAN_POINT('Ctrl Pts',(97.6047428238428,-1.0351394896833,-5.95434179013894));
#22313=CARTESIAN_POINT('Ctrl Pts',(97.6390701871419,-0.99719340274645,-5.95169541009603));
#22314=CARTESIAN_POINT('Ctrl Pts',(97.6714572375037,-0.957594078838122,
-5.94904903005312));
#22315=CARTESIAN_POINT('Ctrl Pts',(97.7017520058931,-0.916567054149245,
-5.94640265001022));
#22316=CARTESIAN_POINT('Ctrl Pts',(97.7359095435129,-0.870308831566921,
-5.94341884024116));
#22317=CARTESIAN_POINT('Ctrl Pts',(97.7675493401887,-0.822041711790214,
-5.94043503047209));
#22318=CARTESIAN_POINT('Ctrl Pts',(97.7964295587994,-0.77206885283428,-5.93745122070303));
#22319=CARTESIAN_POINT('Ctrl Pts',(97.8252637154166,-0.722175697205116,
-5.93447216990854));
#22320=CARTESIAN_POINT('Ctrl Pts',(97.8513467650861,-0.670582637972176,
-5.93149311911405));
#22321=CARTESIAN_POINT('Ctrl Pts',(97.8744789895756,-0.61762330176256,-5.92851406831956));
#22322=CARTESIAN_POINT('Ctrl Pts',(97.8975810174734,-0.564733098180144,
-5.9255389063504));
#22323=CARTESIAN_POINT('Ctrl Pts',(97.9177396604431,-0.510480626667888,
-5.92256374438124));
#22324=CARTESIAN_POINT('Ctrl Pts',(97.9348012475247,-0.455223746150777,
-5.91958858241208));
#22325=CARTESIAN_POINT('Ctrl Pts',(97.9518495970124,-0.400009737855236,
-5.91661572878537));
#22326=CARTESIAN_POINT('Ctrl Pts',(97.9658055059916,-0.343793356931493,
-5.91364287515866));
#22327=CARTESIAN_POINT('Ctrl Pts',(97.9765642485778,-0.286950223019388,
-5.91067002153195));
#22328=CARTESIAN_POINT('Ctrl Pts',(97.9873211159564,-0.230116996647804,
-5.90769768606224));
#22329=CARTESIAN_POINT('Ctrl Pts',(97.9948818164853,-0.172657737517019,
-5.90472535059254));
#22330=CARTESIAN_POINT('Ctrl Pts',(97.9991925548639,-0.114959104708224,
-5.90175301512283));
#22331=CARTESIAN_POINT('Ctrl Pts',(98.0020760817902,-0.076363498410695,
-5.89976476888564));
#22332=CARTESIAN_POINT('Ctrl Pts',(98.0035064719747,-0.037661007893966,
-5.89777652264845));
#22333=CARTESIAN_POINT('Ctrl Pts',(98.0034806047668,0.00103154458141929,
-5.89578827641126));
#22334=CARTESIAN_POINT('Ctrl Pts',(95.5043589656634,0.823943515129422,-6.49867147181494));
#22335=CARTESIAN_POINT('Ctrl Pts',(95.2313273711832,0.507125615617518,-6.47230253119553));
#22336=CARTESIAN_POINT('Ctrl Pts',(95.0301651886135,-0.41430205054822,-6.41957181200518));
#22337=CARTESIAN_POINT('Ctrl Pts',(96.0282541226869,-1.42674737697425,-6.34047931424389));
#22338=CARTESIAN_POINT('Ctrl Pts',(97.4200723870437,-1.13963437637263,-6.26139397853106));
#22339=CARTESIAN_POINT('Ctrl Pts',(97.9392541762185,0.182147029996038,-6.18230864281824));
#22340=CARTESIAN_POINT('Ctrl Pts',(97.1144000113395,1.33894478249095,-6.10322330710542));
#22341=CARTESIAN_POINT('Ctrl Pts',(95.6950438149812,1.27835036330238,-6.02413797139259));
#22342=CARTESIAN_POINT('Ctrl Pts',(94.9715162077941,0.0558575875799088,
-5.94505263567977));
#22343=CARTESIAN_POINT('Ctrl Pts',(95.6014510801772,-1.21747314835048,-5.86596729996694));
#22344=CARTESIAN_POINT('Ctrl Pts',(97.0122595444212,-1.38408065930718,-5.78688196425412));
#22345=CARTESIAN_POINT('Ctrl Pts',(97.9214937080554,-0.292562534091784,
-5.70779662854129));
#22346=CARTESIAN_POINT('Ctrl Pts',(97.5026547470092,1.064906048784,-5.62871129282847));
#22347=CARTESIAN_POINT('Ctrl Pts',(96.1364757169747,1.45435879288526,-5.54962595711564));
#22348=CARTESIAN_POINT('Ctrl Pts',(95.064809124152,0.521798178599738,-5.47054062140283));
#22349=CARTESIAN_POINT('Ctrl Pts',(95.2618435898322,-0.885101436100427,
-5.39145528569));
#22350=CARTESIAN_POINT('Ctrl Pts',(96.548398339734,-1.48739510247996,-5.31236994997717));
#22351=CARTESIAN_POINT('Ctrl Pts',(97.7551431885111,-0.737721463002487,
-5.23328461426435));
#22352=CARTESIAN_POINT('Ctrl Pts',(97.7848018665854,0.682731210024832,-5.15419927855152));
#22353=CARTESIAN_POINT('Ctrl Pts',(96.6111236810192,1.48219061059408,-5.0751139428387));
#22354=CARTESIAN_POINT('Ctrl Pts',(95.2994978278247,0.93517180164541,-4.99602860712587));
#22355=CARTESIAN_POINT('Ctrl Pts',(95.0454088976356,-0.463506086877637,
-4.91694327141305));
#22356=CARTESIAN_POINT('Ctrl Pts',(95.7305669616929,-1.1113509684898,-4.86421971427117));
#22357=CARTESIAN_POINT('Ctrl Pts',(96.1344998019829,-1.21933935595969,-4.83785793570023));
#22358=CARTESIAN_POINT('Ctrl Pts',(95.4329527647036,0.885478211758894,-6.55309378487631));
#22359=CARTESIAN_POINT('Ctrl Pts',(95.1395303108646,0.544999353728263,-6.5267248442569));
#22360=CARTESIAN_POINT('Ctrl Pts',(94.9233447029623,-0.445243432481966,
-6.47399412506655));
#22361=CARTESIAN_POINT('Ctrl Pts',(95.9959740620038,-1.53330136447085,-6.39490162730526));
#22362=CARTESIAN_POINT('Ctrl Pts',(97.4917376977215,-1.22474586075344,-6.31581629159243));
#22363=CARTESIAN_POINT('Ctrl Pts',(98.049693618018,0.195750343848208,-6.23673095587962));
#22364=CARTESIAN_POINT('Ctrl Pts',(97.1632367463181,1.43894139570691,-6.15764562016679));
#22365=CARTESIAN_POINT('Ctrl Pts',(95.6378785591096,1.37382159445786,-6.07856028445398));
#22366=CARTESIAN_POINT('Ctrl Pts',(94.8603156315467,0.060029208137714,-5.99947494874113));
#22367=CARTESIAN_POINT('Ctrl Pts',(95.5372960241103,-1.30839787736726,-5.92038961302833));
#22368=CARTESIAN_POINT('Ctrl Pts',(97.0534681076501,-1.48744816195426,-5.84130427731549));
#22369=CARTESIAN_POINT('Ctrl Pts',(98.0306067421578,-0.314412025531326,
-5.76221894160267));
#22370=CARTESIAN_POINT('Ctrl Pts',(97.5804875684133,1.14443658631183,-5.68313360588984));
#22371=CARTESIAN_POINT('Ctrl Pts',(96.1122779857853,1.56297488788122,-5.60404827017702));
#22372=CARTESIAN_POINT('Ctrl Pts',(94.9605759567141,0.56076770992362,-5.52496293446419));
#22373=CARTESIAN_POINT('Ctrl Pts',(95.1723255768299,-0.951203598878167,
-5.44587759875138));
#22374=CARTESIAN_POINT('Ctrl Pts',(96.5549642873171,-1.59847845312067,-5.36679226303854));
#22375=CARTESIAN_POINT('Ctrl Pts',(97.8518326419112,-0.792816825232235,
-5.28770692732572));
#22376=CARTESIAN_POINT('Ctrl Pts',(97.8837063234708,0.733719726976447,-5.20862159161289));
#22377=CARTESIAN_POINT('Ctrl Pts',(96.622374154636,1.59288527338979,-5.12953625590007));
#22378=CARTESIAN_POINT('Ctrl Pts',(95.2127919519034,1.00501337701317,-5.05045092018725));
#22379=CARTESIAN_POINT('Ctrl Pts',(94.9397268601826,-0.498122181207173,
-4.97136558447442));
#22380=CARTESIAN_POINT('Ctrl Pts',(95.6760546862938,-1.19435015889442,-4.91864202733255));
#22381=CARTESIAN_POINT('Ctrl Pts',(96.1101545032388,-1.31040345923813,-4.89228024876161));
#22382=CARTESIAN_POINT('Ctrl Pts',(95.3615465637438,0.947012908388365,-6.60751609793768));
#22383=CARTESIAN_POINT('Ctrl Pts',(95.0477332505459,0.582873091839006,-6.58114715731827));
#22384=CARTESIAN_POINT('Ctrl Pts',(94.8165242173111,-0.476184814415712,
-6.52841643812792));
#22385=CARTESIAN_POINT('Ctrl Pts',(95.9636940013207,-1.63985535196744,-6.44932394036664));
#22386=CARTESIAN_POINT('Ctrl Pts',(97.5634030083993,-1.30985734513425,-6.37023860465382));
#22387=CARTESIAN_POINT('Ctrl Pts',(98.1601330598174,0.209353657700377,-6.29115326894099));
#22388=CARTESIAN_POINT('Ctrl Pts',(97.2120734812969,1.53893800892286,-6.21206793322817));
#22389=CARTESIAN_POINT('Ctrl Pts',(95.5807133032378,1.46929282561336,-6.13298259751535));
#22390=CARTESIAN_POINT('Ctrl Pts',(94.7491150552996,0.0642008286955192,
-6.05389726180251));
#22391=CARTESIAN_POINT('Ctrl Pts',(95.4731409680433,-1.39932260638405,-5.9748119260897));
#22392=CARTESIAN_POINT('Ctrl Pts',(97.0946766708791,-1.59081566460134,-5.89572659037687));
#22393=CARTESIAN_POINT('Ctrl Pts',(98.1397197762602,-0.33626151697087,-5.81664125466405));
#22394=CARTESIAN_POINT('Ctrl Pts',(97.6583203898173,1.22396712383966,-5.73755591895122));
#22395=CARTESIAN_POINT('Ctrl Pts',(96.0880802545957,1.67159098287717,-5.6584705832384));
#22396=CARTESIAN_POINT('Ctrl Pts',(94.8563427892762,0.599737241247502,-5.57938524752557));
#22397=CARTESIAN_POINT('Ctrl Pts',(95.0828075638274,-1.01730576165591,-5.50029991181274));
#22398=CARTESIAN_POINT('Ctrl Pts',(96.5615302349002,-1.7095618037614,-5.42121457609992));
#22399=CARTESIAN_POINT('Ctrl Pts',(97.9485220953112,-0.847912187461983,
-5.3421292403871));
#22400=CARTESIAN_POINT('Ctrl Pts',(97.9826107803565,0.784708243928062,-5.26304390467428));
#22401=CARTESIAN_POINT('Ctrl Pts',(96.6336246282528,1.70357993618549,-5.18395856896145));
#22402=CARTESIAN_POINT('Ctrl Pts',(95.1260860759822,1.07485495238092,-5.10487323324863));
#22403=CARTESIAN_POINT('Ctrl Pts',(94.8340448227295,-0.532738275536707,
-5.0257878975358));
#22404=CARTESIAN_POINT('Ctrl Pts',(95.6215424108947,-1.27734934929906,-4.97306434039392));
#22405=CARTESIAN_POINT('Ctrl Pts',(96.0858092044945,-1.40146756251658,-4.94670256182298));
#22406=CARTESIAN_POINT('Ctrl Pts',(95.290140362784,1.00854760501783,-6.66193841099905));
#22407=CARTESIAN_POINT('Ctrl Pts',(94.9559361902272,0.620746829949751,-6.63556947037964));
#22408=CARTESIAN_POINT('Ctrl Pts',(94.70970373166,-0.507126196349458,-6.58283875118929));
#22409=CARTESIAN_POINT('Ctrl Pts',(95.9314139406376,-1.74640933946404,-6.50374625342801));
#22410=CARTESIAN_POINT('Ctrl Pts',(97.6350683190773,-1.39496882951506,-6.42466091771519));
#22411=CARTESIAN_POINT('Ctrl Pts',(98.2705725016169,0.222956971552548,-6.34557558200236));
#22412=CARTESIAN_POINT('Ctrl Pts',(97.2609102162756,1.63893462213883,-6.26649024628954));
#22413=CARTESIAN_POINT('Ctrl Pts',(95.523548047366,1.56476405676884,-6.18740491057671));
#22414=CARTESIAN_POINT('Ctrl Pts',(94.6379144790523,0.0683724492533236,
-6.10831957486389));
#22415=CARTESIAN_POINT('Ctrl Pts',(95.4089859119762,-1.49024733540083,-6.02923423915106));
#22416=CARTESIAN_POINT('Ctrl Pts',(97.1358852341083,-1.69418316724842,-5.95014890343824));
#22417=CARTESIAN_POINT('Ctrl Pts',(98.2488328103626,-0.358111008410412,
-5.87106356772542));
#22418=CARTESIAN_POINT('Ctrl Pts',(97.7361532112215,1.30349766136748,-5.79197823201259));
#22419=CARTESIAN_POINT('Ctrl Pts',(96.0638825234059,1.78020707787313,-5.71289289629977));
#22420=CARTESIAN_POINT('Ctrl Pts',(94.7521096218384,0.638706772571385,-5.63380756058694));
#22421=CARTESIAN_POINT('Ctrl Pts',(94.993289550825,-1.08340792443364,-5.55472222487413));
#22422=CARTESIAN_POINT('Ctrl Pts',(96.5680961824832,-1.82064515440211,-5.47563688916129));
#22423=CARTESIAN_POINT('Ctrl Pts',(98.0452115487115,-0.903007549691732,
-5.39655155344847));
#22424=CARTESIAN_POINT('Ctrl Pts',(98.0815152372419,0.835696760879677,-5.31746621773565));
#22425=CARTESIAN_POINT('Ctrl Pts',(96.6448751018697,1.81427459898119,-5.23838088202282));
#22426=CARTESIAN_POINT('Ctrl Pts',(95.0393802000608,1.14469652774868,-5.15929554631));
#22427=CARTESIAN_POINT('Ctrl Pts',(94.7283627852766,-0.567354369866243,
-5.08021021059717));
#22428=CARTESIAN_POINT('Ctrl Pts',(95.5670301354957,-1.36034853970369,-5.02748665345529));
#22429=CARTESIAN_POINT('Ctrl Pts',(96.0614639057505,-1.49253166579503,-5.00112487488435));
#22430=CARTESIAN_POINT('',(95.5014043034582,0.825823195401267,-4.99934226694474));
#22431=CARTESIAN_POINT('Ctrl Pts',(96.0619671077198,-1.49064942821852,-4.99999999999999));
#22432=CARTESIAN_POINT('Ctrl Pts',(96.0044903608498,-1.46964766148004,-5.));
#22433=CARTESIAN_POINT('Ctrl Pts',(95.9485815372201,-1.44501993476363,-4.99999999999999));
#22434=CARTESIAN_POINT('Ctrl Pts',(95.8944377879902,-1.41706920437079,-4.99999999999999));
#22435=CARTESIAN_POINT('Ctrl Pts',(95.8402940387602,-1.38911847397796,-4.99999999999999));
#22436=CARTESIAN_POINT('Ctrl Pts',(95.7879146300858,-1.35784372527998,-4.99999999999998));
#22437=CARTESIAN_POINT('Ctrl Pts',(95.7375294374415,-1.32350210039842,-4.99999999999999));
#22438=CARTESIAN_POINT('Ctrl Pts',(95.6994193338114,-1.29752695146327,-4.99999999999999));
#22439=CARTESIAN_POINT('Ctrl Pts',(95.6624507216058,-1.26979620197149,-5.));
#22440=CARTESIAN_POINT('Ctrl Pts',(95.626739354002,-1.2404089680386,-4.99999999999999));
#22441=CARTESIAN_POINT('Ctrl Pts',(95.6076811882898,-1.22472581693859,-4.99999999999998));
#22442=CARTESIAN_POINT('Ctrl Pts',(95.5889813520719,-1.20857073916018,-4.99999999999998));
#22443=CARTESIAN_POINT('Ctrl Pts',(95.5706593721573,-1.19195798019386,-4.99999999999998));
#22444=CARTESIAN_POINT('Ctrl Pts',(95.5629407688328,-1.18495942997258,-4.99999999999998));
#22445=CARTESIAN_POINT('Ctrl Pts',(95.5552893940888,-1.17787965716329,-4.99999999999997));
#22446=CARTESIAN_POINT('Ctrl Pts',(95.5477168724182,-1.17072963197948,-4.99999999999997));
#22447=CARTESIAN_POINT('Ctrl Pts',(95.504650124993,-1.13006572343368,-4.99999999999999));
#22448=CARTESIAN_POINT('Ctrl Pts',(95.4640439159528,-1.0870546361245,-5.));
#22449=CARTESIAN_POINT('Ctrl Pts',(95.4261046731238,-1.0419386282516,-4.99999999999999));
#22450=CARTESIAN_POINT('Ctrl Pts',(95.3889373943342,-0.997740612755019,
-4.99999999999998));
#22451=CARTESIAN_POINT('Ctrl Pts',(95.3543292114615,-0.951521519435711,
-4.99999999999996));
#22452=CARTESIAN_POINT('Ctrl Pts',(95.3225171923515,-0.903486061979851,
-4.99999999999998));
#22453=CARTESIAN_POINT('Ctrl Pts',(95.2912703645555,-0.856304031124319,
-5.));
#22454=CARTESIAN_POINT('Ctrl Pts',(95.2627208389812,-0.807368811665195,
-5.));
#22455=CARTESIAN_POINT('Ctrl Pts',(95.2371412618981,-0.756864590129229,
-4.99999999999998));
#22456=CARTESIAN_POINT('Ctrl Pts',(95.2336088440832,-0.749890197577584,
-4.99999999999998));
#22457=CARTESIAN_POINT('Ctrl Pts',(95.2301331454239,-0.742885878855996,
-4.99999999999998));
#22458=CARTESIAN_POINT('Ctrl Pts',(95.2267149639007,-0.73585211685431,-4.99999999999998));
#22459=CARTESIAN_POINT('Ctrl Pts',(95.2218245699291,-0.725788910129543,
-4.99999999999997));
#22460=CARTESIAN_POINT('Ctrl Pts',(95.2170556886264,-0.715673106931688,
-4.99999999999998));
#22461=CARTESIAN_POINT('Ctrl Pts',(95.2124126352842,-0.705512126926518,
-4.99999999999998));
#22462=CARTESIAN_POINT('Ctrl Pts',(95.1892489299728,-0.654820065223355,
-4.99999999999999));
#22463=CARTESIAN_POINT('Ctrl Pts',(95.1691908098272,-0.602958917485143,
-5.));
#22464=CARTESIAN_POINT('Ctrl Pts',(95.1524510672623,-0.550120264291242,
-4.99999999999999));
#22465=CARTESIAN_POINT('Ctrl Pts',(95.1406599895568,-0.512901969968789,
-4.99999999999997));
#22466=CARTESIAN_POINT('Ctrl Pts',(95.1305162434914,-0.475198299946772,
-4.99999999999999));
#22467=CARTESIAN_POINT('Ctrl Pts',(95.1221096646921,-0.437074027164263,
-4.99999999999999));
#22468=CARTESIAN_POINT('Ctrl Pts',(95.1102087873009,-0.383102928237414,
-5.));
#22469=CARTESIAN_POINT('Ctrl Pts',(95.1017878832149,-0.328287883604904,
-5.00000000000001));
#22470=CARTESIAN_POINT('Ctrl Pts',(95.0967901027504,-0.272945005188943,
-5.));
#22471=CARTESIAN_POINT('Ctrl Pts',(95.0953641741231,-0.257154996962496,
-4.99999999999999));
#22472=CARTESIAN_POINT('Ctrl Pts',(95.0942171752866,-0.241322108062098,
-4.99999999999998));
#22473=CARTESIAN_POINT('Ctrl Pts',(95.0933484296855,-0.225453941639844,
-4.99999999999998));
#22474=CARTESIAN_POINT('Ctrl Pts',(95.0926773352721,-0.213195994293428,
-4.99999999999998));
#22475=CARTESIAN_POINT('Ctrl Pts',(95.0921723561223,-0.200914299570177,
-5.00000000000001));
#22476=CARTESIAN_POINT('Ctrl Pts',(95.0918335220152,-0.188636107436641,
-5.00000000000001));
#22477=CARTESIAN_POINT('Ctrl Pts',(95.0902952695563,-0.132895085968137,
-5.00000000000001));
#22478=CARTESIAN_POINT('Ctrl Pts',(95.0921697597597,-0.0771242598153453,
-4.99999999999998));
#22479=CARTESIAN_POINT('Ctrl Pts',(95.0973480466347,-0.0216419304349217,
-5.));
#22480=CARTESIAN_POINT('Ctrl Pts',(95.1025032536317,0.0335931114889033,
-5.00000000000002));
#22481=CARTESIAN_POINT('Ctrl Pts',(95.1109333654676,0.0885433493664647,
-4.99999999999998));
#22482=CARTESIAN_POINT('Ctrl Pts',(95.1225798921731,0.1428795104336,-4.99999999999999));
#22483=CARTESIAN_POINT('Ctrl Pts',(95.1297471360315,0.176317850167353,-4.99999999999999));
#22484=CARTESIAN_POINT('Ctrl Pts',(95.1381334114814,0.209523261961388,-5.));
#22485=CARTESIAN_POINT('Ctrl Pts',(95.1477331817925,0.242413357936291,-4.99999999999999));
#22486=CARTESIAN_POINT('Ctrl Pts',(95.1527180305541,0.259492115956323,-4.99999999999998));
#22487=CARTESIAN_POINT('Ctrl Pts',(95.1580301804523,0.27648576852378,-5.));
#22488=CARTESIAN_POINT('Ctrl Pts',(95.1636694489763,0.293382161393636,-4.99999999999999));
#22489=CARTESIAN_POINT('Ctrl Pts',(95.1678840387523,0.306009927625527,-4.99999999999999));
#22490=CARTESIAN_POINT('Ctrl Pts',(95.1722821897657,0.318585210618562,-5.));
#22491=CARTESIAN_POINT('Ctrl Pts',(95.1768559904802,0.331082302853865,-5.));
#22492=CARTESIAN_POINT('Ctrl Pts',(95.1953000280353,0.381477335979576,-5.));
#22493=CARTESIAN_POINT('Ctrl Pts',(95.2166211329857,0.430678493749573,-5.00000000000001));
#22494=CARTESIAN_POINT('Ctrl Pts',(95.240774279695,0.478371965785178,-5.00000000000001));
#22495=CARTESIAN_POINT('Ctrl Pts',(95.2570276377204,0.510466296424444,-5.00000000000001));
#22496=CARTESIAN_POINT('Ctrl Pts',(95.2745642988511,0.541877366233536,-5.00000000000001));
#22497=CARTESIAN_POINT('Ctrl Pts',(95.2933797850577,0.572499863819867,-5.));
#22498=CARTESIAN_POINT('Ctrl Pts',(95.3018662740307,0.586311757131528,-5.));
#22499=CARTESIAN_POINT('Ctrl Pts',(95.3106153830304,0.599966301852985,-4.99999999999998));
#22500=CARTESIAN_POINT('Ctrl Pts',(95.3196115901348,0.613430963692222,-4.99999999999998));
#22501=CARTESIAN_POINT('Ctrl Pts',(95.348069797335,0.656024484723174,-4.99999999999998));
#22502=CARTESIAN_POINT('Ctrl Pts',(95.3790237180575,0.696765113806646,-5.00000000000001));
#22503=CARTESIAN_POINT('Ctrl Pts',(95.4124490992335,0.73535259756695,-5.));
#22504=CARTESIAN_POINT('Ctrl Pts',(95.4310001045575,0.756768557280509,-4.99999999999999));
#22505=CARTESIAN_POINT('Ctrl Pts',(95.4503129437851,0.777520633676359,-5.00000000000001));
#22506=CARTESIAN_POINT('Ctrl Pts',(95.4703873188195,0.797551637847658,-5.));
#22507=CARTESIAN_POINT('Ctrl Pts',(95.48024357984,0.80738660432981,-5.));
#22508=CARTESIAN_POINT('Ctrl Pts',(95.49028346793,0.817047668215136,-5.));
#22509=CARTESIAN_POINT('Ctrl Pts',(95.5005012383867,0.826532410909935,-4.99999999999998));
#22510=CARTESIAN_POINT('Ctrl Pts',(95.5023647968546,0.825211298936477,-6.49999999999999));
#22511=CARTESIAN_POINT('Ctrl Pts',(95.465287791204,0.790586303190538,-6.49999999999999));
#22512=CARTESIAN_POINT('Ctrl Pts',(95.4306205888711,0.753694223654168,-6.49999999999999));
#22513=CARTESIAN_POINT('Ctrl Pts',(95.3983634067294,0.714861091992313,-6.49999999999999));
#22514=CARTESIAN_POINT('Ctrl Pts',(95.3648728756,0.674543180804199,-6.49999999999998));
#22515=CARTESIAN_POINT('Ctrl Pts',(95.3339795912397,0.632132434877562,-6.49999999999999));
#22516=CARTESIAN_POINT('Ctrl Pts',(95.3057119559182,0.587944010484693,-6.49999999999999));
#22517=CARTESIAN_POINT('Ctrl Pts',(95.2829274891997,0.552326963870395,-6.5));
#22518=CARTESIAN_POINT('Ctrl Pts',(95.2618492968538,0.515553843547565,-6.5));
#22519=CARTESIAN_POINT('Ctrl Pts',(95.2425087645259,0.477771511851716,-6.49999999999999));
#22520=CARTESIAN_POINT('Ctrl Pts',(95.2337277979766,0.460617620472229,-6.49999999999999));
#22521=CARTESIAN_POINT('Ctrl Pts',(95.2253052381579,0.443255508206861,-6.5));
#22522=CARTESIAN_POINT('Ctrl Pts',(95.2172451705105,0.42569809959244,-6.49999999999999));
#22523=CARTESIAN_POINT('Ctrl Pts',(95.2135756822996,0.417704779096444,-6.49999999999998));
#22524=CARTESIAN_POINT('Ctrl Pts',(95.209982368788,0.409673082119565,-6.49999999999999));
#22525=CARTESIAN_POINT('Ctrl Pts',(95.2064689645341,0.401612534201166,-6.49999999999999));
#22526=CARTESIAN_POINT('Ctrl Pts',(95.184714004968,0.351701712282167,-6.5));
#22527=CARTESIAN_POINT('Ctrl Pts',(95.165979192754,0.300599814091978,-6.49999999999997));
#22528=CARTESIAN_POINT('Ctrl Pts',(95.1502902359844,0.248639171268916,-6.49999999999998));
#22529=CARTESIAN_POINT('Ctrl Pts',(95.1342974905974,0.195672403432671,-6.49999999999999));
#22530=CARTESIAN_POINT('Ctrl Pts',(95.1214690981579,0.141812387425034,-6.50000000000001));
#22531=CARTESIAN_POINT('Ctrl Pts',(95.1118732260187,0.0873765018499251,
-6.5));
#22532=CARTESIAN_POINT('Ctrl Pts',(95.1048940041838,0.0477844652225939,
-6.5));
#22533=CARTESIAN_POINT('Ctrl Pts',(95.0996255705039,0.00788700886965863,
-6.50000000000001));
#22534=CARTESIAN_POINT('Ctrl Pts',(95.0961101241668,-0.0322004775501682,
-6.50000000000001));
#22535=CARTESIAN_POINT('Ctrl Pts',(95.0946964759413,-0.048320650809826,
-6.50000000000001));
#22536=CARTESIAN_POINT('Ctrl Pts',(95.0935664559224,-0.0644715938332609,
-6.5));
#22537=CARTESIAN_POINT('Ctrl Pts',(95.0927234879583,-0.0806459176364314,
-6.5));
#22538=CARTESIAN_POINT('Ctrl Pts',(95.0921920134768,-0.0908435060643399,
-6.5));
#22539=CARTESIAN_POINT('Ctrl Pts',(95.0917751094851,-0.101042304681634,
-6.50000000000001));
#22540=CARTESIAN_POINT('Ctrl Pts',(95.09147320548,-0.111235651179997,-6.50000000000001));
#22541=CARTESIAN_POINT('Ctrl Pts',(95.0897905333277,-0.168048611595366,
-6.49999999999999));
#22542=CARTESIAN_POINT('Ctrl Pts',(95.0916740645112,-0.22473643786415,-6.50000000000001));
#22543=CARTESIAN_POINT('Ctrl Pts',(95.0971821488728,-0.280965948211095,
-6.50000000000001));
#22544=CARTESIAN_POINT('Ctrl Pts',(95.1008218950827,-0.318122450133394,
-6.5));
#22545=CARTESIAN_POINT('Ctrl Pts',(95.1060452317314,-0.355079435484354,
-6.49999999999997));
#22546=CARTESIAN_POINT('Ctrl Pts',(95.1128809155332,-0.391744565936287,
-6.49999999999998));
#22547=CARTESIAN_POINT('Ctrl Pts',(95.1229622858471,-0.445818857318795,
-6.49999999999999));
#22548=CARTESIAN_POINT('Ctrl Pts',(95.1365480764267,-0.499258916074601,
-6.5));
#22549=CARTESIAN_POINT('Ctrl Pts',(95.15341201345,-0.551862544225393,-6.5));
#22550=CARTESIAN_POINT('Ctrl Pts',(95.1580484215608,-0.566324878132217,
-6.49999999999999));
#22551=CARTESIAN_POINT('Ctrl Pts',(95.1629329153471,-0.580723955294647,
-6.49999999999999));
#22552=CARTESIAN_POINT('Ctrl Pts',(95.1680614573946,-0.595055460668329,
-6.49999999999999));
#22553=CARTESIAN_POINT('Ctrl Pts',(95.172427499774,-0.607256191254597,-6.49999999999998));
#22554=CARTESIAN_POINT('Ctrl Pts',(95.1769718397079,-0.619411186056283,
-6.49999999999999));
#22555=CARTESIAN_POINT('Ctrl Pts',(95.1816821868991,-0.63149341392484,-6.49999999999999));
#22556=CARTESIAN_POINT('Ctrl Pts',(95.2025223736644,-0.684949321759963,
-6.5));
#22557=CARTESIAN_POINT('Ctrl Pts',(95.2266387923791,-0.737074044746253,
-6.49999999999999));
#22558=CARTESIAN_POINT('Ctrl Pts',(95.2537356093761,-0.787653241889366,
-6.49999999999999));
#22559=CARTESIAN_POINT('Ctrl Pts',(95.280832426373,-0.838232439032478,-6.49999999999999));
#22560=CARTESIAN_POINT('Ctrl Pts',(95.3109101915958,-0.887266965797818,
-6.49999999999998));
#22561=CARTESIAN_POINT('Ctrl Pts',(95.3437265952813,-0.93453689164767,-6.49999999999999));
#22562=CARTESIAN_POINT('Ctrl Pts',(95.3644390346566,-0.964371832819955,
-6.5));
#22563=CARTESIAN_POINT('Ctrl Pts',(95.3862434920268,-0.993503667320148,
-6.49999999999998));
#22564=CARTESIAN_POINT('Ctrl Pts',(95.4090885081249,-1.02187358457514,-6.49999999999999));
#22565=CARTESIAN_POINT('Ctrl Pts',(95.4201840553492,-1.03565250927805,-6.49999999999999));
#22566=CARTESIAN_POINT('Ctrl Pts',(95.4315251653976,-1.04925165069866,-6.49999999999998));
#22567=CARTESIAN_POINT('Ctrl Pts',(95.4431064930379,-1.0626639234839,-6.49999999999999));
#22568=CARTESIAN_POINT('Ctrl Pts',(95.4503586859564,-1.07106264880577,-6.50000000000001));
#22569=CARTESIAN_POINT('Ctrl Pts',(95.457705080573,-1.07938809381907,-6.49999999999998));
#22570=CARTESIAN_POINT('Ctrl Pts',(95.4651444307094,-1.08763846447625,-6.49999999999998));
#22571=CARTESIAN_POINT('Ctrl Pts',(95.4727475267872,-1.09607043227366,-6.49999999999998));
#22572=CARTESIAN_POINT('Ctrl Pts',(95.4804419218002,-1.10441752546094,-6.5));
#22573=CARTESIAN_POINT('Ctrl Pts',(95.4882237216775,-1.11267593612413,-6.5));
#22574=CARTESIAN_POINT('Ctrl Pts',(95.5296481884137,-1.1566375212592,-6.49999999999998));
#22575=CARTESIAN_POINT('Ctrl Pts',(95.5735639857425,-1.19810830457877,-6.49999999999999));
#22576=CARTESIAN_POINT('Ctrl Pts',(95.6197151559512,-1.23683755194955,-6.49999999999999));
#22577=CARTESIAN_POINT('Ctrl Pts',(95.6520292546319,-1.26395497314833,-6.49999999999999));
#22578=CARTESIAN_POINT('Ctrl Pts',(95.6854403501075,-1.2897280483634,-6.5));
#22579=CARTESIAN_POINT('Ctrl Pts',(95.7198731814153,-1.31406219407389,-6.5));
#22580=CARTESIAN_POINT('Ctrl Pts',(95.7332874249566,-1.32354222068023,-6.5));
#22581=CARTESIAN_POINT('Ctrl Pts',(95.7468588681643,-1.33280488458279,-6.49999999999997));
#22582=CARTESIAN_POINT('Ctrl Pts',(95.7605632855576,-1.34183160585072,-6.49999999999998));
#22583=CARTESIAN_POINT('Ctrl Pts',(95.8113349748999,-1.37527351548072,-6.49999999999998));
#22584=CARTESIAN_POINT('Ctrl Pts',(95.863984835545,-1.40552072986475,-6.5));
#22585=CARTESIAN_POINT('Ctrl Pts',(95.9182746138887,-1.4323100669816,-6.49999999999999));
#22586=CARTESIAN_POINT('Ctrl Pts',(95.9495324392697,-1.44773426739684,-6.49999999999998));
#22587=CARTESIAN_POINT('Ctrl Pts',(95.9813346518669,-1.46201162597775,-6.49999999999999));
#22588=CARTESIAN_POINT('Ctrl Pts',(96.0136410264312,-1.47508602121386,-6.49999999999999));
#22589=CARTESIAN_POINT('Ctrl Pts',(96.0292107636313,-1.48138709648526,-6.49999999999998));
#22590=CARTESIAN_POINT('Ctrl Pts',(96.0448976513391,-1.4874086909893,-6.49999999999999));
#22591=CARTESIAN_POINT('Ctrl Pts',(96.0606948201728,-1.49315277804518,-6.49999999999999));
#22592=CARTESIAN_POINT('Ctrl Pts',(95.5022584080476,0.825087759517108,-4.99934226694474));
#22593=CARTESIAN_POINT('Ctrl Pts',(95.5066224930217,0.830156025949504,-4.99956151129649));
#22594=CARTESIAN_POINT('Ctrl Pts',(95.5110267897309,0.835189667628379,-4.99978075564824));
#22595=CARTESIAN_POINT('Ctrl Pts',(95.5154707437297,0.840188050881734,-4.99999999999999));
#22596=CARTESIAN_POINT('Ctrl Pts',(96.8593706716433,-1.49265850562707,-6.49883138166506));
#22597=CARTESIAN_POINT('Ctrl Pts',(97.3538985322231,-1.36050793369471,-6.47246692892639));
#22598=CARTESIAN_POINT('Ctrl Pts',(98.1927101176,-0.567444892518825,-6.41974069761678));
#22599=CARTESIAN_POINT('Ctrl Pts',(97.8816642045551,1.14476294416278,-6.34065268773623));
#22600=CARTESIAN_POINT('Ctrl Pts',(96.27607609225,1.81437997786543,-6.26156735202342));
#22601=CARTESIAN_POINT('Ctrl Pts',(94.8393525453763,0.835745259019781,-6.18248201631059));
#22602=CARTESIAN_POINT('Ctrl Pts',(94.8756583481607,-0.903059964588701,
-6.10339668059776));
#22603=CARTESIAN_POINT('Ctrl Pts',(96.35285946686,-1.82075086179174,-6.02431134488494));
#22604=CARTESIAN_POINT('Ctrl Pts',(97.9277575306634,-1.08347082117818,-5.94522600917211));
#22605=CARTESIAN_POINT('Ctrl Pts',(98.16895145999,0.638743852593271,-5.86614067345928));
#22606=CARTESIAN_POINT('Ctrl Pts',(96.8571024015692,1.78031043271048,-5.78705533774647));
#22607=CARTESIAN_POINT('Ctrl Pts',(95.1847346256529,1.30357333827821,-5.70797000203363));
#22608=CARTESIAN_POINT('Ctrl Pts',(94.6720252621149,-0.358131798728269,
-5.62888466632083));
#22609=CARTESIAN_POINT('Ctrl Pts',(95.7850374527541,-1.69428152784527,-5.54979933060799));
#22610=CARTESIAN_POINT('Ctrl Pts',(97.5120370344031,-1.49033385341736,-5.47071399489516));
#22611=CARTESIAN_POINT('Ctrl Pts',(98.2831532326639,0.0683764156440079,
-5.39162865918234));
#22612=CARTESIAN_POINT('Ctrl Pts',(97.3974682491448,1.56485490851585,-5.31254332346951));
#22613=CARTESIAN_POINT('Ctrl Pts',(95.6600052081528,1.63902976330342,-5.23345798775669));
#22614=CARTESIAN_POINT('Ctrl Pts',(94.6502843168414,0.222969934548651,-5.15437265204388));
#22615=CARTESIAN_POINT('Ctrl Pts',(95.2858253605478,-1.39504985668874,-5.07528731633104));
#22616=CARTESIAN_POINT('Ctrl Pts',(96.9895786983007,-1.74651069703396,-4.99620198061823));
#22617=CARTESIAN_POINT('Ctrl Pts',(98.2112489397104,-0.507268079750478,
-4.9171166449054));
#22618=CARTESIAN_POINT('Ctrl Pts',(97.965179897774,0.620476460483682,-4.86439308776351));
#22619=CARTESIAN_POINT('Ctrl Pts',(97.6311617451579,1.00829008801941,-4.83803130919258));
#22620=CARTESIAN_POINT('Ctrl Pts',(96.8350765218437,-1.40174899523043,-6.5531598419852));
#22621=CARTESIAN_POINT('Ctrl Pts',(97.2994854466366,-1.27764697810663,-6.52679538924653));
#22622=CARTESIAN_POINT('Ctrl Pts',(98.0872096933796,-0.532884986712179,
-6.47406915793692));
#22623=CARTESIAN_POINT('Ctrl Pts',(97.7951078533155,1.07504181345423,-6.39498114805637));
#22624=CARTESIAN_POINT('Ctrl Pts',(96.2873071643481,1.70387620567681,-6.31589581234354));
#22625=CARTESIAN_POINT('Ctrl Pts',(94.9380864412811,0.7848446732345,-6.23681047663072));
#22626=CARTESIAN_POINT('Ctrl Pts',(94.9721810599645,-0.848059615258915,
-6.1577251409179));
#22627=CARTESIAN_POINT('Ctrl Pts',(96.3594140915549,-1.70985907457065,-6.07863980520507));
#22628=CARTESIAN_POINT('Ctrl Pts',(97.838393891827,-1.01748265207518,-5.99955446949225));
#22629=CARTESIAN_POINT('Ctrl Pts',(98.0648980431881,0.599841524506028,-5.92046913377942));
#22630=CARTESIAN_POINT('Ctrl Pts',(96.8329463994579,1.67188164663409,-5.8413837980666));
#22631=CARTESIAN_POINT('Ctrl Pts',(95.2624332240001,1.22417995157775,-5.76229846235377));
#22632=CARTESIAN_POINT('Ctrl Pts',(94.7809501302615,-0.336319986879062,
-5.68321312664096));
#22633=CARTESIAN_POINT('Ctrl Pts',(95.8261749516296,-1.59109228289083,-5.60412779092812));
#22634=CARTESIAN_POINT('Ctrl Pts',(97.4479926140177,-1.3995659246306,-5.52504245521531));
#22635=CARTESIAN_POINT('Ctrl Pts',(98.1721444223804,0.0642119892561631,
-5.44595711950247));
#22636=CARTESIAN_POINT('Ctrl Pts',(97.3404015749321,1.4695483175986,-5.36687178378965));
#22637=CARTESIAN_POINT('Ctrl Pts',(95.7087577241924,1.53920559538711,-5.28778644807683));
#22638=CARTESIAN_POINT('Ctrl Pts',(94.7605333047936,0.209390078535656,-5.20870111236401));
#22639=CARTESIAN_POINT('Ctrl Pts',(95.3573670856515,-1.31008514508701,-5.12961577665117));
#22640=CARTESIAN_POINT('Ctrl Pts',(96.9573543032989,-1.64014046447823,-5.05053044093836));
#22641=CARTESIAN_POINT('Ctrl Pts',(98.1046194191596,-0.476373208220177,
-4.97144510522553));
#22642=CARTESIAN_POINT('Ctrl Pts',(97.8735370711266,0.582686697438373,-4.91872154808365));
#22643=CARTESIAN_POINT('Ctrl Pts',(97.5598621025699,0.946880758360905,-4.89235976951271));
#22644=CARTESIAN_POINT('Ctrl Pts',(96.8107823720442,-1.31083948483379,-6.60748830230534));
#22645=CARTESIAN_POINT('Ctrl Pts',(97.2450723610501,-1.19478602251856,-6.58112384956667));
#22646=CARTESIAN_POINT('Ctrl Pts',(97.9817092691592,-0.498325080905534,
-6.52839761825706));
#22647=CARTESIAN_POINT('Ctrl Pts',(97.7085515020758,1.00532068274568,-6.44930960837651));
#22648=CARTESIAN_POINT('Ctrl Pts',(96.2985382364459,1.5933724334882,-6.37022427266369));
#22649=CARTESIAN_POINT('Ctrl Pts',(95.0368203371858,0.733944087449216,-6.29113893695086));
#22650=CARTESIAN_POINT('Ctrl Pts',(95.0687037717685,-0.793059265929128,
-6.21205360123804));
#22651=CARTESIAN_POINT('Ctrl Pts',(96.3659687162497,-1.59896728734956,-6.13296826552521));
#22652=CARTESIAN_POINT('Ctrl Pts',(97.7490302529905,-0.951494482972173,
-6.05388292981239));
#22653=CARTESIAN_POINT('Ctrl Pts',(97.9608446263864,0.560939196418784,-5.97479759409956));
#22654=CARTESIAN_POINT('Ctrl Pts',(96.8087903973465,1.56345286055771,-5.89571225838674));
#22655=CARTESIAN_POINT('Ctrl Pts',(95.3401318223472,1.14478656487729,-5.81662692267391));
#22656=CARTESIAN_POINT('Ctrl Pts',(94.8898749984081,-0.314508175029856,
-5.73754158696109));
#22657=CARTESIAN_POINT('Ctrl Pts',(95.8673124505051,-1.48790303793639,-5.65845625124826));
#22658=CARTESIAN_POINT('Ctrl Pts',(97.3839481936324,-1.30879799584384,-5.57937091553545));
#22659=CARTESIAN_POINT('Ctrl Pts',(98.0611356120971,0.0600475628683185,
-5.50028557982261));
#22660=CARTESIAN_POINT('Ctrl Pts',(97.2833349007192,1.37424172668135,-5.4212002441098));
#22661=CARTESIAN_POINT('Ctrl Pts',(95.757510240232,1.43938142747079,-5.34211490839696));
#22662=CARTESIAN_POINT('Ctrl Pts',(94.8707822927458,0.19581022252266,-5.26302957268415));
#22663=CARTESIAN_POINT('Ctrl Pts',(95.4289088107553,-1.22512043348528,-5.18394423697132));
#22664=CARTESIAN_POINT('Ctrl Pts',(96.9251299082968,-1.53377023192249,-5.1048589012585));
#22665=CARTESIAN_POINT('Ctrl Pts',(97.9979898986088,-0.445478336689876,
-5.02577356554567));
#22666=CARTESIAN_POINT('Ctrl Pts',(97.7818942444792,0.544896934393064,-4.97305000840379));
#22667=CARTESIAN_POINT('Ctrl Pts',(97.488562459982,0.885471428702395,-4.94668822983285));
#22668=CARTESIAN_POINT('Ctrl Pts',(96.7864882222446,-1.21992997443715,-6.66181676262547));
#22669=CARTESIAN_POINT('Ctrl Pts',(97.1906592754635,-1.11192506693047,-6.6354523098868));
#22670=CARTESIAN_POINT('Ctrl Pts',(97.8762088449389,-0.463765175098888,
-6.5827260785772));
#22671=CARTESIAN_POINT('Ctrl Pts',(97.621995150836,0.935599552037132,-6.50363806869664));
#22672=CARTESIAN_POINT('Ctrl Pts',(96.3097693085439,1.48286866129958,-6.42455273298382));
#22673=CARTESIAN_POINT('Ctrl Pts',(95.1355542330906,0.683043501663935,-6.34546739727099));
#22674=CARTESIAN_POINT('Ctrl Pts',(95.1652264835723,-0.738058916599343,
-6.26638206155817));
#22675=CARTESIAN_POINT('Ctrl Pts',(96.3725233409445,-1.48807550012847,-6.18729672584535));
#22676=CARTESIAN_POINT('Ctrl Pts',(97.6596666141542,-0.885506313869171,
-6.10821139013252));
#22677=CARTESIAN_POINT('Ctrl Pts',(97.8567912095845,0.522036868331542,-6.02912605441969));
#22678=CARTESIAN_POINT('Ctrl Pts',(96.7846343952353,1.45502407448132,-5.95004071870687));
#22679=CARTESIAN_POINT('Ctrl Pts',(95.4178304206945,1.06539317817682,-5.87095538299404));
#22680=CARTESIAN_POINT('Ctrl Pts',(94.9987998665546,-0.29269636318065,-5.79187004728123));
#22681=CARTESIAN_POINT('Ctrl Pts',(95.9084499493806,-1.38471379298194,-5.71278471156839));
#22682=CARTESIAN_POINT('Ctrl Pts',(97.3199037732469,-1.21803006705708,-5.63369937585557));
#22683=CARTESIAN_POINT('Ctrl Pts',(97.9501268018138,0.0558831364804743,
-5.55461404014274));
#22684=CARTESIAN_POINT('Ctrl Pts',(97.2262682265065,1.2789351357641,-5.47552870442993));
#22685=CARTESIAN_POINT('Ctrl Pts',(95.8062627562716,1.33955725955447,-5.3964433687171));
#22686=CARTESIAN_POINT('Ctrl Pts',(94.9810312806979,0.182230366509664,-5.31735803300428));
#22687=CARTESIAN_POINT('Ctrl Pts',(95.500450535859,-1.14015572188355,-5.23827269729146));
#22688=CARTESIAN_POINT('Ctrl Pts',(96.8929055132947,-1.42739999936675,-5.15918736157863));
#22689=CARTESIAN_POINT('Ctrl Pts',(97.891360378058,-0.414583465159574,-5.0801020258658));
#22690=CARTESIAN_POINT('Ctrl Pts',(97.6902514178318,0.507107171347755,-5.02737846872392));
#22691=CARTESIAN_POINT('Ctrl Pts',(97.4172628173941,0.824062099043887,-5.00101669015298));
#22692=CARTESIAN_POINT('Ctrl Pts',(97.4185971022994,0.825211298936501,-4.99999999999999));
#22693=CARTESIAN_POINT('Ctrl Pts',(97.4554550558806,0.790790868711375,-4.99999999999997));
#22694=CARTESIAN_POINT('Ctrl Pts',(97.4899315734933,0.75413001564445,-4.99999999999998));
#22695=CARTESIAN_POINT('Ctrl Pts',(97.5220265074298,0.71554916654118,-4.99999999999999));
#22696=CARTESIAN_POINT('Ctrl Pts',(97.5555441517723,0.675258098136734,-4.99999999999999));
#22697=CARTESIAN_POINT('Ctrl Pts',(97.5864650020965,0.632872580965763,-4.99999999999998));
#22698=CARTESIAN_POINT('Ctrl Pts',(97.6147608454724,0.588707955597061,-4.99999999999997));
#22699=CARTESIAN_POINT('Ctrl Pts',(97.6377328401419,0.552852882289196,-4.99999999999997));
#22700=CARTESIAN_POINT('Ctrl Pts',(97.6589742582729,0.515824041492352,-4.99999999999997));
#22701=CARTESIAN_POINT('Ctrl Pts',(97.6784530940387,0.477771520420676,-4.99999999999998));
#22702=CARTESIAN_POINT('Ctrl Pts',(97.6872340438242,0.460617657594326,-4.99999999999999));
#22703=CARTESIAN_POINT('Ctrl Pts',(97.6956565880827,0.443255574531325,-5.));
#22704=CARTESIAN_POINT('Ctrl Pts',(97.7037166414093,0.425698195714689,-4.99999999999998));
#22705=CARTESIAN_POINT('Ctrl Pts',(97.7073861170761,0.417704901907484,-4.99999999999997));
#22706=CARTESIAN_POINT('Ctrl Pts',(97.7109794186128,0.409673231731474,-5.));
#22707=CARTESIAN_POINT('Ctrl Pts',(97.7144928114126,0.401612710819986,-5.00000000000001));
#22708=CARTESIAN_POINT('Ctrl Pts',(97.7364622700353,0.351209783867421,-5.00000000000001));
#22709=CARTESIAN_POINT('Ctrl Pts',(97.7553517923287,0.299592241161254,-4.99999999999999));
#22710=CARTESIAN_POINT('Ctrl Pts',(97.7711347217224,0.24710214790481,-4.99999999999999));
#22711=CARTESIAN_POINT('Ctrl Pts',(97.7869025056492,0.194662424700384,-4.99999999999998));
#22712=CARTESIAN_POINT('Ctrl Pts',(97.7995701097015,0.141350806312005,-4.99999999999997));
#22713=CARTESIAN_POINT('Ctrl Pts',(97.8090712523609,0.0874748631209174,
-4.99999999999998));
#22714=CARTESIAN_POINT('Ctrl Pts',(97.8160590828384,0.0478505809339526,
-4.99999999999999));
#22715=CARTESIAN_POINT('Ctrl Pts',(97.8213333251037,0.00792027680426406,
-5.));
#22716=CARTESIAN_POINT('Ctrl Pts',(97.8248516812115,-0.0322003712787191,
-4.99999999999999));
#22717=CARTESIAN_POINT('Ctrl Pts',(97.8262653010745,-0.0483202134177673,
-4.99999999999999));
#22718=CARTESIAN_POINT('Ctrl Pts',(97.82739530449,-0.0644708240410482,-5.));
#22719=CARTESIAN_POINT('Ctrl Pts',(97.8282382678351,-0.0806448146134011,
-4.99999999999999));
#22720=CARTESIAN_POINT('Ctrl Pts',(97.8287697686908,-0.0908427548658557,
-4.99999999999999));
#22721=CARTESIAN_POINT('Ctrl Pts',(97.8291866912673,-0.101041906912261,
-5.00000000000002));
#22722=CARTESIAN_POINT('Ctrl Pts',(97.8294886059173,-0.11123560581186,-5.00000000000002));
#22723=CARTESIAN_POINT('Ctrl Pts',(97.8311712794237,-0.16804857289554,-5.00000000000001));
#22724=CARTESIAN_POINT('Ctrl Pts',(97.8292877502248,-0.224736405431888,
-4.99999999999998));
#22725=CARTESIAN_POINT('Ctrl Pts',(97.823779668819,-0.280965921284123,-4.99999999999997));
#22726=CARTESIAN_POINT('Ctrl Pts',(97.820139920031,-0.318122473102923,-4.99999999999996));
#22727=CARTESIAN_POINT('Ctrl Pts',(97.8149165772873,-0.355079507520968,
-4.99999999999997));
#22728=CARTESIAN_POINT('Ctrl Pts',(97.8080808838596,-0.391744685765442,
-4.99999999999998));
#22729=CARTESIAN_POINT('Ctrl Pts',(97.7979995113489,-0.445818983269784,
-5.));
#22730=CARTESIAN_POINT('Ctrl Pts',(97.7844137192366,-0.499259046888469,
-4.99999999999999));
#22731=CARTESIAN_POINT('Ctrl Pts',(97.7675497811822,-0.551862678807369,
-5.));
#22732=CARTESIAN_POINT('Ctrl Pts',(97.7629133729061,-0.566325013381729,
-5.));
#22733=CARTESIAN_POINT('Ctrl Pts',(97.758028879005,-0.580724091132068,-5.));
#22734=CARTESIAN_POINT('Ctrl Pts',(97.7529003368896,-0.595055597017538,
-5.));
#22735=CARTESIAN_POINT('Ctrl Pts',(97.7485342959591,-0.607256323829169,
-5.00000000000001));
#22736=CARTESIAN_POINT('Ctrl Pts',(97.7439899576327,-0.61941131482884,-4.99999999999998));
#22737=CARTESIAN_POINT('Ctrl Pts',(97.7392796121955,-0.631493538889831,
-4.99999999999998));
#22738=CARTESIAN_POINT('Ctrl Pts',(97.7188419797954,-0.683916881769837,
-5.));
#22739=CARTESIAN_POINT('Ctrl Pts',(97.6952532881221,-0.735059967855329,
-4.99999999999998));
#22740=CARTESIAN_POINT('Ctrl Pts',(97.6687930745268,-0.78472064231593,-4.99999999999999));
#22741=CARTESIAN_POINT('Ctrl Pts',(97.6414632614169,-0.836013385930035,
-5.));
#22742=CARTESIAN_POINT('Ctrl Pts',(97.611069818818,-0.88572557878977,-4.99999999999998));
#22743=CARTESIAN_POINT('Ctrl Pts',(97.5778652315618,-0.933628810807292,
-4.99999999999999));
#22744=CARTESIAN_POINT('Ctrl Pts',(97.55696507361,-0.963780822872587,-5.));
#22745=CARTESIAN_POINT('Ctrl Pts',(97.5349500727209,-0.993215986882425,
-4.99999999999999));
#22746=CARTESIAN_POINT('Ctrl Pts',(97.5118733059413,-1.02187370244541,-4.99999999999999));
#22747=CARTESIAN_POINT('Ctrl Pts',(97.5007777616897,-1.03565262365284,-4.99999999999999));
#22748=CARTESIAN_POINT('Ctrl Pts',(97.4894366547208,-1.04925176160035,-4.99999999999997));
#22749=CARTESIAN_POINT('Ctrl Pts',(97.4778553302579,-1.06266403094416,-4.99999999999998));
#22750=CARTESIAN_POINT('Ctrl Pts',(97.4706031339387,-1.07106276035367,-4.99999999999998));
#22751=CARTESIAN_POINT('Ctrl Pts',(97.4632567358199,-1.07938820935805,-4.99999999999998));
#22752=CARTESIAN_POINT('Ctrl Pts',(97.4558173820803,-1.08763858390813,-4.99999999999999));
#22753=CARTESIAN_POINT('Ctrl Pts',(97.448214291688,-1.09607054529482,-5.));
#22754=CARTESIAN_POINT('Ctrl Pts',(97.4405199025075,-1.10441763214809,-4.99999999999998));
#22755=CARTESIAN_POINT('Ctrl Pts',(97.4327381085711,-1.11267603659566,-4.99999999999998));
#22756=CARTESIAN_POINT('Ctrl Pts',(97.3913123727389,-1.15663896902978,-5.));
#22757=CARTESIAN_POINT('Ctrl Pts',(97.3473951534589,-1.19811094637215,-5.));
#22758=CARTESIAN_POINT('Ctrl Pts',(97.3012424311067,-1.23684121121544,-4.99999999999999));
#22759=CARTESIAN_POINT('Ctrl Pts',(97.268929657142,-1.26395732115855,-4.99999999999999));
#22760=CARTESIAN_POINT('Ctrl Pts',(97.2355199860345,-1.2897291990635,-4.99999999999999));
#22761=CARTESIAN_POINT('Ctrl Pts',(97.2010886685523,-1.31406227375371,-4.99999999999998));
#22762=CARTESIAN_POINT('Ctrl Pts',(97.1876744276178,-1.32354229805831,-4.99999999999997));
#22763=CARTESIAN_POINT('Ctrl Pts',(97.1741029870343,-1.33280495971514,-5.));
#22764=CARTESIAN_POINT('Ctrl Pts',(97.1603985722682,-1.34183167880629,-4.99999999999999));
#22765=CARTESIAN_POINT('Ctrl Pts',(97.109626887535,-1.37527358374674,-4.99999999999998));
#22766=CARTESIAN_POINT('Ctrl Pts',(97.0569770311592,-1.40552079373867,-4.99999999999998));
#22767=CARTESIAN_POINT('Ctrl Pts',(97.0026872565067,-1.43231012699531,-4.99999999999998));
#22768=CARTESIAN_POINT('Ctrl Pts',(96.9714294348054,-1.44773432442092,-4.99999999999998));
#22769=CARTESIAN_POINT('Ctrl Pts',(96.9396272257503,-1.46201168030251,-4.99999999999999));
#22770=CARTESIAN_POINT('Ctrl Pts',(96.9073208545389,-1.47508607318309,-4.99999999999999));
#22771=CARTESIAN_POINT('Ctrl Pts',(96.8916875526902,-1.4814128725953,-4.99999999999999));
#22772=CARTESIAN_POINT('Ctrl Pts',(96.8759361418645,-1.48745790481111,-4.99999999999999));
#22773=CARTESIAN_POINT('Ctrl Pts',(96.8600735756126,-1.49322316678187,-4.99999999999999));
#22774=CARTESIAN_POINT('Ctrl Pts',(96.8589947914343,-1.49064942821851,-6.49999999999999));
#22775=CARTESIAN_POINT('Ctrl Pts',(96.9148518906818,-1.47023947405498,-6.49999999999999));
#22776=CARTESIAN_POINT('Ctrl Pts',(96.969228063587,-1.44640480416822,-6.5));
#22777=CARTESIAN_POINT('Ctrl Pts',(97.021942725396,-1.41942415227612,-6.49999999999999));
#22778=CARTESIAN_POINT('Ctrl Pts',(97.0758376502637,-1.39183941291317,-6.49999999999999));
#22779=CARTESIAN_POINT('Ctrl Pts',(97.1279966319397,-1.36096545034004,-6.49999999999999));
#22780=CARTESIAN_POINT('Ctrl Pts',(97.1781953688626,-1.32705566669257,-6.49999999999998));
#22781=CARTESIAN_POINT('Ctrl Pts',(97.2181578764102,-1.30006056546066,-6.49999999999998));
#22782=CARTESIAN_POINT('Ctrl Pts',(97.2568775916097,-1.27114046090819,-6.49999999999998));
#22783=CARTESIAN_POINT('Ctrl Pts',(97.2942225391991,-1.24040893115648,-6.49999999999999));
#22784=CARTESIAN_POINT('Ctrl Pts',(97.3132807037093,-1.22472577754498,-6.49999999999999));
#22785=CARTESIAN_POINT('Ctrl Pts',(97.3319805387447,-1.20857069716563,-6.5));
#22786=CARTESIAN_POINT('Ctrl Pts',(97.3503025175037,-1.1919579355381,-6.50000000000001));
#22787=CARTESIAN_POINT('Ctrl Pts',(97.3580211211267,-1.18495938348356,-6.50000000000001));
#22788=CARTESIAN_POINT('Ctrl Pts',(97.3656724961627,-1.17787960881166,-6.49999999999999));
#22789=CARTESIAN_POINT('Ctrl Pts',(97.3732450181154,-1.17072958174374,-6.49999999999999));
#22790=CARTESIAN_POINT('Ctrl Pts',(97.4162534779211,-1.13012069956669,-6.49999999999998));
#22791=CARTESIAN_POINT('Ctrl Pts',(97.4568080454813,-1.08717098043465,-6.49999999999999));
#22792=CARTESIAN_POINT('Ctrl Pts',(97.4947031586331,-1.04212172111347,-6.5));
#22793=CARTESIAN_POINT('Ctrl Pts',(97.5319288757374,-0.997868231843363,
-6.50000000000001));
#22794=CARTESIAN_POINT('Ctrl Pts',(97.5665887281823,-0.951587784658056,
-6.5));
#22795=CARTESIAN_POINT('Ctrl Pts',(97.5984446961916,-0.903485955601459,
-6.5));
#22796=CARTESIAN_POINT('Ctrl Pts',(97.6220018485104,-0.867915160403415,
-6.49999999999999));
#22797=CARTESIAN_POINT('Ctrl Pts',(97.6440248688239,-0.831347822374541,
-6.50000000000002));
#22798=CARTESIAN_POINT('Ctrl Pts',(97.6643996535905,-0.793863066977394,
-6.50000000000002));
#22799=CARTESIAN_POINT('Ctrl Pts',(97.6747826326615,-0.774760856317049,
-6.50000000000002));
#22800=CARTESIAN_POINT('Ctrl Pts',(97.684737320669,-0.755420366979109,-6.49999999999998));
#22801=CARTESIAN_POINT('Ctrl Pts',(97.6942469201329,-0.735851988628946,
-6.49999999999999));
#22802=CARTESIAN_POINT('Ctrl Pts',(97.699137314062,-0.725788780493837,-6.5));
#22803=CARTESIAN_POINT('Ctrl Pts',(97.7039061953277,-0.715672975917219,
-6.5));
#22804=CARTESIAN_POINT('Ctrl Pts',(97.708549248637,-0.705511994572704,-6.5));
#22805=CARTESIAN_POINT('Ctrl Pts',(97.7317129543623,-0.654819924922506,
-6.5));
#22806=CARTESIAN_POINT('Ctrl Pts',(97.7517710748817,-0.602958770123721,
-6.49999999999999));
#22807=CARTESIAN_POINT('Ctrl Pts',(97.7685108178151,-0.550120111169122,
-6.5));
#22808=CARTESIAN_POINT('Ctrl Pts',(97.7803018950071,-0.512901815229096,
-6.5));
#22809=CARTESIAN_POINT('Ctrl Pts',(97.790445640772,-0.475198144298214,-6.50000000000002));
#22810=CARTESIAN_POINT('Ctrl Pts',(97.7988522195133,-0.437073871454044,
-6.5));
#22811=CARTESIAN_POINT('Ctrl Pts',(97.8107530971982,-0.383102770735259,
-6.49999999999999));
#22812=CARTESIAN_POINT('Ctrl Pts',(97.8191740018439,-0.32828772595591,-6.50000000000001));
#22813=CARTESIAN_POINT('Ctrl Pts',(97.8241717830776,-0.272944848744542,
-6.50000000000001));
#22814=CARTESIAN_POINT('Ctrl Pts',(97.8255977119158,-0.257154840956551,
-6.50000000000001));
#22815=CARTESIAN_POINT('Ctrl Pts',(97.8267447109837,-0.241321952605189,
-6.49999999999999));
#22816=CARTESIAN_POINT('Ctrl Pts',(97.8276134568352,-0.225453786835658,
-6.49999999999999));
#22817=CARTESIAN_POINT('Ctrl Pts',(97.8282845514555,-0.213195839747077,
-6.49999999999999));
#22818=CARTESIAN_POINT('Ctrl Pts',(97.8287895308168,-0.200914145342743,
-6.50000000000002));
#22819=CARTESIAN_POINT('Ctrl Pts',(97.8291283651393,-0.188635953585735,
-6.50000000000002));
#22820=CARTESIAN_POINT('Ctrl Pts',(97.8306666185408,-0.132894935106274,
-6.50000000000001));
#22821=CARTESIAN_POINT('Ctrl Pts',(97.8287921295153,-0.0771241131303391,
-6.49999999999998));
#22822=CARTESIAN_POINT('Ctrl Pts',(97.8236138439893,-0.0216417887842293,
-6.49999999999998));
#22823=CARTESIAN_POINT('Ctrl Pts',(97.8184586382926,0.0335932485862221,
-6.49999999999998));
#22824=CARTESIAN_POINT('Ctrl Pts',(97.8100285278727,0.0885434810548811,
-6.49999999999998));
#22825=CARTESIAN_POINT('Ctrl Pts',(97.7983820026397,0.142879636166974,-6.49999999999997));
#22826=CARTESIAN_POINT('Ctrl Pts',(97.7912147600914,0.176317970351754,-6.49999999999997));
#22827=CARTESIAN_POINT('Ctrl Pts',(97.7828284861102,0.20952337641607,-6.49999999999998));
#22828=CARTESIAN_POINT('Ctrl Pts',(97.7732287174118,0.242413466567256,-6.49999999999998));
#22829=CARTESIAN_POINT('Ctrl Pts',(97.7682438685886,0.259492224643258,-6.49999999999999));
#22830=CARTESIAN_POINT('Ctrl Pts',(97.7629317185495,0.276485877210698,-6.49999999999999));
#22831=CARTESIAN_POINT('Ctrl Pts',(97.7572924498035,0.29338227003039,-6.49999999999999));
#22832=CARTESIAN_POINT('Ctrl Pts',(97.7530778601672,0.306010035309496,-6.49999999999998));
#22833=CARTESIAN_POINT('Ctrl Pts',(97.7486797092745,0.318585317329429,-6.5));
#22834=CARTESIAN_POINT('Ctrl Pts',(97.7441059086613,0.331082408575578,-6.5));
#22835=CARTESIAN_POINT('Ctrl Pts',(97.7256779487625,0.381433509511468,-6.49999999999998));
#22836=CARTESIAN_POINT('Ctrl Pts',(97.7043779291848,0.430592810395182,-6.49999999999997));
#22837=CARTESIAN_POINT('Ctrl Pts',(97.6802507744572,0.478247335619807,-6.49999999999998));
#22838=CARTESIAN_POINT('Ctrl Pts',(97.6639796936088,0.510385009600785,-6.49999999999999));
#22839=CARTESIAN_POINT('Ctrl Pts',(97.6464219739521,0.541837784449329,-6.5));
#22840=CARTESIAN_POINT('Ctrl Pts',(97.6275821154523,0.57249994485488,-6.49999999999999));
#22841=CARTESIAN_POINT('Ctrl Pts',(97.619095628227,0.586311833759779,-6.49999999999998));
#22842=CARTESIAN_POINT('Ctrl Pts',(97.6103465210592,0.599966374158017,-6.49999999999999));
#22843=CARTESIAN_POINT('Ctrl Pts',(97.6013503158627,0.613431031783383,-6.49999999999999));
#22844=CARTESIAN_POINT('Ctrl Pts',(97.5728921081116,0.656024549342588,-6.49999999999999));
#22845=CARTESIAN_POINT('Ctrl Pts',(97.5419381864423,0.696765175184464,-6.49999999999999));
#22846=CARTESIAN_POINT('Ctrl Pts',(97.508512803874,0.735352656153272,-6.49999999999998));
#22847=CARTESIAN_POINT('Ctrl Pts',(97.4899618010268,0.756768610566281,-6.49999999999998));
#22848=CARTESIAN_POINT('Ctrl Pts',(97.4706489644052,0.777520682032755,-6.5));
#22849=CARTESIAN_POINT('Ctrl Pts',(97.4505745920965,0.797551681714772,-6.49999999999998));
#22850=CARTESIAN_POINT('Ctrl Pts',(97.4407183312139,0.807386647190681,-6.49999999999998));
#22851=CARTESIAN_POINT('Ctrl Pts',(97.4306784432458,0.817047710133597,-6.49999999999998));
#22852=CARTESIAN_POINT('Ctrl Pts',(97.4204606728957,0.82653245194677,-6.49999999999997));
#22853=CARTESIAN_POINT('Origin',(96.460480949577,-1.35113193175836E-15,
-6.49999999999999));
#22854=CARTESIAN_POINT('',(97.6151814879562,-2.,-6.49999999999999));
#22855=CARTESIAN_POINT('',(95.3057804111977,-2.,-6.49999999999999));
#22856=CARTESIAN_POINT('',(97.6151814879562,-2.,-6.49999999999999));
#22857=CARTESIAN_POINT('',(94.1510798728185,-2.7389107125398E-15,-6.49999999999999));
#22858=CARTESIAN_POINT('',(95.3057804111977,-2.,-6.49999999999999));
#22859=CARTESIAN_POINT('',(95.3057804111977,2.,-6.49999999999999));
#22860=CARTESIAN_POINT('',(94.1510798728185,-2.7389107125398E-15,-6.49999999999999));
#22861=CARTESIAN_POINT('',(97.6151814879562,2.,-6.49999999999999));
#22862=CARTESIAN_POINT('',(95.3057804111977,2.,-6.49999999999999));
#22863=CARTESIAN_POINT('',(98.7698820263355,4.52980483257521E-16,-6.49999999999999));
#22864=CARTESIAN_POINT('',(97.6151814879562,2.,-6.49999999999999));
#22865=CARTESIAN_POINT('',(98.7698820263355,4.52980483257521E-16,-6.49999999999999));
#22866=CARTESIAN_POINT('Origin',(94.1510798728185,-2.7389107125398E-15,
-6.49999999999999));
#22867=CARTESIAN_POINT('',(95.3057804111977,-2.,-4.99999999999999));
#22868=CARTESIAN_POINT('',(95.3057804111977,-2.,-6.49999999999999));
#22869=CARTESIAN_POINT('',(94.1510798728185,-2.5552136926677E-15,-4.99999999999999));
#22870=CARTESIAN_POINT('',(95.3057804111977,-2.,-4.99999999999999));
#22871=CARTESIAN_POINT('',(94.1510798728185,-2.7389107125398E-15,-6.49999999999999));
#22872=CARTESIAN_POINT('Origin',(95.3057804111977,2.,-6.49999999999999));
#22873=CARTESIAN_POINT('',(95.3057804111977,2.,-4.99999999999999));
#22874=CARTESIAN_POINT('',(94.1510798728185,-2.5552136926677E-15,-4.99999999999999));
#22875=CARTESIAN_POINT('',(95.3057804111977,2.,-6.49999999999999));
#22876=CARTESIAN_POINT('Origin',(97.6151814879562,2.,-6.49999999999999));
#22877=CARTESIAN_POINT('',(97.6151814879562,2.,-4.99999999999999));
#22878=CARTESIAN_POINT('',(95.3057804111977,2.,-4.99999999999999));
#22879=CARTESIAN_POINT('',(97.6151814879562,2.,-6.49999999999999));
#22880=CARTESIAN_POINT('Origin',(98.7698820263355,5.91758361335666E-16,
-6.49999999999999));
#22881=CARTESIAN_POINT('',(98.7698820263355,6.36677503129625E-16,-4.99999999999999));
#22882=CARTESIAN_POINT('',(97.6151814879562,2.,-4.99999999999999));
#22883=CARTESIAN_POINT('',(98.7698820263355,4.52980483257521E-16,-6.49999999999999));
#22884=CARTESIAN_POINT('Origin',(97.6151814879562,-2.,-6.49999999999999));
#22885=CARTESIAN_POINT('',(97.6151814879562,-2.,-4.99999999999999));
#22886=CARTESIAN_POINT('',(98.7698820263355,6.36677503129624E-16,-4.99999999999999));
#22887=CARTESIAN_POINT('',(97.6151814879562,-2.,-6.49999999999999));
#22888=CARTESIAN_POINT('Origin',(95.3057804111977,-2.,-6.49999999999999));
#22889=CARTESIAN_POINT('',(97.6151814879562,-2.,-4.99999999999999));
#22890=CARTESIAN_POINT('Origin',(96.460480949577,-1.16743491188625E-15,
-4.99999999999999));
#22891=CARTESIAN_POINT('',(0.,0.,0.));
#22892=CARTESIAN_POINT('Origin',(96.460480949577,-7.19464945638997E-16,
0.924367114736168));
#22893=CARTESIAN_POINT('',(95.9218016724468,1.04733934275882,-0.262495071028826));
#22894=CARTESIAN_POINT('',(95.9218016730721,1.04733934308042,-0.162850753546055));
#22895=CARTESIAN_POINT('',(95.9218016730721,1.04733934308042,0.924367114736168));
#22896=CARTESIAN_POINT('',(97.1339231275304,-0.966214621837945,-5.34765442106351E-14));
#22897=CARTESIAN_POINT('Ctrl Pts',(95.9218016724468,1.04733934275882,-0.262495071028825));
#22898=CARTESIAN_POINT('Ctrl Pts',(95.9168323908224,1.04478348629092,-0.262102466988266));
#22899=CARTESIAN_POINT('Ctrl Pts',(95.9118812731618,1.04219225000779,-0.261708746243414));
#22900=CARTESIAN_POINT('Ctrl Pts',(95.8615982372324,1.01541830112118,-0.257684079597526));
#22901=CARTESIAN_POINT('Ctrl Pts',(95.817881247505,0.988331638390339,-0.253964206255137));
#22902=CARTESIAN_POINT('Ctrl Pts',(95.7085732743141,0.910280094927417,-0.244136329072671));
#22903=CARTESIAN_POINT('Ctrl Pts',(95.6463469511429,0.855080568629144,-0.237981412999409));
#22904=CARTESIAN_POINT('Ctrl Pts',(95.5848295257772,0.787653983866887,-0.231596017471511));
#22905=CARTESIAN_POINT('Ctrl Pts',(95.5792897742812,0.781451429369945,-0.231018128933633));
#22906=CARTESIAN_POINT('Ctrl Pts',(95.5711678613817,0.772161563912934,-0.23016722728284));
#22907=CARTESIAN_POINT('Ctrl Pts',(95.5685352158595,0.769119014787333,-0.229890832536729));
#22908=CARTESIAN_POINT('Ctrl Pts',(95.5640451150508,0.763875742122085,-0.229418511236026));
#22909=CARTESIAN_POINT('Ctrl Pts',(95.5621800667519,0.761681612745837,-0.229222048236102));
#22910=CARTESIAN_POINT('Ctrl Pts',(95.5583052004454,0.757089011804468,-0.228813334904457));
#22911=CARTESIAN_POINT('Ctrl Pts',(95.5562968797751,0.754689354806667,-0.228601202842244));
#22912=CARTESIAN_POINT('Ctrl Pts',(95.5513891953363,0.748777660595372,-0.228082015489454));
#22913=CARTESIAN_POINT('Ctrl Pts',(95.5485005544082,0.745256709583808,-0.227775722724851));
#22914=CARTESIAN_POINT('Ctrl Pts',(95.5379805653814,0.732281179789277,-0.226657282874926));
#22915=CARTESIAN_POINT('Ctrl Pts',(95.5304749108787,0.72272503882737,-0.225853512167293));
#22916=CARTESIAN_POINT('Ctrl Pts',(95.5118553269796,0.698248202961025,-0.223839659051407));
#22917=CARTESIAN_POINT('Ctrl Pts',(95.5009442470649,0.683176785131831,-0.222640720972597));
#22918=CARTESIAN_POINT('Ctrl Pts',(95.4527554960439,0.613180375978137,-0.217225437062142));
#22919=CARTESIAN_POINT('Ctrl Pts',(95.4198033491736,0.555420689895478,-0.21317042092782));
#22920=CARTESIAN_POINT('Ctrl Pts',(95.3622453187482,0.431213720152704,-0.204691697395776));
#22921=CARTESIAN_POINT('Ctrl Pts',(95.3384078824534,0.364714717858227,-0.200274417096875));
#22922=CARTESIAN_POINT('Ctrl Pts',(95.3180297803759,0.286373245568453,-0.194964067220175));
#22923=CARTESIAN_POINT('Ctrl Pts',(95.3155333865259,0.276223417137716,-0.194274339566029));
#22924=CARTESIAN_POINT('Ctrl Pts',(95.3116539451387,0.259493289874712,-0.193133956989658));
#22925=CARTESIAN_POINT('Ctrl Pts',(95.3101915379279,0.252931848328484,-0.192685831511372));
#22926=CARTESIAN_POINT('Ctrl Pts',(95.3076564554833,0.241080644457487,-0.191874692369414));
#22927=CARTESIAN_POINT('Ctrl Pts',(95.3065638111565,0.235795308068159,-0.191512324206385));
#22928=CARTESIAN_POINT('Ctrl Pts',(95.3043029214912,0.22446673289002,-0.190734210525823));
#22929=CARTESIAN_POINT('Ctrl Pts',(95.3031456501842,0.218421494097882,-0.190318129003744));
#22930=CARTESIAN_POINT('Ctrl Pts',(95.3001190491258,0.201911669313706,-0.189179310361597));
#22931=CARTESIAN_POINT('Ctrl Pts',(95.2983439662919,0.191430617664011,-0.188453631496875));
#22932=CARTESIAN_POINT('Ctrl Pts',(95.2890156874044,0.131428770594929,-0.184282638221013));
#22933=CARTESIAN_POINT('Ctrl Pts',(95.2844871441334,0.0814967000799421,
-0.180743822486812));
#22934=CARTESIAN_POINT('Ctrl Pts',(95.2818161501703,-0.0185434480269267,
-0.173526918471726));
#22935=CARTESIAN_POINT('Ctrl Pts',(95.2836655013368,-0.0685522922392763,
-0.169856405756507));
#22936=CARTESIAN_POINT('Ctrl Pts',(95.2898734133365,-0.13004909239642,-0.165319055376679));
#22937=CARTESIAN_POINT('Ctrl Pts',(95.2912375276573,-0.141790670241545,
-0.164451831728975));
#22938=CARTESIAN_POINT('Ctrl Pts',(95.2995472056142,-0.204999889568257,
-0.159783082837273));
#22939=CARTESIAN_POINT('Ctrl Pts',(95.3097154142873,-0.255992341042425,
-0.156013580207507));
#22940=CARTESIAN_POINT('Ctrl Pts',(95.3248847675913,-0.312341902781773,
-0.151952114068799));
#22941=CARTESIAN_POINT('Ctrl Pts',(95.3266016223442,-0.318518176262677,
-0.151508421645522));
#22942=CARTESIAN_POINT('Ctrl Pts',(95.3294493942366,-0.328447934975755,
-0.150797795129124));
#22943=CARTESIAN_POINT('Ctrl Pts',(95.3305487434164,-0.332210228268276,
-0.150529175473158));
#22944=CARTESIAN_POINT('Ctrl Pts',(95.3325349181096,-0.338883567439533,
-0.150053920071292));
#22945=CARTESIAN_POINT('Ctrl Pts',(95.3334142571126,-0.341796713741235,
-0.14984687062544));
#22946=CARTESIAN_POINT('Ctrl Pts',(95.3353525669371,-0.348129283328287,
-0.149397692909303));
#22947=CARTESIAN_POINT('Ctrl Pts',(95.3364158395737,-0.351547300740957,
-0.14915581422261));
#22948=CARTESIAN_POINT('Ctrl Pts',(95.3394686084005,-0.361205326566207,
-0.148473820040189));
#22949=CARTESIAN_POINT('Ctrl Pts',(95.3414946324133,-0.367433781589195,
-0.148035736328086));
#22950=CARTESIAN_POINT('Ctrl Pts',(95.3553690263957,-0.408907424332733,
-0.145128237207898));
#22951=CARTESIAN_POINT('Ctrl Pts',(95.368830142273,-0.44359528065562,-0.142742616817202));
#22952=CARTESIAN_POINT('Ctrl Pts',(95.4054551811603,-0.526154102342101,
-0.137046987745201));
#22953=CARTESIAN_POINT('Ctrl Pts',(95.4302607539313,-0.573205319099704,
-0.13378385334963));
#22954=CARTESIAN_POINT('Ctrl Pts',(95.496835198365,-0.681107281832769,-0.12592896825162));
#22955=CARTESIAN_POINT('Ctrl Pts',(95.5413003738846,-0.740017028192766,
-0.121320580631259));
#22956=CARTESIAN_POINT('Ctrl Pts',(95.5980112425028,-0.802091024433251,
-0.115801343177005));
#22957=CARTESIAN_POINT('Ctrl Pts',(95.6051533128247,-0.809702803253676,
-0.115112184838288));
#22958=CARTESIAN_POINT('Ctrl Pts',(95.6170852467238,-0.822085416853332,
-0.113969799383936));
#22959=CARTESIAN_POINT('Ctrl Pts',(95.6218167913321,-0.826911827637914,
-0.113519043179907));
#22960=CARTESIAN_POINT('Ctrl Pts',(95.6304431432331,-0.835560938291993,
-0.112701108714745));
#22961=CARTESIAN_POINT('Ctrl Pts',(95.6343235027868,-0.839397827593819,
-0.112334562682231));
#22962=CARTESIAN_POINT('Ctrl Pts',(95.6427106780903,-0.847576549442378,
-0.111545150971558));
#22963=CARTESIAN_POINT('Ctrl Pts',(95.6472256985851,-0.851909689011483,
-0.11112192935171));
#22964=CARTESIAN_POINT('Ctrl Pts',(95.6596994538843,-0.863691425957646,
-0.109957264320697));
#22965=CARTESIAN_POINT('Ctrl Pts',(95.6677272361081,-0.871065680151812,
-0.109212740924639));
#22966=CARTESIAN_POINT('Ctrl Pts',(95.7162031223826,-0.91437003037409,-0.104745218885447));
#22967=CARTESIAN_POINT('Ctrl Pts',(95.7589798171695,-0.9475846564076,-0.100913910332391));
#22968=CARTESIAN_POINT('Ctrl Pts',(95.8430555670714,-1.00404561387092,-0.0935930913100962));
#22969=CARTESIAN_POINT('Ctrl Pts',(95.8837732202382,-1.0279734928091,-0.0901297649956015));
#22970=CARTESIAN_POINT('Ctrl Pts',(95.9764607364817,-1.0751978665864,-0.0825046897981003));
#22971=CARTESIAN_POINT('Ctrl Pts',(96.0289143655834,-1.09730470165327,-0.0783539314668988));
#22972=CARTESIAN_POINT('Ctrl Pts',(96.0922356957895,-1.11874505103074,-0.0736682238755853));
#22973=CARTESIAN_POINT('Ctrl Pts',(96.1017480195882,-1.12183143004247,-0.072972763418035));
#22974=CARTESIAN_POINT('Ctrl Pts',(96.1150848051069,-1.12597170499654,-0.0720104997719221));
#22975=CARTESIAN_POINT('Ctrl Pts',(96.1188767081283,-1.12712790774487,-0.071738345647365));
#22976=CARTESIAN_POINT('Ctrl Pts',(96.1256655444289,-1.12916050925448,-0.0712537444420071));
#22977=CARTESIAN_POINT('Ctrl Pts',(96.1286602441681,-1.13004417240052,-0.0710408970244024));
#22978=CARTESIAN_POINT('Ctrl Pts',(96.1347808419727,-1.13182378288448,-0.0706077883512765));
#22979=CARTESIAN_POINT('Ctrl Pts',(96.1379069616128,-1.13271870229142,-0.0703875820424255));
#22980=CARTESIAN_POINT('Ctrl Pts',(96.1456145631442,-1.13489067370124,-0.0698470345285675));
#22981=CARTESIAN_POINT('Ctrl Pts',(96.1502001987723,-1.13615295630171,-0.0695275026503178));
#22982=CARTESIAN_POINT('Ctrl Pts',(96.1603216789144,-1.13887323421163,-0.0688265171665768));
#22983=CARTESIAN_POINT('Ctrl Pts',(96.1658607941909,-1.14031872668004,-0.0684457087685313));
#22984=CARTESIAN_POINT('Ctrl Pts',(96.1818979644173,-1.14437914330862,-0.0673507041001178));
#22985=CARTESIAN_POINT('Ctrl Pts',(96.1924220619256,-1.14688994837368,-0.066641419878612));
#22986=CARTESIAN_POINT('Ctrl Pts',(96.2297049004991,-1.15524351249402,-0.0641566012865987));
#22987=CARTESIAN_POINT('Ctrl Pts',(96.256632697569,-1.1602979120863,-0.0624122995080675));
#22988=CARTESIAN_POINT('Ctrl Pts',(96.3636616471749,-1.17654580478821,-0.0555926116133099));
#22989=CARTESIAN_POINT('Ctrl Pts',(96.4446463678075,-1.18041678584323,-0.0506659079224153));
#22990=CARTESIAN_POINT('Ctrl Pts',(96.5646673606718,-1.17379198969531,-0.0430543066728464));
#22991=CARTESIAN_POINT('Ctrl Pts',(96.6038074886636,-1.16965784180789,-0.0405254741412704));
#22992=CARTESIAN_POINT('Ctrl Pts',(96.6529971820366,-1.16195608316122,-0.0372489460046783));
#22993=CARTESIAN_POINT('Ctrl Pts',(96.6633073347592,-1.16020079517852,-0.0365567300417322));
#22994=CARTESIAN_POINT('Ctrl Pts',(96.679688055867,-1.15718698609715,-0.0354475859696136));
#22995=CARTESIAN_POINT('Ctrl Pts',(96.6857745806643,-1.15601741059374,-0.035033398705134));
#22996=CARTESIAN_POINT('Ctrl Pts',(96.6967267677052,-1.15382307929414,-0.0342842442105372));
#22997=CARTESIAN_POINT('Ctrl Pts',(96.7015957413507,-1.15281544091163,-0.0339498150351981));
#22998=CARTESIAN_POINT('Ctrl Pts',(96.7130428970855,-1.15037074978377,-0.0331602278284289));
#22999=CARTESIAN_POINT('Ctrl Pts',(96.7196153678732,-1.14890806826841,-0.0327042818610877));
#23000=CARTESIAN_POINT('Ctrl Pts',(96.7388299251554,-1.14445867098202,-0.0313634986172859));
#23001=CARTESIAN_POINT('Ctrl Pts',(96.7514352267475,-1.14131914346809,-0.0304739265301974));
#23002=CARTESIAN_POINT('Ctrl Pts',(96.8282399042547,-1.12083482611298,-0.0249902212920711));
#23003=CARTESIAN_POINT('Ctrl Pts',(96.8909165022146,-1.09828954316116,-0.0202318454842622));
#23004=CARTESIAN_POINT('Ctrl Pts',(97.0152059874345,-1.04130225887301,-0.0102566782470006));
#23005=CARTESIAN_POINT('Ctrl Pts',(97.0763067357945,-1.00637268554291,-0.00504969948552843));
#23006=CARTESIAN_POINT('Ctrl Pts',(97.1339231275304,-0.966214621837945,
-5.34765442106351E-14));
#23007=CARTESIAN_POINT('',(95.7758165250375,-0.958295198918397,1.18465120291105E-14));
#23008=CARTESIAN_POINT('Origin',(96.460480949577,-8.32667268468867E-16,
1.18130019239114E-14));
#23009=CARTESIAN_POINT('Ctrl Pts',(95.7758165250375,-0.958295198918382,
1.23234755733392E-14));
#23010=CARTESIAN_POINT('Ctrl Pts',(95.7361773941706,-0.929974590868919,
-0.00329165982696945));
#23011=CARTESIAN_POINT('Ctrl Pts',(95.698263491806,-0.899166066562328,-0.0065833196539512));
#23012=CARTESIAN_POINT('Ctrl Pts',(95.6623872069498,-0.866107060633552,
-0.00987497948093297));
#23013=CARTESIAN_POINT('Ctrl Pts',(95.6269881901253,-0.833487844018334,
-0.0131228498237755));
#23014=CARTESIAN_POINT('Ctrl Pts',(95.5935732745532,-0.798678049076778,
-0.016370720166618));
#23015=CARTESIAN_POINT('Ctrl Pts',(95.5624087893347,-0.761945836328084,
-0.0196185905094606));
#23016=CARTESIAN_POINT('Ctrl Pts',(95.5312515903722,-0.725222211569948,
-0.0228657015002861));
#23017=CARTESIAN_POINT('Ctrl Pts',(95.50234411452,-0.686577458385615,-0.0261128124911119));
#23018=CARTESIAN_POINT('Ctrl Pts',(95.4759133383833,-0.646313918686786,
-0.0293599234819374));
#23019=CARTESIAN_POINT('Ctrl Pts',(95.4494795040222,-0.606045720216871,
-0.0326074101860486));
#23020=CARTESIAN_POINT('Ctrl Pts',(95.425523222863,-0.564158800022298,-0.0358548968901596));
#23021=CARTESIAN_POINT('Ctrl Pts',(95.4042276697578,-0.52098375346178,-0.0391023835942709));
#23022=CARTESIAN_POINT('Ctrl Pts',(95.3824252116664,-0.476780997206698,
-0.0424271712820442));
#23023=CARTESIAN_POINT('Ctrl Pts',(95.3634120793787,-0.431228492082274,
-0.0457519589698178));
#23024=CARTESIAN_POINT('Ctrl Pts',(95.3473332165921,-0.384704025259145,
-0.0490767466575911));
#23025=CARTESIAN_POINT('Ctrl Pts',(95.3315957313724,-0.33916734031433,-0.0523309442827269));
#23026=CARTESIAN_POINT('Ctrl Pts',(95.3186691853137,-0.292700104231772,
-0.0555851419078624));
#23027=CARTESIAN_POINT('Ctrl Pts',(95.3086384940891,-0.245670552235394,
-0.0588393395329982));
#23028=CARTESIAN_POINT('Ctrl Pts',(95.2982814241977,-0.197110752508088,
-0.0621994222520902));
#23029=CARTESIAN_POINT('Ctrl Pts',(95.2910120737039,-0.147951994733136,
-0.0655595049711821));
#23030=CARTESIAN_POINT('Ctrl Pts',(95.286866085045,-0.0986063499450008,
-0.0689195876902741));
#23031=CARTESIAN_POINT('Ctrl Pts',(95.2827200963861,-0.0492607051568646,
-0.0722796704093661));
#23032=CARTESIAN_POINT('Ctrl Pts',(95.281697415506,0.000271221556261803,
-0.0756397531284582));
#23033=CARTESIAN_POINT('Ctrl Pts',(95.2837749850334,0.04957958760985,-0.0789998358475502));
#23034=CARTESIAN_POINT('Ctrl Pts',(95.2858102480679,0.0978838649868566,
-0.082291495674532));
#23035=CARTESIAN_POINT('Ctrl Pts',(95.2908306717257,0.146196916652632,-0.0855831555015136));
#23036=CARTESIAN_POINT('Ctrl Pts',(95.2988379439023,0.194114888318772,-0.0888748153284954));
#23037=CARTESIAN_POINT('Ctrl Pts',(95.3064816880046,0.239857396533906,-0.0920170346554361));
#23038=CARTESIAN_POINT('Ctrl Pts',(95.3168468319963,0.285239281260163,-0.0951592539823768));
#23039=CARTESIAN_POINT('Ctrl Pts',(95.3298817822784,0.329909965602386,-0.0983014733093175));
#23040=CARTESIAN_POINT('Ctrl Pts',(95.3429020065228,0.37453018391514,-0.101440142761536));
#23041=CARTESIAN_POINT('Ctrl Pts',(95.3585859147225,0.418440247031338,-0.104578812213755));
#23042=CARTESIAN_POINT('Ctrl Pts',(95.376830955067,0.461300067091394,-0.107717481665974));
#23043=CARTESIAN_POINT('Ctrl Pts',(95.3950638069178,0.504131254896376,-0.110854054348206));
#23044=CARTESIAN_POINT('Ctrl Pts',(95.4158541826417,0.545913065207913,-0.113990627030438));
#23045=CARTESIAN_POINT('Ctrl Pts',(95.4390507459098,0.586323632080711,-0.11712719971267));
#23046=CARTESIAN_POINT('Ctrl Pts',(95.4622425210494,0.62672585758928,-0.120263124957927));
#23047=CARTESIAN_POINT('Ctrl Pts',(95.4878392142814,0.665756908007129,-0.123399050203184));
#23048=CARTESIAN_POINT('Ctrl Pts',(95.5156440752432,0.703120433069016,-0.126534975448441));
#23049=CARTESIAN_POINT('Ctrl Pts',(95.5434755084833,0.740519665339904,-0.129673897604133));
#23050=CARTESIAN_POINT('Ctrl Pts',(95.5735189791043,0.776247735140941,-0.132812819759825));
#23051=CARTESIAN_POINT('Ctrl Pts',(95.6055362907784,0.810039932899456,-0.135951741915517));
#23052=CARTESIAN_POINT('Ctrl Pts',(95.6375716526691,0.843851181491955,-0.139092433683393));
#23053=CARTESIAN_POINT('Ctrl Pts',(95.6715826527233,0.875723998278705,-0.142233125451269));
#23054=CARTESIAN_POINT('Ctrl Pts',(95.707295670523,0.90543193996919,-0.145373817219145));
#23055=CARTESIAN_POINT('Ctrl Pts',(95.74307434671,0.935194499713862,-0.148520283149194));
#23056=CARTESIAN_POINT('Ctrl Pts',(95.7805608209667,0.962783912497935,-0.151666749079243));
#23057=CARTESIAN_POINT('Ctrl Pts',(95.8194516823276,0.988016467995215,-0.154813215009293));
#23058=CARTESIAN_POINT('Ctrl Pts',(95.8325800669933,0.996534219545908,-0.155875367237899));
#23059=CARTESIAN_POINT('Ctrl Pts',(95.8458682817941,1.0047837881853,-0.156937519466506));
#23060=CARTESIAN_POINT('Ctrl Pts',(95.8593040846046,1.01275931964212,-0.157999671695113));
#23061=CARTESIAN_POINT('Ctrl Pts',(95.8797588359455,1.02490131927261,-0.15961669897876));
#23062=CARTESIAN_POINT('Ctrl Pts',(95.9006043517095,1.03643689984567,-0.161233726262408));
#23063=CARTESIAN_POINT('Ctrl Pts',(95.9218016730721,1.04733934308042,-0.162850753546055));
#23064=CARTESIAN_POINT('Origin',(96.460480949577,-7.19464945638997E-16,
0.924367114736168));
#23065=CARTESIAN_POINT('',(95.921801662562,1.04733933767479,-0.761747732816349));
#23066=CARTESIAN_POINT('',(95.9218016734189,1.04733934325879,-0.661999947661212));
#23067=CARTESIAN_POINT('',(95.9218016730721,1.04733934308042,0.924367114736168));
#23068=CARTESIAN_POINT('Ctrl Pts',(95.921801662562,1.04733933767479,-0.761747732816352));
#23069=CARTESIAN_POINT('Ctrl Pts',(95.883175508933,1.02747270214554,-0.759053178224855));
#23070=CARTESIAN_POINT('Ctrl Pts',(95.8456739353038,1.0054824021569,-0.756338917671403));
#23071=CARTESIAN_POINT('Ctrl Pts',(95.7930101764126,0.97055032306898,-0.752300385322997));
#23072=CARTESIAN_POINT('Ctrl Pts',(95.7768288777527,0.959221007440542,-0.751026396207034));
#23073=CARTESIAN_POINT('Ctrl Pts',(95.7489791754977,0.938659341417836,-0.748768147748057));
#23074=CARTESIAN_POINT('Ctrl Pts',(95.7371863806177,0.929602639869777,-0.747790326834797));
#23075=CARTESIAN_POINT('Ctrl Pts',(95.7200663091019,0.915931658638611,-0.746336714737209));
#23076=CARTESIAN_POINT('Ctrl Pts',(95.7146036249844,0.911488703265523,-0.745867635471517));
#23077=CARTESIAN_POINT('Ctrl Pts',(95.7049759903812,0.90351377223756,-0.745031317294701));
#23078=CARTESIAN_POINT('Ctrl Pts',(95.7007951117538,0.900001281160456,-0.744664865071834));
#23079=CARTESIAN_POINT('Ctrl Pts',(95.6920493365921,0.892549312429411,-0.743891280900056));
#23080=CARTESIAN_POINT('Ctrl Pts',(95.6874899774325,0.888603608818043,-0.743483902360617));
#23081=CARTESIAN_POINT('Ctrl Pts',(95.6754943726046,0.878060339647571,-0.742401051401197));
#23082=CARTESIAN_POINT('Ctrl Pts',(95.668111152382,0.871403454248285,-0.741723149027886));
#23083=CARTESIAN_POINT('Ctrl Pts',(95.6356286319705,0.841362282641241,-0.738688566017347));
#23084=CARTESIAN_POINT('Ctrl Pts',(95.6114760782899,0.816983569241954,-0.736290333530637));
#23085=CARTESIAN_POINT('Ctrl Pts',(95.5209915352847,0.71730074211193,-0.726720246965365));
#23086=CARTESIAN_POINT('Ctrl Pts',(95.4633315461491,0.634704031424583,-0.719240177441031));
#23087=CARTESIAN_POINT('Ctrl Pts',(95.4068753061827,0.526757118265861,-0.710431220858489));
#23088=CARTESIAN_POINT('Ctrl Pts',(95.3974283974248,0.507422207953915,-0.708889581995119));
#23089=CARTESIAN_POINT('Ctrl Pts',(95.3829184905314,0.475538458686883,-0.70641694709215));
#23090=CARTESIAN_POINT('Ctrl Pts',(95.377532812947,0.463142581971482,-0.705472286298644));
#23091=CARTESIAN_POINT('Ctrl Pts',(95.370538095951,0.446253676992116,-0.704210150104191));
#23092=CARTESIAN_POINT('Ctrl Pts',(95.3687414767789,0.441840122548483,-0.703882593050572));
#23093=CARTESIAN_POINT('Ctrl Pts',(95.3657886165976,0.434458174171859,-0.703338663209367));
#23094=CARTESIAN_POINT('Ctrl Pts',(95.3646175597465,0.431495817522591,-0.703121435561114));
#23095=CARTESIAN_POINT('Ctrl Pts',(95.3624229651439,0.425877711778397,-0.702711497325987));
#23096=CARTESIAN_POINT('Ctrl Pts',(95.3613970137209,0.423222949458762,-0.702518641099976));
#23097=CARTESIAN_POINT('Ctrl Pts',(95.3589899062457,0.41692650779497,-0.702063196056052));
#23098=CARTESIAN_POINT('Ctrl Pts',(95.3576171602591,0.413281616724026,-0.70180109689761));
#23099=CARTESIAN_POINT('Ctrl Pts',(95.3528520751442,0.400436620127926,-0.700882645218786));
#23100=CARTESIAN_POINT('Ctrl Pts',(95.3495564599009,0.391200720625591,-0.700231631579146));
#23101=CARTESIAN_POINT('Ctrl Pts',(95.3235020744241,0.315197956433535,-0.694942528266368));
#23102=CARTESIAN_POINT('Ctrl Pts',(95.3066652524538,0.246541720849499,-0.690587662731763));
#23103=CARTESIAN_POINT('Ctrl Pts',(95.2871758999191,0.11817243775893,-0.682556262573215));
#23104=CARTESIAN_POINT('Ctrl Pts',(95.2827159202301,0.0589774671510073,
-0.678893948014252));
#23105=CARTESIAN_POINT('Ctrl Pts',(95.2827364028008,-0.0216032836315505,
-0.67375862036588));
#23106=CARTESIAN_POINT('Ctrl Pts',(95.2833198525272,-0.0429020934960637,
-0.672387663883698));
#23107=CARTESIAN_POINT('Ctrl Pts',(95.2853392862911,-0.0799094805642896,
-0.669973549186979));
#23108=CARTESIAN_POINT('Ctrl Pts',(95.2865137929773,-0.095627040862744,
-0.668938174233592));
#23109=CARTESIAN_POINT('Ctrl Pts',(95.288684274623,-0.118488513312446,-0.667415339378116));
#23110=CARTESIAN_POINT('Ctrl Pts',(95.2894310573696,-0.125654770400463,
-0.666935566827369));
#23111=CARTESIAN_POINT('Ctrl Pts',(95.2908617015114,-0.138260357386943,
-0.666087172534181));
#23112=CARTESIAN_POINT('Ctrl Pts',(95.2915178809062,-0.143702659064925,
-0.665719420049251));
#23113=CARTESIAN_POINT('Ctrl Pts',(95.2929653561576,-0.155041261594513,
-0.664950079167147));
#23114=CARTESIAN_POINT('Ctrl Pts',(95.2937633811791,-0.160936531053128,
-0.664548291101586));
#23115=CARTESIAN_POINT('Ctrl Pts',(95.2959621700797,-0.176302972258673,
-0.663496211740579));
#23116=CARTESIAN_POINT('Ctrl Pts',(95.2974337976727,-0.185763394915532,
-0.6628437313546));
#23117=CARTESIAN_POINT('Ctrl Pts',(95.3041297854199,-0.225604284995654,
-0.660075124693852));
#23118=CARTESIAN_POINT('Ctrl Pts',(95.3104300855992,-0.255789007360232,
-0.657925883700481));
#23119=CARTESIAN_POINT('Ctrl Pts',(95.3380853240114,-0.366392145815569,
-0.649853020082257));
#23120=CARTESIAN_POINT('Ctrl Pts',(95.3667558691237,-0.444721502703924,
-0.643721683528358));
#23121=CARTESIAN_POINT('Ctrl Pts',(95.4264488532246,-0.566213086230039,
-0.633812571898049));
#23122=CARTESIAN_POINT('Ctrl Pts',(95.4525588129756,-0.611484998968461,
-0.630025482866978));
#23123=CARTESIAN_POINT('Ctrl Pts',(95.4854589832101,-0.660663036865783,
-0.625910146231612));
#23124=CARTESIAN_POINT('Ctrl Pts',(95.4893795043116,-0.666412388866609,
-0.625429045201617));
#23125=CARTESIAN_POINT('Ctrl Pts',(95.4954404839801,-0.675133593744484,
-0.624699693948617));
#23126=CARTESIAN_POINT('Ctrl Pts',(95.497544145083,-0.678130651946481,-0.624449129982574));
#23127=CARTESIAN_POINT('Ctrl Pts',(95.5014210988507,-0.6835996778996,-0.623992117964115));
#23128=CARTESIAN_POINT('Ctrl Pts',(95.5031899977151,-0.686074595673858,
-0.623785393930058));
#23129=CARTESIAN_POINT('Ctrl Pts',(95.5072052740297,-0.691646721034061,
-0.623320150460493));
#23130=CARTESIAN_POINT('Ctrl Pts',(95.5094571667806,-0.694739854835062,
-0.623062009242804));
#23131=CARTESIAN_POINT('Ctrl Pts',(95.5153166979157,-0.702706456626337,
-0.622397299369914));
#23132=CARTESIAN_POINT('Ctrl Pts',(95.5189470229731,-0.707563209667553,
-0.621992214828497));
#23133=CARTESIAN_POINT('Ctrl Pts',(95.5435737488713,-0.739984374202579,
-0.619287460584144));
#23134=CARTESIAN_POINT('Ctrl Pts',(95.5657424625328,-0.766641529032463,
-0.617060368082938));
#23135=CARTESIAN_POINT('Ctrl Pts',(95.608028899734,-0.813151857328128,-0.613088443996411));
#23136=CARTESIAN_POINT('Ctrl Pts',(95.6277451311158,-0.833331637360445,
-0.611332377661967));
#23137=CARTESIAN_POINT('Ctrl Pts',(95.6828814034993,-0.885851259702204,
-0.606611168969166));
#23138=CARTESIAN_POINT('Ctrl Pts',(95.7195813084104,-0.916766675901992,
-0.603662983051974));
#23139=CARTESIAN_POINT('Ctrl Pts',(95.8009142147579,-0.977198428823439,
-0.59732679130867));
#23140=CARTESIAN_POINT('Ctrl Pts',(95.8458756378212,-1.00608363014918,-0.593933277407727));
#23141=CARTESIAN_POINT('Ctrl Pts',(95.9021298814729,-1.03704221295016,-0.589713131939763));
#23142=CARTESIAN_POINT('Ctrl Pts',(95.9116939988176,-1.04213498961617,-0.588996647613429));
#23143=CARTESIAN_POINT('Ctrl Pts',(95.9268602191834,-1.04994414881689,-0.587861367674102));
#23144=CARTESIAN_POINT('Ctrl Pts',(95.9324160781207,-1.05274939494953,-0.587445663834514));
#23145=CARTESIAN_POINT('Ctrl Pts',(95.9428592077469,-1.05791883776531,-0.586664493736362));
#23146=CARTESIAN_POINT('Ctrl Pts',(95.947741116453,-1.06029354272856,-0.586299401733016));
#23147=CARTESIAN_POINT('Ctrl Pts',(95.9587072892667,-1.06553436733621,-0.585479400461564));
#23148=CARTESIAN_POINT('Ctrl Pts',(95.9647999963751,-1.06838227406905,-0.585023883402262));
#23149=CARTESIAN_POINT('Ctrl Pts',(95.9803651615633,-1.07549607833121,-0.583860170693215));
#23150=CARTESIAN_POINT('Ctrl Pts',(95.9898701192688,-1.07968903801979,-0.58314954489004));
#23151=CARTESIAN_POINT('Ctrl Pts',(96.0688174940618,-1.11327487395352,-0.577245684955331));
#23152=CARTESIAN_POINT('Ctrl Pts',(96.1408675037319,-1.13605659196619,-0.57183118287821));
#23153=CARTESIAN_POINT('Ctrl Pts',(96.271027585386,-1.1638441470624,-0.562095418288413));
#23154=CARTESIAN_POINT('Ctrl Pts',(96.3282780046136,-1.17172880972086,-0.55783301952061));
#23155=CARTESIAN_POINT('Ctrl Pts',(96.4064210712549,-1.17668873084238,-0.552178135924882));
#23156=CARTESIAN_POINT('Ctrl Pts',(96.4269975000278,-1.17745394775479,-0.550704859581647));
#23157=CARTESIAN_POINT('Ctrl Pts',(96.460676718844,-1.17782275800697,-0.548329315087066));
#23158=CARTESIAN_POINT('Ctrl Pts',(96.4737710499031,-1.17774780684484,-0.54741459827547));
#23159=CARTESIAN_POINT('Ctrl Pts',(96.4915692344859,-1.17734903472878,-0.546185715716059));
#23160=CARTESIAN_POINT('Ctrl Pts',(96.4962758268873,-1.17721534125518,-0.545862120274871));
#23161=CARTESIAN_POINT('Ctrl Pts',(96.5041535940924,-1.17694427911458,-0.545322932476015));
#23162=CARTESIAN_POINT('Ctrl Pts',(96.5073252042244,-1.17682231140232,-0.54510651590472));
#23163=CARTESIAN_POINT('Ctrl Pts',(96.5133515988379,-1.1765661579976,-0.544696607346896));
#23164=CARTESIAN_POINT('Ctrl Pts',(96.5162064393188,-1.17643440103334,-0.544502979149504));
#23165=CARTESIAN_POINT('Ctrl Pts',(96.5229931550246,-1.17609641966686,-0.544043932661879));
#23166=CARTESIAN_POINT('Ctrl Pts',(96.5269245626726,-1.17588086622953,-0.543779021649199));
#23167=CARTESIAN_POINT('Ctrl Pts',(96.5408393247403,-1.17504793105682,-0.542844725833134));
#23168=CARTESIAN_POINT('Ctrl Pts',(96.5508161520526,-1.17432307146511,-0.54218090365708));
#23169=CARTESIAN_POINT('Ctrl Pts',(96.6236928733034,-1.16809396251231,-0.537368405130885));
#23170=CARTESIAN_POINT('Ctrl Pts',(96.6860772599701,-1.15766577448211,-0.533444365229694));
#23171=CARTESIAN_POINT('Ctrl Pts',(96.8076751106828,-1.12713010411461,-0.525681964414421));
#23172=CARTESIAN_POINT('Ctrl Pts',(96.8667198121304,-1.10721971269949,-0.521853641267478));
#23173=CARTESIAN_POINT('Ctrl Pts',(96.9565764886802,-1.06875935943932,-0.515647447785411));
#23174=CARTESIAN_POINT('Ctrl Pts',(96.9885869091643,-1.05330957811765,-0.513356456117118));
#23175=CARTESIAN_POINT('Ctrl Pts',(97.0283783520863,-1.03183407812645,-0.510377300056813));
#23176=CARTESIAN_POINT('Ctrl Pts',(97.0368513147062,-1.02712521999043,-0.509735128418848));
#23177=CARTESIAN_POINT('Ctrl Pts',(97.0504529069733,-1.01934482544907,-0.508691053061727));
#23178=CARTESIAN_POINT('Ctrl Pts',(97.0556180818328,-1.0163378253653,-0.508291442175202));
#23179=CARTESIAN_POINT('Ctrl Pts',(97.065471845453,-1.01050040599915,-0.507522959230861));
#23180=CARTESIAN_POINT('Ctrl Pts',(97.0701640286481,-1.00767633492837,-0.507154322362964));
#23181=CARTESIAN_POINT('Ctrl Pts',(97.0808373589423,-1.00115056970297,-0.506309497127684));
#23182=CARTESIAN_POINT('Ctrl Pts',(97.0868053344931,-0.997427841502103,
-0.505832555579537));
#23183=CARTESIAN_POINT('Ctrl Pts',(97.1055903858657,-0.985474954680329,
-0.504316573511841));
#23184=CARTESIAN_POINT('Ctrl Pts',(97.1182808876775,-0.97704978117323,-0.503270445204628));
#23185=CARTESIAN_POINT('Ctrl Pts',(97.2014241411096,-0.919497204083365,
-0.496265631504845));
#23186=CARTESIAN_POINT('Ctrl Pts',(97.2664725388368,-0.863043601592718,
-0.490024242795726));
#23187=CARTESIAN_POINT('Ctrl Pts',(97.3584923083937,-0.763630432497412,
-0.480082845415622));
#23188=CARTESIAN_POINT('Ctrl Pts',(97.3898574909068,-0.725131442667534,
-0.47643880324814));
#23189=CARTESIAN_POINT('Ctrl Pts',(97.4277539183399,-0.672101492416839,
-0.471769616429379));
#23190=CARTESIAN_POINT('Ctrl Pts',(97.4365536782622,-0.65925677080646,-0.47066392381815));
#23191=CARTESIAN_POINT('Ctrl Pts',(97.450947588531,-0.637326135923955,-0.468822744339366));
#23192=CARTESIAN_POINT('Ctrl Pts',(97.4566774954469,-0.628332100348734,
-0.46808047217702));
#23193=CARTESIAN_POINT('Ctrl Pts',(97.4645698119503,-0.615564380396892,
-0.467045970709026));
#23194=CARTESIAN_POINT('Ctrl Pts',(97.4668344900243,-0.611854968997145,
-0.466747664461544));
#23195=CARTESIAN_POINT('Ctrl Pts',(97.4706813912681,-0.605474826087057,
-0.466238533587721));
#23196=CARTESIAN_POINT('Ctrl Pts',(97.4722736713353,-0.602810240900197,
-0.466027075008146));
#23197=CARTESIAN_POINT('Ctrl Pts',(97.4753524003984,-0.597611605487717,
-0.465616834140029));
#23198=CARTESIAN_POINT('Ctrl Pts',(97.4768399161787,-0.595078267283493,
-0.465417978232927));
#23199=CARTESIAN_POINT('Ctrl Pts',(97.4808977304109,-0.588107939547102,
-0.464873660669491));
#23200=CARTESIAN_POINT('Ctrl Pts',(97.4834485942745,-0.583659622955238,
-0.464529413745853));
#23201=CARTESIAN_POINT('Ctrl Pts',(97.4933650466222,-0.566102111953248,
-0.463182338794736));
#23202=CARTESIAN_POINT('Ctrl Pts',(97.5005087257035,-0.552868370947933,
-0.462192414695996));
#23203=CARTESIAN_POINT('Ctrl Pts',(97.5191780650158,-0.51663998773245,-0.459540628846992));
#23204=CARTESIAN_POINT('Ctrl Pts',(97.5302075893586,-0.49339796471292,-0.45790152035355));
#23205=CARTESIAN_POINT('Ctrl Pts',(97.5613029659211,-0.421917026002823,
-0.45299158517889));
#23206=CARTESIAN_POINT('Ctrl Pts',(97.5789297272181,-0.372687343470029,
-0.449783838693494));
#23207=CARTESIAN_POINT('Ctrl Pts',(97.6131931189828,-0.252321296073137,
-0.442031229795563));
#23208=CARTESIAN_POINT('Ctrl Pts',(97.6265977460064,-0.180501841042826,
-0.437469067927289));
#23209=CARTESIAN_POINT('Ctrl Pts',(97.6342318086101,-0.0975324642251496,
-0.432001344547463));
#23210=CARTESIAN_POINT('Ctrl Pts',(97.6350488238433,-0.0871433192819611,
-0.431313480616302));
#23211=CARTESIAN_POINT('Ctrl Pts',(97.6361665474715,-0.0700268708716457,
-0.430174254414681));
#23212=CARTESIAN_POINT('Ctrl Pts',(97.6365476265763,-0.0633052591097759,
-0.429725375911245));
#23213=CARTESIAN_POINT('Ctrl Pts',(97.6371316861353,-0.0511618978609094,
-0.428911541953791));
#23214=CARTESIAN_POINT('Ctrl Pts',(97.6373548722398,-0.0457412735787324,
-0.428547221717702));
#23215=CARTESIAN_POINT('Ctrl Pts',(97.6377531758196,-0.0341134384786835,
-0.42776340314737));
#23216=CARTESIAN_POINT('Ctrl Pts',(97.6379166687722,-0.0279060204894306,
-0.42734355645944));
#23217=CARTESIAN_POINT('Ctrl Pts',(97.6382297343926,-0.0109157201833946,
-0.426190385203877));
#23218=CARTESIAN_POINT('Ctrl Pts',(97.6382803052739,-0.000131842598366711,
-0.425454034069181));
#23219=CARTESIAN_POINT('Ctrl Pts',(97.6377087775588,0.0630636529869075,
-0.421111713507778));
#23220=CARTESIAN_POINT('Ctrl Pts',(97.633736564964,0.115378690850311,-0.417403533785645));
#23221=CARTESIAN_POINT('Ctrl Pts',(97.6152083901342,0.244529779270065,-0.407979584444264));
#23222=CARTESIAN_POINT('Ctrl Pts',(97.5964659729673,0.320510900434516,-0.402183935243037));
#23223=CARTESIAN_POINT('Ctrl Pts',(97.5590097426722,0.426001490579876,-0.394072370120888));
#23224=CARTESIAN_POINT('Ctrl Pts',(97.5463007056735,0.457426174424071,-0.391650022603342));
#23225=CARTESIAN_POINT('Ctrl Pts',(97.5297533990795,0.493748766075535,-0.388875976599983));
#23226=CARTESIAN_POINT('Ctrl Pts',(97.5272116481038,0.499216421901405,-0.388459118458316));
#23227=CARTESIAN_POINT('Ctrl Pts',(97.5229935109954,0.508110882160203,-0.387782459316815));
#23228=CARTESIAN_POINT('Ctrl Pts',(97.5213423057645,0.511549406920673,-0.387521227998317));
#23229=CARTESIAN_POINT('Ctrl Pts',(97.518344871286,0.517714429857221,-0.387053586461117));
#23230=CARTESIAN_POINT('Ctrl Pts',(97.5170047687458,0.520443779750109,-0.386846818113173));
#23231=CARTESIAN_POINT('Ctrl Pts',(97.5140241850062,0.526455293733115,-0.386391983380981));
#23232=CARTESIAN_POINT('Ctrl Pts',(97.5123789288335,0.529734997306368,-0.386144213239588));
#23233=CARTESIAN_POINT('Ctrl Pts',(97.5075527880926,0.539244428409664,-0.385426743344741));
#23234=CARTESIAN_POINT('Ctrl Pts',(97.504331633202,0.545453705407088,-0.384959435322203));
#23235=CARTESIAN_POINT('Ctrl Pts',(97.4756384149433,0.599579122224819,-0.38089302884618));
#23236=CARTESIAN_POINT('Ctrl Pts',(97.4469346321389,0.645717081971682,-0.37747399607917));
#23237=CARTESIAN_POINT('Ctrl Pts',(97.3632655202171,0.761527161251995,-0.368584937962893));
#23238=CARTESIAN_POINT('Ctrl Pts',(97.30345136125,0.827250687989441,-0.363193827150058));
#23239=CARTESIAN_POINT('Ctrl Pts',(97.2181118995332,0.902058947730075,-0.355903010213178));
#23240=CARTESIAN_POINT('Ctrl Pts',(97.1988740497568,0.917872807074346,-0.354283610705932));
#23241=CARTESIAN_POINT('Ctrl Pts',(97.1721265760849,0.938474384311253,-0.352054838550277));
#23242=CARTESIAN_POINT('Ctrl Pts',(97.1650418792318,0.943804829953751,-0.351466595056858));
#23243=CARTESIAN_POINT('Ctrl Pts',(97.1536924764191,0.952144987217313,-0.35052719461897));
#23244=CARTESIAN_POINT('Ctrl Pts',(97.1494666842747,0.955207283017022,-0.350178059111182));
#23245=CARTESIAN_POINT('Ctrl Pts',(97.1407573313736,0.96143080952085,-0.349459709170628));
#23246=CARTESIAN_POINT('Ctrl Pts',(97.1362717628489,0.964588996452458,-0.34909039116953));
#23247=CARTESIAN_POINT('Ctrl Pts',(97.125834319578,0.971829224757706,-0.348232436638685));
#23248=CARTESIAN_POINT('Ctrl Pts',(97.1198667125322,0.975888088187573,-0.34774294896745));
#23249=CARTESIAN_POINT('Ctrl Pts',(97.1007044791588,0.988665260234743,-0.346174257112538));
#23250=CARTESIAN_POINT('Ctrl Pts',(97.0873718739467,0.997172448222111,-0.345087369360005));
#23251=CARTESIAN_POINT('Ctrl Pts',(97.0556054106112,1.01655291574387,-0.342507111447704));
#23252=CARTESIAN_POINT('Ctrl Pts',(97.0370389756335,1.02719701058837,-0.341006191423924));
#23253=CARTESIAN_POINT('Ctrl Pts',(96.9655640134995,1.06562504371581,-0.335254427332842));
#23254=CARTESIAN_POINT('Ctrl Pts',(96.9108625239515,1.08987184139744,-0.330899911259941));
#23255=CARTESIAN_POINT('Ctrl Pts',(96.788836999403,1.13319992221958,-0.321400919226787));
#23256=CARTESIAN_POINT('Ctrl Pts',(96.7211609044422,1.15065524141902,-0.31626326058391));
#23257=CARTESIAN_POINT('Ctrl Pts',(96.6426352963192,1.1636199803381,-0.310684842131048));
#23258=CARTESIAN_POINT('Ctrl Pts',(96.6329178744116,1.16509964694966,-0.310001245297676));
#23259=CARTESIAN_POINT('Ctrl Pts',(96.619309486215,1.16699779432538,-0.309054338598213));
#23260=CARTESIAN_POINT('Ctrl Pts',(96.6154335545219,1.16751875673237,-0.308785818224782));
#23261=CARTESIAN_POINT('Ctrl Pts',(96.6087256575918,1.16838636945384,-0.308323218540102));
#23262=CARTESIAN_POINT('Ctrl Pts',(96.6058949249572,1.16874204937883,-0.308128652193352));
#23263=CARTESIAN_POINT('Ctrl Pts',(96.5998920975165,1.16947415439466,-0.307717474527367));
#23264=CARTESIAN_POINT('Ctrl Pts',(96.5967196987903,1.16984796866048,-0.307501012233984));
#23265=CARTESIAN_POINT('Ctrl Pts',(96.5888061242937,1.17074782372535,-0.306963047038128));
#23266=CARTESIAN_POINT('Ctrl Pts',(96.5840631449785,1.17125798189131,-0.306642408530999));
#23267=CARTESIAN_POINT('Ctrl Pts',(96.565910797779,1.17309896730375,-0.305421649475919));
#23268=CARTESIAN_POINT('Ctrl Pts',(96.5524814479601,1.1742285068074,-0.304531835572617));
#23269=CARTESIAN_POINT('Ctrl Pts',(96.5176686038893,1.1765556496786,-0.30225276191564));
#23270=CARTESIAN_POINT('Ctrl Pts',(96.4962659261763,1.17740102382463,-0.300878449029231));
#23271=CARTESIAN_POINT('Ctrl Pts',(96.3757729610454,1.17887128754924,-0.293233736932032));
#23272=CARTESIAN_POINT('Ctrl Pts',(96.2769370490261,1.1675729618675,-0.287280365906995));
#23273=CARTESIAN_POINT('Ctrl Pts',(96.1467186906655,1.13572469125749,-0.278766983427975));
#23274=CARTESIAN_POINT('Ctrl Pts',(96.113148245026,1.12591161353944,-0.276513013453992));
#23275=CARTESIAN_POINT('Ctrl Pts',(96.0705880123846,1.11138600820529,-0.273551977230737));
#23276=CARTESIAN_POINT('Ctrl Pts',(96.0611517740671,1.10803048747445,-0.272888829077721));
#23277=CARTESIAN_POINT('Ctrl Pts',(96.0460819976803,1.10245418113594,-0.271818520353859));
#23278=CARTESIAN_POINT('Ctrl Pts',(96.0404206616993,1.10030953148593,-0.27141385828414));
#23279=CARTESIAN_POINT('Ctrl Pts',(96.0296762839738,1.09614429731005,-0.270640833639246));
#23280=CARTESIAN_POINT('Ctrl Pts',(96.0245902780235,1.09413175676287,-0.270272745195363));
#23281=CARTESIAN_POINT('Ctrl Pts',(96.0129948036356,1.08944972795434,-0.269428488257682));
#23282=CARTESIAN_POINT('Ctrl Pts',(96.0064949190696,1.08675721343144,-0.268951564267823));
#23283=CARTESIAN_POINT('Ctrl Pts',(95.9864069298799,1.07822429434095,-0.267465959759572));
#23284=CARTESIAN_POINT('Ctrl Pts',(95.9729048845689,1.07218624849779,-0.266450717872592));
#23285=CARTESIAN_POINT('Ctrl Pts',(95.946837381003,1.05993478354444,-0.26445698429842));
#23286=CARTESIAN_POINT('Ctrl Pts',(95.9342624202848,1.05374829386364,-0.263479547321252));
#23287=CARTESIAN_POINT('Ctrl Pts',(95.9218016724468,1.04733934275882,-0.262495071028825));
#23288=CARTESIAN_POINT('',(97.6382306586311,0.000827842401244189,-0.325632885263827));
#23289=CARTESIAN_POINT('Ctrl Pts',(95.9218016730721,1.04733934308042,-0.162850753546055));
#23290=CARTESIAN_POINT('Ctrl Pts',(95.963457953322,1.06876446670931,-0.16602848249336));
#23291=CARTESIAN_POINT('Ctrl Pts',(96.0064744835986,1.08774169819866,-0.169206211440665));
#23292=CARTESIAN_POINT('Ctrl Pts',(96.0505334981692,1.10410060664064,-0.172383940387971));
#23293=CARTESIAN_POINT('Ctrl Pts',(96.0945382959645,1.12043938464457,-0.175557758984172));
#23294=CARTESIAN_POINT('Ctrl Pts',(96.139582521453,1.13416602324947,-0.178731577580373));
#23295=CARTESIAN_POINT('Ctrl Pts',(96.1853263829313,1.14515720621843,-0.181905396176574));
#23296=CARTESIAN_POINT('Ctrl Pts',(96.2310339716416,1.15613967368727,-0.185076698081309));
#23297=CARTESIAN_POINT('Ctrl Pts',(96.277439558641,1.1643908508674,-0.188247999986045));
#23298=CARTESIAN_POINT('Ctrl Pts',(96.3241886475632,1.16983736942867,-0.19141930189078));
#23299=CARTESIAN_POINT('Ctrl Pts',(96.3709211218398,1.17528195229497,-0.194589476713496));
#23300=CARTESIAN_POINT('Ctrl Pts',(96.4179963040495,1.17792378871448,-0.197759651536212));
#23301=CARTESIAN_POINT('Ctrl Pts',(96.4650526666343,1.17774112686241,-0.200929826358928));
#23302=CARTESIAN_POINT('Ctrl Pts',(96.5121475638274,1.17755831542797,-0.204102597248113));
#23303=CARTESIAN_POINT('Ctrl Pts',(96.5592230532303,1.17454638285798,-0.207275368137299));
#23304=CARTESIAN_POINT('Ctrl Pts',(96.6059176191503,1.16873574328991,-0.210448139026484));
#23305=CARTESIAN_POINT('Ctrl Pts',(96.6526303191125,1.16292284713414,-0.213622142075341));
#23306=CARTESIAN_POINT('Ctrl Pts',(96.6989612519655,1.15430917475159,-0.216796145124199));
#23307=CARTESIAN_POINT('Ctrl Pts',(96.7445576924114,1.14297658186009,-0.219970148173057));
#23308=CARTESIAN_POINT('Ctrl Pts',(96.7902419709798,1.13162215757844,-0.22315026570071));
#23309=CARTESIAN_POINT('Ctrl Pts',(96.8351883971898,1.11753851314616,-0.226330383228363));
#23310=CARTESIAN_POINT('Ctrl Pts',(96.8790595461831,1.10085740264727,-0.229510500756015));
#23311=CARTESIAN_POINT('Ctrl Pts',(96.9134976164422,1.08776302813135,-0.232006836351569));
#23312=CARTESIAN_POINT('Ctrl Pts',(96.9472733745764,1.07306913453378,-0.234503171947122));
#23313=CARTESIAN_POINT('Ctrl Pts',(96.9802341500302,1.05685934405611,-0.236999507542675));
#23314=CARTESIAN_POINT('Ctrl Pts',(97.0236961190942,1.03548516815837,-0.240291167369657));
#23315=CARTESIAN_POINT('Ctrl Pts',(97.0659334661461,1.01137835486445,-0.243582827196638));
#23316=CARTESIAN_POINT('Ctrl Pts',(97.1065838599168,0.984706094096334,-0.24687448702362));
#23317=CARTESIAN_POINT('Ctrl Pts',(97.1458237609606,0.958959310951739,-0.250051932403593));
#23318=CARTESIAN_POINT('Ctrl Pts',(97.1835845317979,0.930822543258878,-0.253229377783565));
#23319=CARTESIAN_POINT('Ctrl Pts',(97.2195635397929,0.900493577839994,-0.256406823163538));
#23320=CARTESIAN_POINT('Ctrl Pts',(97.2555079630214,0.870193766092844,-0.259581214228987));
#23321=CARTESIAN_POINT('Ctrl Pts',(97.2896735909337,0.837706284579617,-0.262755605294436));
#23322=CARTESIAN_POINT('Ctrl Pts',(97.3217887886277,0.803270732001229,-0.265929996359885));
#23323=CARTESIAN_POINT('Ctrl Pts',(97.353887119405,0.768853264991046,-0.269102720233673));
#23324=CARTESIAN_POINT('Ctrl Pts',(97.3839367753294,0.732490159590648,-0.27227544410746));
#23325=CARTESIAN_POINT('Ctrl Pts',(97.4117030748047,0.694457724398867,-0.275448167981248));
#23326=CARTESIAN_POINT('Ctrl Pts',(97.4394668978288,0.656428681285709,-0.278620608882652));
#23327=CARTESIAN_POINT('Ctrl Pts',(97.4649474433992,0.616731053807496,-0.281793049784056));
#23328=CARTESIAN_POINT('Ctrl Pts',(97.4879520809459,0.575671900220555,-0.28496549068546));
#23329=CARTESIAN_POINT('Ctrl Pts',(97.5109804732496,0.534570348651244,-0.288141207472548));
#23330=CARTESIAN_POINT('Ctrl Pts',(97.5315275861647,0.492104952068775,-0.291316924259635));
#23331=CARTESIAN_POINT('Ctrl Pts',(97.5494466716691,0.448607532937615,-0.294492641046723));
#23332=CARTESIAN_POINT('Ctrl Pts',(97.5673769246852,0.40508300539552,-0.297670337000331));
#23333=CARTESIAN_POINT('Ctrl Pts',(97.5826757106302,0.360525700835335,-0.300848032953939));
#23334=CARTESIAN_POINT('Ctrl Pts',(97.5952456640176,0.315284166047998,-0.304025728907547));
#23335=CARTESIAN_POINT('Ctrl Pts',(97.607838216946,0.269961291426521,-0.307209138046241));
#23336=CARTESIAN_POINT('Ctrl Pts',(97.6176920373088,0.223952275727347,-0.310392547184935));
#23337=CARTESIAN_POINT('Ctrl Pts',(97.6247608897451,0.177615549493993,-0.313575956323629));
#23338=CARTESIAN_POINT('Ctrl Pts',(97.6265546235301,0.16585752341037,-0.314383752012498));
#23339=CARTESIAN_POINT('Ctrl Pts',(97.6281692948468,0.154078412576249,-0.315191547701367));
#23340=CARTESIAN_POINT('Ctrl Pts',(97.6296046814756,0.142284089101716,-0.315999343390236));
#23341=CARTESIAN_POINT('Ctrl Pts',(97.6353106858459,0.095398838854968,-0.319210524014766));
#23342=CARTESIAN_POINT('Ctrl Pts',(97.6381973880941,0.0481609642844836,
-0.322421704639297));
#23343=CARTESIAN_POINT('Ctrl Pts',(97.6382306586311,0.000827842401244189,
-0.325632885263827));
#23344=CARTESIAN_POINT('Ctrl Pts',(97.638230626738,0.00087203623034647,
-0.326333448408234));
#23345=CARTESIAN_POINT('Ctrl Pts',(97.638286653864,-0.0747967573660931,
-0.331106951541581));
#23346=CARTESIAN_POINT('Ctrl Pts',(97.6310503143384,-0.150299827625081,
-0.335701552920094));
#23347=CARTESIAN_POINT('Ctrl Pts',(97.6065752538257,-0.276290640543653,
-0.343727845590335));
#23348=CARTESIAN_POINT('Ctrl Pts',(97.5930771831955,-0.327251259773279,
-0.347076331299543));
#23349=CARTESIAN_POINT('Ctrl Pts',(97.5727718465764,-0.387323797531268,
-0.351243588323239));
#23350=CARTESIAN_POINT('Ctrl Pts',(97.5691881255141,-0.397465909388993,
-0.351954786272469));
#23351=CARTESIAN_POINT('Ctrl Pts',(97.5633268243591,-0.413357298293986,
-0.353081903965348));
#23352=CARTESIAN_POINT('Ctrl Pts',(97.5611419630215,-0.419140323267442,
-0.353494761614325));
#23353=CARTESIAN_POINT('Ctrl Pts',(97.5569658010524,-0.4299361864992,-0.354270671893381));
#23354=CARTESIAN_POINT('Ctrl Pts',(97.5549853879578,-0.434953085601531,
-0.35463335385735));
#23355=CARTESIAN_POINT('Ctrl Pts',(97.5504741686503,-0.446155248917659,
-0.355448012816802));
#23356=CARTESIAN_POINT('Ctrl Pts',(97.5479250526679,-0.452332889820701,
-0.355900594056792));
#23357=CARTESIAN_POINT('Ctrl Pts',(97.54130493958,-0.467996930121249,-0.357056808364033));
#23358=CARTESIAN_POINT('Ctrl Pts',(97.5371616120618,-0.477451948542248,
-0.357762856559819));
#23359=CARTESIAN_POINT('Ctrl Pts',(97.501988241869,-0.554930277674469,-0.363617460740938));
#23360=CARTESIAN_POINT('Ctrl Pts',(97.4646753399647,-0.619899070466905,
-0.368984890550831));
#23361=CARTESIAN_POINT('Ctrl Pts',(97.3887244692412,-0.727094549333626,
-0.378598449683826));
#23362=CARTESIAN_POINT('Ctrl Pts',(97.3526921559772,-0.770883811115552,
-0.382784366829987));
#23363=CARTESIAN_POINT('Ctrl Pts',(97.2983523795545,-0.827984826870115,
-0.388492113375989));
#23364=CARTESIAN_POINT('Ctrl Pts',(97.2826037832981,-0.843624072369617,
-0.390084122301438));
#23365=CARTESIAN_POINT('Ctrl Pts',(97.2596099943568,-0.865202343965956,
-0.392311658655913));
#23366=CARTESIAN_POINT('Ctrl Pts',(97.2527221509007,-0.871513750700355,
-0.39296715274739));
#23367=CARTESIAN_POINT('Ctrl Pts',(97.2419402985011,-0.88115981102705,-0.393974232478295));
#23368=CARTESIAN_POINT('Ctrl Pts',(97.2380985494794,-0.884551975423763,
-0.394329419251078));
#23369=CARTESIAN_POINT('Ctrl Pts',(97.2309868797649,-0.890749253457098,
-0.394980046441199));
#23370=CARTESIAN_POINT('Ctrl Pts',(97.2277234941237,-0.89356169361344,-0.395275979316444));
#23371=CARTESIAN_POINT('Ctrl Pts',(97.2220939187674,-0.898359776486915,
-0.39578188883736));
#23372=CARTESIAN_POINT('Ctrl Pts',(97.2197352316942,-0.900354118570464,
-0.395992484975316));
#23373=CARTESIAN_POINT('Ctrl Pts',(97.2151804080346,-0.904174732838357,
-0.39639649511028));
#23374=CARTESIAN_POINT('Ctrl Pts',(97.2129854537589,-0.906002313312708,
-0.396590009691239));
#23375=CARTESIAN_POINT('Ctrl Pts',(97.20775142626,-0.910328168317545,-0.397048730528729));
#23376=CARTESIAN_POINT('Ctrl Pts',(97.2047064170228,-0.912819255964677,
-0.39731343043369));
#23377=CARTESIAN_POINT('Ctrl Pts',(97.1938746389186,-0.921590380420619,
-0.398247601276371));
#23378=CARTESIAN_POINT('Ctrl Pts',(97.1860201418531,-0.927786629336338,
-0.398911504529218));
#23379=CARTESIAN_POINT('Ctrl Pts',(97.1274032075592,-0.972828586360824,
-0.403775394732494));
#23380=CARTESIAN_POINT('Ctrl Pts',(97.0736255359534,-1.00758952055075,-0.407744936598658));
#23381=CARTESIAN_POINT('Ctrl Pts',(96.9628335653648,-1.06703112701297,-0.415527671305366));
#23382=CARTESIAN_POINT('Ctrl Pts',(96.9061698609204,-1.09191318868212,-0.419331122902057));
#23383=CARTESIAN_POINT('Ctrl Pts',(96.8143642675086,-1.12388455892939,-0.425504562497344));
#23384=CARTESIAN_POINT('Ctrl Pts',(96.7804053869462,-1.13401846613699,-0.427789056511789));
#23385=CARTESIAN_POINT('Ctrl Pts',(96.7366376884247,-1.14495699488098,-0.430761529832749));
#23386=CARTESIAN_POINT('Ctrl Pts',(96.727203103462,-1.14719150447881,-0.431403856280194));
#23387=CARTESIAN_POINT('Ctrl Pts',(96.7119027582329,-1.15061633250221,-0.432448575648654));
#23388=CARTESIAN_POINT('Ctrl Pts',(96.7060535000077,-1.15187889586214,-0.432848680443888));
#23389=CARTESIAN_POINT('Ctrl Pts',(96.6948225444863,-1.15421366724631,-0.433618389107223));
#23390=CARTESIAN_POINT('Ctrl Pts',(96.6894424644627,-1.15529294800911,-0.433987759314069));
#23391=CARTESIAN_POINT('Ctrl Pts',(96.6771296621551,-1.15767359506622,-0.43483467085645));
#23392=CARTESIAN_POINT('Ctrl Pts',(96.6701924524564,-1.15895034371545,-0.435312970227495));
#23393=CARTESIAN_POINT('Ctrl Pts',(96.64871663689,-1.16270369774481,-0.436797395805814));
#23394=CARTESIAN_POINT('Ctrl Pts',(96.6341431435467,-1.16496951506449,-0.43781002015643));
#23395=CARTESIAN_POINT('Ctrl Pts',(96.5304332668459,-1.17910461722937,-0.445056738645634));
#23396=CARTESIAN_POINT('Ctrl Pts',(96.4402532700717,-1.18100210103111,-0.451603848062412));
#23397=CARTESIAN_POINT('Ctrl Pts',(96.3330120482362,-1.17096725549395,-0.459504678241724));
#23398=CARTESIAN_POINT('Ctrl Pts',(96.3153088108866,-1.16890448561184,-0.460811442676354));
#23399=CARTESIAN_POINT('Ctrl Pts',(96.2534134697254,-1.16026459829467,-0.465378565572855));
#23400=CARTESIAN_POINT('Ctrl Pts',(96.2095503574649,-1.1515752416042,-0.468613282352042));
#23401=CARTESIAN_POINT('Ctrl Pts',(96.1569795149387,-1.138013295214,-0.472414445999536));
#23402=CARTESIAN_POINT('Ctrl Pts',(96.1477052079481,-1.13549933116797,-0.473082049171882));
#23403=CARTESIAN_POINT('Ctrl Pts',(96.1344440850418,-1.13172986020041,-0.47403136114128));
#23404=CARTESIAN_POINT('Ctrl Pts',(96.1304318537952,-1.13056627811609,-0.4743178830513));
#23405=CARTESIAN_POINT('Ctrl Pts',(96.1234678780811,-1.12850643199712,-0.474813879337796));
#23406=CARTESIAN_POINT('Ctrl Pts',(96.1205133335706,-1.12761988205035,-0.47502389568723));
#23407=CARTESIAN_POINT('Ctrl Pts',(96.1142659347862,-1.12571848077101,-0.475467061339255));
#23408=CARTESIAN_POINT('Ctrl Pts',(96.1109740210883,-1.12470077892736,-0.475700046185299));
#23409=CARTESIAN_POINT('Ctrl Pts',(96.1020183155644,-1.12188898681131,-0.476332559052906));
#23410=CARTESIAN_POINT('Ctrl Pts',(96.0963634630065,-1.12006643479134,-0.476730493953298));
#23411=CARTESIAN_POINT('Ctrl Pts',(96.0693878937946,-1.1111463536967,-0.478622918039608));
#23412=CARTESIAN_POINT('Ctrl Pts',(96.0482578738526,-1.10348189409222,-0.480087705162348));
#23413=CARTESIAN_POINT('Ctrl Pts',(95.9315902415259,-1.05734366709929,-0.488144435009503));
#23414=CARTESIAN_POINT('Ctrl Pts',(95.8411968708528,-1.00707107590836,-0.494305631442383));
#23415=CARTESIAN_POINT('Ctrl Pts',(95.7365015771007,-0.929353974180032,
-0.502537883011989));
#23416=CARTESIAN_POINT('Ctrl Pts',(95.7150908513257,-0.912271004488046,
-0.504285583845986));
#23417=CARTESIAN_POINT('Ctrl Pts',(95.6798282908509,-0.882065408523191,
-0.507294611658994));
#23418=CARTESIAN_POINT('Ctrl Pts',(95.6656641508287,-0.86932396088567,-0.508541594396956));
#23419=CARTESIAN_POINT('Ctrl Pts',(95.6461717376941,-0.850914707735897,
-0.510316666380331));
#23420=CARTESIAN_POINT('Ctrl Pts',(95.6405805893273,-0.845528667083554,
-0.510832934842955));
#23421=CARTESIAN_POINT('Ctrl Pts',(95.6310659143291,-0.836179916407774,
-0.511724078215793));
#23422=CARTESIAN_POINT('Ctrl Pts',(95.6271164837528,-0.832243845626137,
-0.512097797509473));
#23423=CARTESIAN_POINT('Ctrl Pts',(95.6196230058521,-0.824668891885829,
-0.512814310352976));
#23424=CARTESIAN_POINT('Ctrl Pts',(95.6160742496399,-0.821034826594318,
-0.513156887551569));
#23425=CARTESIAN_POINT('Ctrl Pts',(95.6078127972499,-0.812464558746713,
-0.513962145954227));
#23426=CARTESIAN_POINT('Ctrl Pts',(95.6031193197148,-0.807510166782562,
-0.514425633124294));
#23427=CARTESIAN_POINT('Ctrl Pts',(95.589387568834,-0.792760380530263,-0.515799745379227));
#23428=CARTESIAN_POINT('Ctrl Pts',(95.5804724683874,-0.782852314762888,
-0.516715452300022));
#23429=CARTESIAN_POINT('Ctrl Pts',(95.5111181626091,-0.703091411133919,
-0.524032195534013));
#23430=CARTESIAN_POINT('Ctrl Pts',(95.4589301588594,-0.626511645363865,
-0.530768169076817));
#23431=CARTESIAN_POINT('Ctrl Pts',(95.3870295048484,-0.488655627230942,
-0.542179085015026));
#23432=CARTESIAN_POINT('Ctrl Pts',(95.3623752128076,-0.430404306197625,
-0.54680356069869));
#23433=CARTESIAN_POINT('Ctrl Pts',(95.339936571119,-0.362687542914304,-0.551781786799588));
#23434=CARTESIAN_POINT('Ctrl Pts',(95.337444801866,-0.354896855630555,-0.552348691949884));
#23435=CARTESIAN_POINT('Ctrl Pts',(95.3338830769724,-0.343347574015294,
-0.553179880678885));
#23436=CARTESIAN_POINT('Ctrl Pts',(95.3327504023157,-0.339608799970925,
-0.553447537500628));
#23437=CARTESIAN_POINT('Ctrl Pts',(95.3307677716046,-0.332945152200068,
-0.553921979334297));
#23438=CARTESIAN_POINT('Ctrl Pts',(95.3299105364955,-0.330022545678446,
-0.554129171267704));
#23439=CARTESIAN_POINT('Ctrl Pts',(95.3280664273338,-0.323643831836692,
-0.554579420538322));
#23440=CARTESIAN_POINT('Ctrl Pts',(95.3270840304339,-0.320186515354768,
-0.554822222302329));
#23441=CARTESIAN_POINT('Ctrl Pts',(95.3243796908818,-0.310500803848293,
-0.555499118262961));
#23442=CARTESIAN_POINT('Ctrl Pts',(95.3226931261551,-0.304262539162929,
-0.55593125998588));
#23443=CARTESIAN_POINT('Ctrl Pts',(95.3131446598321,-0.267754627932298,
-0.558439681465034));
#23444=CARTESIAN_POINT('Ctrl Pts',(95.3064388270834,-0.237192469622415,
-0.560457316304132));
#23445=CARTESIAN_POINT('Ctrl Pts',(95.2828459683939,-0.104649286476163,
-0.568997223734907));
#23446=CARTESIAN_POINT('Ctrl Pts',(95.2782047698755,-0.000959642945746481,
-0.575188967530022));
#23447=CARTESIAN_POINT('Ctrl Pts',(95.2890334061612,0.123592247912445,-0.583151241255716));
#23448=CARTESIAN_POINT('Ctrl Pts',(95.2915048553716,0.145117872134375,-0.584544587217426));
#23449=CARTESIAN_POINT('Ctrl Pts',(95.2968257556906,0.182363451527379,-0.586994379173968));
#23450=CARTESIAN_POINT('Ctrl Pts',(95.2994040233507,0.198116557834131,-0.588042703817235));
#23451=CARTESIAN_POINT('Ctrl Pts',(95.3036155157851,0.220929440703581,-0.589580856496452));
#23452=CARTESIAN_POINT('Ctrl Pts',(95.3049950619999,0.228034667037812,-0.590062761988184));
#23453=CARTESIAN_POINT('Ctrl Pts',(95.3075345994478,0.240499144872412,-0.590913355505525));
#23454=CARTESIAN_POINT('Ctrl Pts',(95.30866670098,0.245863905353598,-0.591281155645434));
#23455=CARTESIAN_POINT('Ctrl Pts',(95.3109458082844,0.256302714917933,-0.592000231632617));
#23456=CARTESIAN_POINT('Ctrl Pts',(95.3120890549894,0.261377462091896,-0.592351380784895));
#23457=CARTESIAN_POINT('Ctrl Pts',(95.3152573433004,0.275018987825597,-0.593299649006156));
#23458=CARTESIAN_POINT('Ctrl Pts',(95.3173448410281,0.283570770832722,-0.593898735068732));
#23459=CARTESIAN_POINT('Ctrl Pts',(95.3256003580512,0.315817317966197,-0.59617574555046));
#23460=CARTESIAN_POINT('Ctrl Pts',(95.332410497508,0.339339706891084,-0.597873851692947));
#23461=CARTESIAN_POINT('Ctrl Pts',(95.3708228260312,0.458033991083355,-0.606639205950092));
#23462=CARTESIAN_POINT('Ctrl Pts',(95.4137522649853,0.549092584150526,-0.614066800457536));
#23463=CARTESIAN_POINT('Ctrl Pts',(95.4835850573301,0.658516218059673,-0.62353278495938));
#23464=CARTESIAN_POINT('Ctrl Pts',(95.5004244603388,0.682833044100112,-0.625671400343901));
#23465=CARTESIAN_POINT('Ctrl Pts',(95.5282687066087,0.719971697025328,-0.628966703663235));
#23466=CARTESIAN_POINT('Ctrl Pts',(95.5386638619967,0.733234096361876,-0.630149578985386));
#23467=CARTESIAN_POINT('Ctrl Pts',(95.5526134626546,0.750265530815474,-0.631671973309801));
#23468=CARTESIAN_POINT('Ctrl Pts',(95.555912591069,0.75423990069677,-0.632027475570406));
#23469=CARTESIAN_POINT('Ctrl Pts',(95.5613428018692,0.760694646566433,-0.632605066966588));
#23470=CARTESIAN_POINT('Ctrl Pts',(95.5634582123561,0.763188026341498,-0.632828237512009));
#23471=CARTESIAN_POINT('Ctrl Pts',(95.5676086356474,0.768038926166544,-0.633262471452468));
#23472=CARTESIAN_POINT('Ctrl Pts',(95.5696426537094,0.770397230046601,-0.633473598879998));
#23473=CARTESIAN_POINT('Ctrl Pts',(95.5742060871919,0.775645977829048,-0.633943612181957));
#23474=CARTESIAN_POINT('Ctrl Pts',(95.5767403593831,0.778532199006007,-0.63420214810385));
#23475=CARTESIAN_POINT('Ctrl Pts',(95.5855539895755,0.788471336881261,-0.635092951167112));
#23476=CARTESIAN_POINT('Ctrl Pts',(95.591904219335,0.795461320174383,-0.635720304095556));
#23477=CARTESIAN_POINT('Ctrl Pts',(95.6511517069113,0.85912212087262,-0.641450384559067));
#23478=CARTESIAN_POINT('Ctrl Pts',(95.7094471544897,0.91052533541087,-0.646207497355856));
#23479=CARTESIAN_POINT('Ctrl Pts',(95.8167297554877,0.987757933655887,-0.654385905932889));
#23480=CARTESIAN_POINT('Ctrl Pts',(95.8632456112907,1.01655824077084,-0.657775375548533));
#23481=CARTESIAN_POINT('Ctrl Pts',(95.9149851355834,1.04381229502683,-0.661508623022443));
#23482=CARTESIAN_POINT('Ctrl Pts',(95.9183891636579,1.0455841831001,-0.661754055889336));
#23483=CARTESIAN_POINT('Ctrl Pts',(95.9218016734189,1.0473393432588,-0.661999947661213));
#23484=CARTESIAN_POINT('Origin',(96.460480949577,-7.19464945638997E-16,
0.924367114736168));
#23485=CARTESIAN_POINT('',(95.9218016672795,1.0473393401011,-1.26059202888094));
#23486=CARTESIAN_POINT('',(95.9218016937941,1.04733935373838,-1.1624507611287));
#23487=CARTESIAN_POINT('',(95.9218016730721,1.04733934308042,0.924367114736168));
#23488=CARTESIAN_POINT('',(97.6382305348814,-0.00104073772955277,-0.924212417541179));
#23489=CARTESIAN_POINT('Ctrl Pts',(95.9218016672795,1.04733934010109,-1.26059202888093));
#23490=CARTESIAN_POINT('Ctrl Pts',(95.9124909570254,1.04255055147708,-1.25985189138548));
#23491=CARTESIAN_POINT('Ctrl Pts',(95.9032430830649,1.03763708108747,-1.2591170773026));
#23492=CARTESIAN_POINT('Ctrl Pts',(95.8885707434698,1.02958874570432,-1.25795317209041));
#23493=CARTESIAN_POINT('Ctrl Pts',(95.8831048669043,1.02653355158647,-1.25752001752847));
#23494=CARTESIAN_POINT('Ctrl Pts',(95.8742870279693,1.02151203921229,-1.25682224850314));
#23495=CARTESIAN_POINT('Ctrl Pts',(95.8709200601205,1.01957251762484,-1.25655605840964));
#23496=CARTESIAN_POINT('Ctrl Pts',(95.864931242162,1.01608310871101,-1.25608310502353));
#23497=CARTESIAN_POINT('Ctrl Pts',(95.8623057467824,1.01453968146771,-1.25587594672969));
#23498=CARTESIAN_POINT('Ctrl Pts',(95.8565779764428,1.01114258179217,-1.25542442204969));
#23499=CARTESIAN_POINT('Ctrl Pts',(95.8534782306762,1.00928480707794,-1.25518032116734));
#23500=CARTESIAN_POINT('Ctrl Pts',(95.8446303081737,1.00392646351676,-1.25448414295944));
#23501=CARTESIAN_POINT('Ctrl Pts',(95.8389034051741,1.00039078274829,-1.25403424444454));
#23502=CARTESIAN_POINT('Ctrl Pts',(95.797090520294,0.974078609272367,-1.25075228311072));
#23503=CARTESIAN_POINT('Ctrl Pts',(95.7622314401185,0.949402180134824,-1.24803114254563));
#23504=CARTESIAN_POINT('Ctrl Pts',(95.6569933917553,0.865965742160164,-1.23960744590673));
#23505=CARTESIAN_POINT('Ctrl Pts',(95.5920898069141,0.800865892348069,-1.23406931740228));
#23506=CARTESIAN_POINT('Ctrl Pts',(95.5155508720362,0.703725404878514,-1.22619237992788));
#23507=CARTESIAN_POINT('Ctrl Pts',(95.4967525246725,0.677753299100132,-1.22412116278549));
#23508=CARTESIAN_POINT('Ctrl Pts',(95.4736715895503,0.642959240143239,-1.22137030981065));
#23509=CARTESIAN_POINT('Ctrl Pts',(95.4684057498474,0.634803974735654,-1.22072722837716));
#23510=CARTESIAN_POINT('Ctrl Pts',(95.4600607763342,0.62152255143322,-1.21968212205514));
#23511=CARTESIAN_POINT('Ctrl Pts',(95.4569187454284,0.616436294475653,-1.21928240073601));
#23512=CARTESIAN_POINT('Ctrl Pts',(95.450974505995,0.606647972576106,-1.21851401131606));
#23513=CARTESIAN_POINT('Ctrl Pts',(95.4481660789842,0.601949851155458,-1.21814558058679));
#23514=CARTESIAN_POINT('Ctrl Pts',(95.4417682914031,0.591075804647422,-1.21729359409879));
#23515=CARTESIAN_POINT('Ctrl Pts',(95.4382021957157,0.584886512305568,-1.21680922302402));
#23516=CARTESIAN_POINT('Ctrl Pts',(95.4271172572576,0.565236465655884,-1.21527294699474));
#23517=CARTESIAN_POINT('Ctrl Pts',(95.419806583154,0.55166077144025,-1.21421379189066));
#23518=CARTESIAN_POINT('Ctrl Pts',(95.4033084353605,0.5195285958921,-1.21171086258152));
#23519=CARTESIAN_POINT('Ctrl Pts',(95.3943398781203,0.500866062612544,-1.21026013151297));
#23520=CARTESIAN_POINT('Ctrl Pts',(95.3627862867526,0.430514504873537,-1.20480176114072));
#23521=CARTESIAN_POINT('Ctrl Pts',(95.3434334155344,0.377465027147153,-1.20070165693744));
#23522=CARTESIAN_POINT('Ctrl Pts',(95.3074172711921,0.251276227315327,-1.19108140531528));
#23523=CARTESIAN_POINT('Ctrl Pts',(95.2937820379467,0.177513712894609,-1.1855523505221));
#23524=CARTESIAN_POINT('Ctrl Pts',(95.2864013510727,0.0934025379049221,
-1.17963729572722));
#23525=CARTESIAN_POINT('Ctrl Pts',(95.2856800443095,0.0838438150060226,
-1.17897088378348));
#23526=CARTESIAN_POINT('Ctrl Pts',(95.2848316916561,0.070418951065792,-1.178044022437));
#23527=CARTESIAN_POINT('Ctrl Pts',(95.284606884592,0.0665596775109735,-1.17777862838284));
#23528=CARTESIAN_POINT('Ctrl Pts',(95.2842349254296,0.059582666803825,-1.17730081914477));
#23529=CARTESIAN_POINT('Ctrl Pts',(95.2840811572407,0.0564653247373613,
-1.17708804899433));
#23530=CARTESIAN_POINT('Ctrl Pts',(95.2837919640534,0.0500873557338245,
-1.17665424130214));
#23531=CARTESIAN_POINT('Ctrl Pts',(95.283657695698,0.0468267193401669,-1.17643326804342));
#23532=CARTESIAN_POINT('Ctrl Pts',(95.2833473591183,0.0384428232385585,
-1.17586706160092));
#23533=CARTESIAN_POINT('Ctrl Pts',(95.2831911813203,0.0333188294994105,
-1.17552290312707));
#23534=CARTESIAN_POINT('Ctrl Pts',(95.2826742418162,0.0117307616841884,
-1.17408026397162));
#23535=CARTESIAN_POINT('Ctrl Pts',(95.2826253333605,-0.00473982236947986,
-1.17299759331857));
#23536=CARTESIAN_POINT('Ctrl Pts',(95.2834364301867,-0.0497775063634159,
-1.17007310830347));
#23537=CARTESIAN_POINT('Ctrl Pts',(95.2849906209954,-0.0783218708327382,
-1.16825913657225));
#23538=CARTESIAN_POINT('Ctrl Pts',(95.295535584052,-0.194146924935691,-1.16096066227737));
#23539=CARTESIAN_POINT('Ctrl Pts',(95.3132247607793,-0.280347081034544,
-1.15565194527878));
#23540=CARTESIAN_POINT('Ctrl Pts',(95.3513597993906,-0.397771595732273,
-1.1478200029324));
#23541=CARTESIAN_POINT('Ctrl Pts',(95.3639373760131,-0.431235174541892,
-1.14551818412745));
#23542=CARTESIAN_POINT('Ctrl Pts',(95.3820023193155,-0.473372237807435,
-1.14250042879455));
#23543=CARTESIAN_POINT('Ctrl Pts',(95.3861086134336,-0.48261941975773,-1.14183062993081));
#23544=CARTESIAN_POINT('Ctrl Pts',(95.3928673445161,-0.497325922631234,
-1.14075270757178));
#23545=CARTESIAN_POINT('Ctrl Pts',(95.395443787189,-0.502819772320877,-1.14034716341966));
#23546=CARTESIAN_POINT('Ctrl Pts',(95.4004153985107,-0.513211273847619,
-1.1395744967103));
#23547=CARTESIAN_POINT('Ctrl Pts',(95.4028023523809,-0.518112697665197,
-1.1392076632697));
#23548=CARTESIAN_POINT('Ctrl Pts',(95.4083181477115,-0.529241981979873,
-1.13836917810798));
#23549=CARTESIAN_POINT('Ctrl Pts',(95.4114683902067,-0.53545894687706,-1.13789679754734));
#23550=CARTESIAN_POINT('Ctrl Pts',(95.4213374349547,-0.554513997220439,
-1.13643638217215));
#23551=CARTESIAN_POINT('Ctrl Pts',(95.4282379070595,-0.56725592622167,-1.1354420774274));
#23552=CARTESIAN_POINT('Ctrl Pts',(95.4632361181719,-0.62912702703182,-1.13052404786013));
#23553=CARTESIAN_POINT('Ctrl Pts',(95.4946110860976,-0.676307479226715,
-1.12648582006652));
#23554=CARTESIAN_POINT('Ctrl Pts',(95.5669868263335,-0.769780827820381,
-1.11789205804334));
#23555=CARTESIAN_POINT('Ctrl Pts',(95.6084890700907,-0.815477652153749,
-1.11333495959732));
#23556=CARTESIAN_POINT('Ctrl Pts',(95.6821768532518,-0.884817369836728,
-1.10597255643867));
#23557=CARTESIAN_POINT('Ctrl Pts',(95.7123278684236,-0.910454116505678,
-1.10313099529562));
#23558=CARTESIAN_POINT('Ctrl Pts',(95.7486650249066,-0.938324075352465,
-1.09994622954635));
#23559=CARTESIAN_POINT('Ctrl Pts',(95.753645381812,-0.942081453666663,-1.09951469441509));
#23560=CARTESIAN_POINT('Ctrl Pts',(95.7617702695327,-0.948110485153555,
-1.09881901079236));
#23561=CARTESIAN_POINT('Ctrl Pts',(95.7648965016738,-0.950406430630044,
-1.09855330152303));
#23562=CARTESIAN_POINT('Ctrl Pts',(95.7704972583483,-0.954477260541574,
-1.09808086176581));
#23563=CARTESIAN_POINT('Ctrl Pts',(95.7729673764979,-0.956258031380015,
-1.09787373987894));
#23564=CARTESIAN_POINT('Ctrl Pts',(95.7783883697733,-0.960134299360713,
-1.0974218961112));
#23565=CARTESIAN_POINT('Ctrl Pts',(95.7813420108848,-0.962225785907608,
-1.09717744265485));
#23566=CARTESIAN_POINT('Ctrl Pts',(95.7898363360079,-0.968182058903928,
-1.09647923238217));
#23567=CARTESIAN_POINT('Ctrl Pts',(95.7954008035634,-0.972012912247251,
-1.09602767428959));
#23568=CARTESIAN_POINT('Ctrl Pts',(95.8370547656034,-1.00016437035739,-1.09268805648767));
#23569=CARTESIAN_POINT('Ctrl Pts',(95.8744389910636,-1.02251881222603,-1.08991540596361));
#23570=CARTESIAN_POINT('Ctrl Pts',(96.0016566312504,-1.08931485285468,-1.08090944030054));
#23571=CARTESIAN_POINT('Ctrl Pts',(96.0959065195447,-1.12437196226241,-1.07486860092377));
#23572=CARTESIAN_POINT('Ctrl Pts',(96.2173064670503,-1.15263214177568,-1.06685673614855));
#23573=CARTESIAN_POINT('Ctrl Pts',(96.2413218258221,-1.1574384765649,-1.06526352103096));
#23574=CARTESIAN_POINT('Ctrl Pts',(96.2741543962825,-1.16295101101242,-1.06306550008254));
#23575=CARTESIAN_POINT('Ctrl Pts',(96.2828564242327,-1.16431188240613,-1.06248107236912));
#23576=CARTESIAN_POINT('Ctrl Pts',(96.2967249274311,-1.16632162397627,-1.06154635589683));
#23577=CARTESIAN_POINT('Ctrl Pts',(96.3018819715535,-1.1670340732127,-1.06119805415939));
#23578=CARTESIAN_POINT('Ctrl Pts',(96.3124848960986,-1.16842729798062,-1.06048037372655));
#23579=CARTESIAN_POINT('Ctrl Pts',(96.3179311424039,-1.16910424395648,-1.06011088520195));
#23580=CARTESIAN_POINT('Ctrl Pts',(96.3305790794201,-1.17058663857696,-1.05925075190084));
#23581=CARTESIAN_POINT('Ctrl Pts',(96.3377838049122,-1.17136372699265,-1.05875923992152));
#23582=CARTESIAN_POINT('Ctrl Pts',(96.3609064790329,-1.17364203103342,-1.0571765795812));
#23583=CARTESIAN_POINT('Ctrl Pts',(96.376847411003,-1.17488556035057,-1.05607754560635));
#23584=CARTESIAN_POINT('Ctrl Pts',(96.4144788704661,-1.17705142234109,-1.05346313378178));
#23585=CARTESIAN_POINT('Ctrl Pts',(96.436178749755,-1.17769925801184,-1.05193992448423));
#23586=CARTESIAN_POINT('Ctrl Pts',(96.5617269039242,-1.17797620020088,-1.04303641956692));
#23587=CARTESIAN_POINT('Ctrl Pts',(96.6651405634321,-1.16446886721859,-1.03528776949736));
#23588=CARTESIAN_POINT('Ctrl Pts',(96.7951197415441,-1.12962714322742,-1.02556444795194));
#23589=CARTESIAN_POINT('Ctrl Pts',(96.8245006383974,-1.12050463434462,-1.02337224247196));
#23590=CARTESIAN_POINT('Ctrl Pts',(96.8595614623931,-1.10809351730552,-1.02078877066075));
#23591=CARTESIAN_POINT('Ctrl Pts',(96.8656120519584,-1.10589569731973,-1.02034413553984));
#23592=CARTESIAN_POINT('Ctrl Pts',(96.8750088372945,-1.10239493043487,-1.01965581053436));
#23593=CARTESIAN_POINT('Ctrl Pts',(96.8783674972106,-1.10112614468873,-1.01941022754282));
#23594=CARTESIAN_POINT('Ctrl Pts',(96.8845665795091,-1.09875189659968,-1.01895784271981));
#23595=CARTESIAN_POINT('Ctrl Pts',(96.8874085090051,-1.09765076921486,-1.01875080425368));
#23596=CARTESIAN_POINT('Ctrl Pts',(96.8938195606446,-1.09513809205787,-1.01828452367841));
#23597=CARTESIAN_POINT('Ctrl Pts',(96.8973860810425,-1.09372011943526,-1.01802566373096));
#23598=CARTESIAN_POINT('Ctrl Pts',(96.908187517084,-1.08936443136305,-1.01724313251011));
#23599=CARTESIAN_POINT('Ctrl Pts',(96.9154003826095,-1.08637210585536,-1.01672255399734));
#23600=CARTESIAN_POINT('Ctrl Pts',(96.932261770753,-1.07917961394909,-1.01550904237972));
#23601=CARTESIAN_POINT('Ctrl Pts',(96.9418849612362,-1.07492138170674,-1.01481913043827));
#23602=CARTESIAN_POINT('Ctrl Pts',(96.9754710792321,-1.0595180965846,-1.01241626403282));
#23603=CARTESIAN_POINT('Ctrl Pts',(96.999116082,-1.04769547718561,-1.01073359862451));
#23604=CARTESIAN_POINT('Ctrl Pts',(97.1009420444648,-0.992422492754522,
-1.00344255079753));
#23605=CARTESIAN_POINT('Ctrl Pts',(97.1744240522513,-0.940945761401129,
-0.998039341482925));
#23606=CARTESIAN_POINT('Ctrl Pts',(97.2691348069077,-0.857058496987549,
-0.990023897388688));
#23607=CARTESIAN_POINT('Ctrl Pts',(97.2957164893404,-0.831174769270511,
-0.987637552706962));
#23608=CARTESIAN_POINT('Ctrl Pts',(97.327994502585,-0.796629977571779,-0.984526096777031));
#23609=CARTESIAN_POINT('Ctrl Pts',(97.3348604807485,-0.789087771151467,
-0.983850997318281));
#23610=CARTESIAN_POINT('Ctrl Pts',(97.3456654839905,-0.776904395144889,
-0.982766560201739));
#23611=CARTESIAN_POINT('Ctrl Pts',(97.3496680841486,-0.772320099780294,
-0.98235985806375));
#23612=CARTESIAN_POINT('Ctrl Pts',(97.3571863493935,-0.763573292261414,
-0.981586278932822));
#23613=CARTESIAN_POINT('Ctrl Pts',(97.3607090205332,-0.759416990373271,
-0.981219701023391));
#23614=CARTESIAN_POINT('Ctrl Pts',(97.3686519997188,-0.74991236064334,-0.980383602493388));
#23615=CARTESIAN_POINT('Ctrl Pts',(97.3730541031154,-0.744549152735319,
-0.979913368477185));
#23616=CARTESIAN_POINT('Ctrl Pts',(97.3857719141876,-0.728772448150182,
-0.978534400550419));
#23617=CARTESIAN_POINT('Ctrl Pts',(97.3939583448664,-0.718256623781256,
-0.977620639102936));
#23618=CARTESIAN_POINT('Ctrl Pts',(97.4359300948534,-0.662412288907622,
-0.972794101565266));
#23619=CARTESIAN_POINT('Ctrl Pts',(97.4665929336296,-0.614839873319073,
-0.96876535672004));
#23620=CARTESIAN_POINT('Ctrl Pts',(97.516707567981,-0.523234832625769,-0.961180454725356));
#23621=CARTESIAN_POINT('Ctrl Pts',(97.5371109118217,-0.479851024723814,
-0.957654073463454));
#23622=CARTESIAN_POINT('Ctrl Pts',(97.5748625466004,-0.384954599822675,
-0.950172572279888));
#23623=CARTESIAN_POINT('Ctrl Pts',(97.5914075263396,-0.333230945947142,
-0.946230811720642));
#23624=CARTESIAN_POINT('Ctrl Pts',(97.6058621785013,-0.274296024846149,
-0.942008102137619));
#23625=CARTESIAN_POINT('Ctrl Pts',(97.607343771293,-0.268033844086378,-0.941562771856642));
#23626=CARTESIAN_POINT('Ctrl Pts',(97.6096490346917,-0.25792106385158,-0.940849346772095));
#23627=CARTESIAN_POINT('Ctrl Pts',(97.6105048269944,-0.254078030383814,
-0.94057956275809));
#23628=CARTESIAN_POINT('Ctrl Pts',(97.6119892382536,-0.247250930128726,
-0.940102738622853));
#23629=CARTESIAN_POINT('Ctrl Pts',(97.6126255566902,-0.244268635706022,
-0.939895276606408));
#23630=CARTESIAN_POINT('Ctrl Pts',(97.6139828345146,-0.237784038228632,
-0.939445992250417));
#23631=CARTESIAN_POINT('Ctrl Pts',(97.6146994321108,-0.234280905794114,
-0.939204414362909));
#23632=CARTESIAN_POINT('Ctrl Pts',(97.6161480392174,-0.227031300609771,
-0.938706722046309));
#23633=CARTESIAN_POINT('Ctrl Pts',(97.6168778118979,-0.223284418018694,
-0.93845073090803));
#23634=CARTESIAN_POINT('Ctrl Pts',(97.6187096775019,-0.213629115425764,
-0.937794093620395));
#23635=CARTESIAN_POINT('Ctrl Pts',(97.619784799232,-0.207715605748008,-0.937394836571943));
#23636=CARTESIAN_POINT('Ctrl Pts',(97.6323431383334,-0.135504017529939,
-0.932551945019631));
#23637=CARTESIAN_POINT('Ctrl Pts',(97.6381710435508,-0.0683401826375768,
-0.928377508108212));
#23638=CARTESIAN_POINT('Ctrl Pts',(97.6382304901167,-0.00104031656738834,
-0.924212313232804));
#23639=CARTESIAN_POINT('Ctrl Pts',(97.6382304897404,-0.00104074251348296,
-0.924212339594643));
#23640=CARTESIAN_POINT('Ctrl Pts',(97.6383086585134,0.087418444371562,-0.918737592289391));
#23641=CARTESIAN_POINT('Ctrl Pts',(97.6284213334225,0.175597665774794,-0.913292158566966));
#23642=CARTESIAN_POINT('Ctrl Pts',(97.6065569748955,0.271482309211362,-0.906868613012748));
#23643=CARTESIAN_POINT('Ctrl Pts',(97.6042365879264,0.281097723819844,-0.906219031606458));
#23644=CARTESIAN_POINT('Ctrl Pts',(97.600193161266,0.296973535564489,-0.905136898968108));
#23645=CARTESIAN_POINT('Ctrl Pts',(97.5985389424447,0.303251064941707,-0.904706498433585));
#23646=CARTESIAN_POINT('Ctrl Pts',(97.595199203206,0.315512588634975,-0.903860721769332));
#23647=CARTESIAN_POINT('Ctrl Pts',(97.5935180317108,0.321497553204364,-0.903445495359054));
#23648=CARTESIAN_POINT('Ctrl Pts',(97.5902799656531,0.332684120375035,-0.902664763176757));
#23649=CARTESIAN_POINT('Ctrl Pts',(97.5887343240487,0.337888830799272,-0.902299627870652));
#23650=CARTESIAN_POINT('Ctrl Pts',(97.5851908284601,0.349525552391896,-0.901478925396652));
#23651=CARTESIAN_POINT('Ctrl Pts',(97.5831736901027,0.355951444083561,-0.901022745579801));
#23652=CARTESIAN_POINT('Ctrl Pts',(97.5778954730715,0.372274675046682,-0.899856163598356));
#23653=CARTESIAN_POINT('Ctrl Pts',(97.574558004916,0.382146508122994,-0.899143310330824));
#23654=CARTESIAN_POINT('Ctrl Pts',(97.5483577604015,0.456381898599413,-0.893725681538761));
#23655=CARTESIAN_POINT('Ctrl Pts',(97.5200696032039,0.51868038345569,-0.888841803407394));
#23656=CARTESIAN_POINT('Ctrl Pts',(97.4578171927982,0.62915903863508,-0.879591269695259));
#23657=CARTESIAN_POINT('Ctrl Pts',(97.4253242814016,0.677936570523005,-0.875265808775647));
#23658=CARTESIAN_POINT('Ctrl Pts',(97.3742360092596,0.743471784678426,-0.869234871334851));
#23659=CARTESIAN_POINT('Ctrl Pts',(97.3585282978016,0.762371116019068,-0.867467677670331));
#23660=CARTESIAN_POINT('Ctrl Pts',(97.3324854923082,0.791782575044832,-0.864688149693622));
#23661=CARTESIAN_POINT('Ctrl Pts',(97.3225248755267,0.802615653912336,-0.863657628258942));
#23662=CARTESIAN_POINT('Ctrl Pts',(97.3090232215204,0.816758515284516,-0.862306379825623));
#23663=CARTESIAN_POINT('Ctrl Pts',(97.3056615460485,0.820236685932479,-0.861973580504424));
#23664=CARTESIAN_POINT('Ctrl Pts',(97.2999932433029,0.826029568315095,-0.861418636342975));
#23665=CARTESIAN_POINT('Ctrl Pts',(97.297698277208,0.828355531172675,-0.861195631753239));
#23666=CARTESIAN_POINT('Ctrl Pts',(97.2931943594301,0.832882442247074,-0.860761303963134));
#23667=CARTESIAN_POINT('Ctrl Pts',(97.2909863061762,0.835084210460701,-0.860549919913104));
#23668=CARTESIAN_POINT('Ctrl Pts',(97.2860290374284,0.839988260136294,-0.860078716670001));
#23669=CARTESIAN_POINT('Ctrl Pts',(97.283275220611,0.842685891132548,-0.859819253064847));
#23670=CARTESIAN_POINT('Ctrl Pts',(97.2736731780032,0.852000080448579,-0.858922262303198));
#23671=CARTESIAN_POINT('Ctrl Pts',(97.2667577717605,0.858547283259369,-0.858289739748856));
#23672=CARTESIAN_POINT('Ctrl Pts',(97.2041614266855,0.916387256190625,-0.852675312332903));
#23673=CARTESIAN_POINT('Ctrl Pts',(97.1437268687053,0.962291315162671,-0.848022311707098));
#23674=CARTESIAN_POINT('Ctrl Pts',(97.0317799325913,1.03142195284057,-0.839883340416475));
#23675=CARTESIAN_POINT('Ctrl Pts',(96.9822399099621,1.05734607375344,-0.836423171278922));
#23676=CARTESIAN_POINT('Ctrl Pts',(96.9121810818576,1.08788132197737,-0.831546596753414));
#23677=CARTESIAN_POINT('Ctrl Pts',(96.8930996430919,1.09560931547076,-0.830220522303214));
#23678=CARTESIAN_POINT('Ctrl Pts',(96.8595783497304,1.10817320368518,-0.827887145797917));
#23679=CARTESIAN_POINT('Ctrl Pts',(96.8452288074174,1.11323655871224,-0.8268871324083));
#23680=CARTESIAN_POINT('Ctrl Pts',(96.8239702546377,1.12027770391992,-0.825401969000131));
#23681=CARTESIAN_POINT('Ctrl Pts',(96.8171344230728,1.12247267442038,-0.824923858800875));
#23682=CARTESIAN_POINT('Ctrl Pts',(96.805047722053,1.1262321326089,-0.824077332517465));
#23683=CARTESIAN_POINT('Ctrl Pts',(96.7998051562549,1.12782275125519,-0.823709772586361));
#23684=CARTESIAN_POINT('Ctrl Pts',(96.7888351222316,1.13106769875277,-0.822939767869058));
#23685=CARTESIAN_POINT('Ctrl Pts',(96.7831058223476,1.13271522947239,-0.822537116264939));
#23686=CARTESIAN_POINT('Ctrl Pts',(96.7680899635722,1.13691005976559,-0.821480371550895));
#23687=CARTESIAN_POINT('Ctrl Pts',(96.7587843968713,1.13938704278695,-0.820824053929541));
#23688=CARTESIAN_POINT('Ctrl Pts',(96.719082027392,1.14943543326278,-0.818017091343524));
#23689=CARTESIAN_POINT('Ctrl Pts',(96.6884224795003,1.15590599743773,-0.815832182778312));
#23690=CARTESIAN_POINT('Ctrl Pts',(96.548635955172,1.17962973600319,-0.805786667577385));
#23691=CARTESIAN_POINT('Ctrl Pts',(96.4376919078291,1.18269689179189,-0.797517192434202));
#23692=CARTESIAN_POINT('Ctrl Pts',(96.3019824333502,1.16732883216616,-0.787699858001737));
#23693=CARTESIAN_POINT('Ctrl Pts',(96.2761108158078,1.16352321708239,-0.785845713235984));
#23694=CARTESIAN_POINT('Ctrl Pts',(96.2445158475531,1.15779519717268,-0.783619116489122));
#23695=CARTESIAN_POINT('Ctrl Pts',(96.2386545234577,1.15668651082085,-0.783207664919409));
#23696=CARTESIAN_POINT('Ctrl Pts',(96.2294182374593,1.15486664943739,-0.782562113993727));
#23697=CARTESIAN_POINT('Ctrl Pts',(96.2260376408562,1.15418511976277,-0.782326431373008));
#23698=CARTESIAN_POINT('Ctrl Pts',(96.2196498366781,1.15286811215125,-0.781882289677524));
#23699=CARTESIAN_POINT('Ctrl Pts',(96.2166421454724,1.15223571668187,-0.781673675034372));
#23700=CARTESIAN_POINT('Ctrl Pts',(96.2096518414285,1.15073734234116,-0.781189959071717));
#23701=CARTESIAN_POINT('Ctrl Pts',(96.2056712047136,1.14986245599718,-0.780915359551082));
#23702=CARTESIAN_POINT('Ctrl Pts',(96.1925946986417,1.14691718881578,-0.78001585959267));
#23703=CARTESIAN_POINT('Ctrl Pts',(96.1835186039726,1.14475934324311,-0.77939563175275));
#23704=CARTESIAN_POINT('Ctrl Pts',(96.0952879351267,1.12267165523643,-0.773397712272924));
#23705=CARTESIAN_POINT('Ctrl Pts',(96.0183700125523,1.09466867527989,-0.768406168752027));
#23706=CARTESIAN_POINT('Ctrl Pts',(95.9371961092389,1.05515049884195,-0.762817833787108));
#23707=CARTESIAN_POINT('Ctrl Pts',(95.9294766873309,1.05128684229111,-0.762283141374746));
#23708=CARTESIAN_POINT('Ctrl Pts',(95.921801662562,1.04733933767479,-0.761747732816352));
#23709=CARTESIAN_POINT('Ctrl Pts',(95.9218016734189,1.0473393432588,-0.661999947661213));
#23710=CARTESIAN_POINT('Ctrl Pts',(95.9364629898361,1.05488011537431,-0.663056383341802));
#23711=CARTESIAN_POINT('Ctrl Pts',(95.9512808635733,1.06211211395517,-0.664121325308709));
#23712=CARTESIAN_POINT('Ctrl Pts',(95.9800444240408,1.07541011441399,-0.666187360446632));
#23713=CARTESIAN_POINT('Ctrl Pts',(95.9939649700543,1.08152160207347,-0.667186733626535));
#23714=CARTESIAN_POINT('Ctrl Pts',(96.0145585472731,1.09009116398921,-0.668666374329298));
#23715=CARTESIAN_POINT('Ctrl Pts',(96.0211421273872,1.09276114970359,-0.669139574791691));
#23716=CARTESIAN_POINT('Ctrl Pts',(96.0328362727037,1.09738097680985,-0.669980601250669));
#23717=CARTESIAN_POINT('Ctrl Pts',(96.0379370663037,1.09935510319017,-0.670347609583992));
#23718=CARTESIAN_POINT('Ctrl Pts',(96.0486614798548,1.1034200388425,-0.671119683938864));
#23719=CARTESIAN_POINT('Ctrl Pts',(96.0542876817077,1.10550354346032,-0.671524978474941));
#23720=CARTESIAN_POINT('Ctrl Pts',(96.0691451814749,1.11087686846875,-0.672596059602218));
#23721=CARTESIAN_POINT('Ctrl Pts',(96.0784018846483,1.11409455540222,-0.673264181047839));
#23722=CARTESIAN_POINT('Ctrl Pts',(96.1188904782369,1.12760469767797,-0.676190742391172));
#23723=CARTESIAN_POINT('Ctrl Pts',(96.1505028425569,1.13670119768807,-0.678487153149228));
#23724=CARTESIAN_POINT('Ctrl Pts',(96.2813715526448,1.16849368462877,-0.688045630061959));
#23725=CARTESIAN_POINT('Ctrl Pts',(96.3829853628467,1.17959616510827,-0.6956353657113));
#23726=CARTESIAN_POINT('Ctrl Pts',(96.506341910909,1.17705515656634,-0.704558159220456));
#23727=CARTESIAN_POINT('Ctrl Pts',(96.5279326870397,1.17601549562344,-0.706106850385334));
#23728=CARTESIAN_POINT('Ctrl Pts',(96.5630025435627,1.17335765647055,-0.708589530377186));
#23729=CARTESIAN_POINT('Ctrl Pts',(96.576503275776,1.17209970839442,-0.709537301584107));
#23730=CARTESIAN_POINT('Ctrl Pts',(96.5947231405698,1.17008412928468,-0.710802972999195));
#23731=CARTESIAN_POINT('Ctrl Pts',(96.5994631764258,1.16953058020455,-0.711131017103561));
#23732=CARTESIAN_POINT('Ctrl Pts',(96.6073637098083,1.16855923203408,-0.711675593546746));
#23733=CARTESIAN_POINT('Ctrl Pts',(96.6105260640824,1.16815739022837,-0.711892983658442));
#23734=CARTESIAN_POINT('Ctrl Pts',(96.6165083919057,1.1673725190118,-0.712303065080476));
#23735=CARTESIAN_POINT('Ctrl Pts',(96.6193286681096,1.16699210094103,-0.712495903030268));
#23736=CARTESIAN_POINT('Ctrl Pts',(96.6260029597358,1.16606718335122,-0.712951163109775));
#23737=CARTESIAN_POINT('Ctrl Pts',(96.6298557393433,1.1655137895343,-0.713213096913204));
#23738=CARTESIAN_POINT('Ctrl Pts',(96.6433388042446,1.16350888032907,-0.714126933638863));
#23739=CARTESIAN_POINT('Ctrl Pts',(96.6529540818923,1.16195697769463,-0.714773583129072));
#23740=CARTESIAN_POINT('Ctrl Pts',(96.733275287522,1.14796871871588,-0.720141457338891));
#23741=CARTESIAN_POINT('Ctrl Pts',(96.8027372298633,1.12920877610411,-0.724568867338573));
#23742=CARTESIAN_POINT('Ctrl Pts',(96.9248360783268,1.08391970457276,-0.732624184268632));
#23743=CARTESIAN_POINT('Ctrl Pts',(96.9780156332161,1.05955877934321,-0.736235742921371));
#23744=CARTESIAN_POINT('Ctrl Pts',(97.0476663566816,1.02115359429345,-0.741306206675936));
#23745=CARTESIAN_POINT('Ctrl Pts',(97.0658875633551,1.01045738059093,-0.742666079276758));
#23746=CARTESIAN_POINT('Ctrl Pts',(97.0970967739225,0.990989690156382,-0.745062429332714));
#23747=CARTESIAN_POINT('Ctrl Pts',(97.1102159001589,0.982438155994047,-0.74609128565934));
#23748=CARTESIAN_POINT('Ctrl Pts',(97.1291014086619,0.969584135052225,-0.747606300793059));
#23749=CARTESIAN_POINT('Ctrl Pts',(97.135005412813,0.965486125182712,-0.748084887153543));
#23750=CARTESIAN_POINT('Ctrl Pts',(97.1453438961868,0.958168998467339,-0.748931938084149));
#23751=CARTESIAN_POINT('Ctrl Pts',(97.1497941485706,0.954972458883899,-0.749299542748041));
#23752=CARTESIAN_POINT('Ctrl Pts',(97.1590362122003,0.948235783044142,-0.750069324082935));
#23753=CARTESIAN_POINT('Ctrl Pts',(97.1638237799105,0.94469011636331,-0.750471705422107));
#23754=CARTESIAN_POINT('Ctrl Pts',(97.1762653599038,0.935328895676632,-0.751527024748737));
#23755=CARTESIAN_POINT('Ctrl Pts',(97.1838753052197,0.929455788017907,-0.752182176419098));
#23756=CARTESIAN_POINT('Ctrl Pts',(97.2158650944623,0.904136258982206,-0.754978289253158));
#23757=CARTESIAN_POINT('Ctrl Pts',(97.2395373590085,0.883820332112883,-0.757153190553328));
#23758=CARTESIAN_POINT('Ctrl Pts',(97.3230834137621,0.806153143673275,-0.765233831574081));
#23759=CARTESIAN_POINT('Ctrl Pts',(97.3776590029529,0.743469572574596,-0.771343906035278));
#23760=CARTESIAN_POINT('Ctrl Pts',(97.4550729439242,0.632925465513976,-0.78122276206864));
#23761=CARTESIAN_POINT('Ctrl Pts',(97.4820908520014,0.588321667040079,-0.785001348935371));
#23762=CARTESIAN_POINT('Ctrl Pts',(97.5092707763867,0.535894907652004,-0.789108667124561));
#23763=CARTESIAN_POINT('Ctrl Pts',(97.5124178080195,0.529690763148121,-0.789589615302407));
#23764=CARTESIAN_POINT('Ctrl Pts',(97.5171369422625,0.520179371647318,-0.790318776711186));
#23765=CARTESIAN_POINT('Ctrl Pts',(97.5187488345946,0.51689220348368,-0.790569302008806));
#23766=CARTESIAN_POINT('Ctrl Pts',(97.5216718952282,0.510860149295372,-0.791026257014491));
#23767=CARTESIAN_POINT('Ctrl Pts',(97.5229877632403,0.508117689749636,-0.791232962559423));
#23768=CARTESIAN_POINT('Ctrl Pts',(97.5259347077451,0.50191432424975,-0.791698181688278));
#23769=CARTESIAN_POINT('Ctrl Pts',(97.5275595555245,0.498450548644316,-0.791956316970774));
#23770=CARTESIAN_POINT('Ctrl Pts',(97.5317160450122,0.489476459223481,-0.792621059105246));
#23771=CARTESIAN_POINT('Ctrl Pts',(97.5342220983695,0.48395431916189,-0.793026181248575));
#23772=CARTESIAN_POINT('Ctrl Pts',(97.5507723214078,0.4467240865121,-0.795732877469607));
#23773=CARTESIAN_POINT('Ctrl Pts',(97.5634542240544,0.414425080495898,-0.797961747330944));
#23774=CARTESIAN_POINT('Ctrl Pts',(97.5838553061855,0.354858711720401,-0.801940071729448));
#23775=CARTESIAN_POINT('Ctrl Pts',(97.5920514688766,0.327784886331824,-0.803700672873348));
#23776=CARTESIAN_POINT('Ctrl Pts',(97.611552769411,0.253867706702854,-0.808440303346063));
#23777=CARTESIAN_POINT('Ctrl Pts',(97.6209712296247,0.206584995324231,-0.811402315078615));
#23778=CARTESIAN_POINT('Ctrl Pts',(97.6346252616797,0.106281655342046,-0.817733744051123));
#23779=CARTESIAN_POINT('Ctrl Pts',(97.6382203381726,0.053287107128603,-0.821107559137969));
#23780=CARTESIAN_POINT('Ctrl Pts',(97.6382330599325,-0.0104561322608248,
-0.825297117237775));
#23781=CARTESIAN_POINT('Ctrl Pts',(97.6380896175091,-0.0211465433735564,
-0.826004033500973));
#23782=CARTESIAN_POINT('Ctrl Pts',(97.6376316346255,-0.0380845801419116,
-0.827131542462318));
#23783=CARTESIAN_POINT('Ctrl Pts',(97.6374128209864,-0.0443343892726304,
-0.827549181359122));
#23784=CARTESIAN_POINT('Ctrl Pts',(97.6369112599392,-0.0560019347455081,
-0.828331997261579));
#23785=CARTESIAN_POINT('Ctrl Pts',(97.636640831053,-0.0614200566131054,
-0.828696783700735));
#23786=CARTESIAN_POINT('Ctrl Pts',(97.6359537790895,-0.0735074191600985,
-0.829513507860688));
#23787=CARTESIAN_POINT('Ctrl Pts',(97.6355178116109,-0.0801753283364768,
-0.829966032415147));
#23788=CARTESIAN_POINT('Ctrl Pts',(97.6340645211051,-0.0998318529038032,
-0.831306089108352));
#23789=CARTESIAN_POINT('Ctrl Pts',(97.6328884199717,-0.112807348893192,
-0.832198484732599));
#23790=CARTESIAN_POINT('Ctrl Pts',(97.6297173567158,-0.14233470580817,-0.834247829698772));
#23791=CARTESIAN_POINT('Ctrl Pts',(97.6275857481215,-0.158868768057103,
-0.835408766385599));
#23792=CARTESIAN_POINT('Ctrl Pts',(97.6191843326564,-0.214668073363343,
-0.839372994425729));
#23793=CARTESIAN_POINT('Ctrl Pts',(97.6112780392822,-0.253656121319864,
-0.842222031824925));
#23794=CARTESIAN_POINT('Ctrl Pts',(97.5798595401621,-0.376348045643641,
-0.851415911361136));
#23795=CARTESIAN_POINT('Ctrl Pts',(97.5490532383205,-0.457882691521918,
-0.857892394180007));
#23796=CARTESIAN_POINT('Ctrl Pts',(97.5008638045821,-0.552326488151946,
-0.865449411361776));
#23797=CARTESIAN_POINT('Ctrl Pts',(97.4917545400068,-0.569153686263592,
-0.866797007090072));
#23798=CARTESIAN_POINT('Ctrl Pts',(97.479445922915,-0.590624227565583,-0.868511142747838));
#23799=CARTESIAN_POINT('Ctrl Pts',(97.4766182407359,-0.59547594724229,-0.868898125823845));
#23800=CARTESIAN_POINT('Ctrl Pts',(97.4720376768403,-0.603207604083673,
-0.86951401353318));
#23801=CARTESIAN_POINT('Ctrl Pts',(97.4703069868448,-0.606100487770441,
-0.869744272550769));
#23802=CARTESIAN_POINT('Ctrl Pts',(97.4669616285834,-0.611638215781978,
-0.870184638819007));
#23803=CARTESIAN_POINT('Ctrl Pts',(97.4653489236494,-0.614284151772185,
-0.870394858972442));
#23804=CARTESIAN_POINT('Ctrl Pts',(97.4614662538408,-0.620598171260433,
-0.87089612352806));
#23805=CARTESIAN_POINT('Ctrl Pts',(97.4591865165201,-0.624260251448492,
-0.871186543030097));
#23806=CARTESIAN_POINT('Ctrl Pts',(97.4513063131519,-0.636765040740172,
-0.872177462365222));
#23807=CARTESIAN_POINT('Ctrl Pts',(97.445607923305,-0.645545879421991,-0.872871962075723));
#23808=CARTESIAN_POINT('Ctrl Pts',(97.431356556009,-0.666877995032726,-0.874558952767379));
#23809=CARTESIAN_POINT('Ctrl Pts',(97.4226762372897,-0.679342312322195,
-0.875544470109523));
#23810=CARTESIAN_POINT('Ctrl Pts',(97.3858597484775,-0.73008617064834,-0.879571334097706));
#23811=CARTESIAN_POINT('Ctrl Pts',(97.3556596198792,-0.766816525818167,
-0.882522643548181));
#23812=CARTESIAN_POINT('Ctrl Pts',(97.262815909318,-0.866750201997286,-0.890967695748882));
#23813=CARTESIAN_POINT('Ctrl Pts',(97.195139872809,-0.924808865377008,-0.896431141247991));
#23814=CARTESIAN_POINT('Ctrl Pts',(97.1091212346914,-0.983151824155626,
-0.903209272507031));
#23815=CARTESIAN_POINT('Ctrl Pts',(97.0965010015412,-0.991362793789658,
-0.904199166048572));
#23816=CARTESIAN_POINT('Ctrl Pts',(97.0777877142271,-1.00303360925367,-0.905662273844377));
#23817=CARTESIAN_POINT('Ctrl Pts',(97.0718153383039,-1.00668481889584,-0.906128536172065));
#23818=CARTESIAN_POINT('Ctrl Pts',(97.0611186071721,-1.01309396823462,-0.90696259212058));
#23819=CARTESIAN_POINT('Ctrl Pts',(97.0564068781327,-1.01587266433764,-0.907329626121802));
#23820=CARTESIAN_POINT('Ctrl Pts',(97.0464954663069,-1.02162514036508,-0.9081010588962));
#23821=CARTESIAN_POINT('Ctrl Pts',(97.0412921244421,-1.02459226920312,-0.908505681440112));
#23822=CARTESIAN_POINT('Ctrl Pts',(97.0275510820101,-1.03228958749823,-0.909573379851047));
#23823=CARTESIAN_POINT('Ctrl Pts',(97.0189769697442,-1.03695347681059,-0.910238765731383));
#23824=CARTESIAN_POINT('Ctrl Pts',(96.9782034694051,-1.0584798412583,-0.913399825408443));
#23825=CARTESIAN_POINT('Ctrl Pts',(96.9452958379927,-1.07395075137319,-0.915942825457955));
#23826=CARTESIAN_POINT('Ctrl Pts',(96.8518298193367,-1.11272022504236,-0.923146922954997));
#23827=CARTESIAN_POINT('Ctrl Pts',(96.7899868929997,-1.13257426486221,-0.927898884795009));
#23828=CARTESIAN_POINT('Ctrl Pts',(96.6687688262731,-1.16071712233671,-0.937030744841404));
#23829=CARTESIAN_POINT('Ctrl Pts',(96.6097603389875,-1.16977141667093,-0.941394804668176));
#23830=CARTESIAN_POINT('Ctrl Pts',(96.5403259504138,-1.17508306141429,-0.946278057080083));
#23831=CARTESIAN_POINT('Ctrl Pts',(96.5303272461704,-1.17571975267062,-0.946975085815661));
#23832=CARTESIAN_POINT('Ctrl Pts',(96.5163875633473,-1.17642892978298,-0.947937171859414));
#23833=CARTESIAN_POINT('Ctrl Pts',(96.5124528452229,-1.17660932321249,-0.948207664455452));
#23834=CARTESIAN_POINT('Ctrl Pts',(96.5056623400249,-1.17688651467025,-0.948672543901359));
#23835=CARTESIAN_POINT('Ctrl Pts',(96.5028070003501,-1.17699266451657,-0.948867431213877));
#23836=CARTESIAN_POINT('Ctrl Pts',(96.4967809819985,-1.17719472991313,-0.949277444915885));
#23837=CARTESIAN_POINT('Ctrl Pts',(96.4936102505795,-1.17728822908428,-0.949492430727119));
#23838=CARTESIAN_POINT('Ctrl Pts',(96.4857388045422,-1.17748851831399,-0.950024357127457));
#23839=CARTESIAN_POINT('Ctrl Pts',(96.4810376913323,-1.17757997275575,-0.950340465236844));
#23840=CARTESIAN_POINT('Ctrl Pts',(96.4632871887172,-1.17781895525767,-0.951528498930309));
#23841=CARTESIAN_POINT('Ctrl Pts',(96.4502356311274,-1.1777777526242,-0.952390754216579));
#23842=CARTESIAN_POINT('Ctrl Pts',(96.4166974383298,-1.17711428709309,-0.954583652577698));
#23843=CARTESIAN_POINT('Ctrl Pts',(96.3962209057811,-1.17617421633128,-0.955900644425788));
#23844=CARTESIAN_POINT('Ctrl Pts',(96.3181160470024,-1.17054239801406,-0.960875365005902));
#23845=CARTESIAN_POINT('Ctrl Pts',(96.260834916314,-1.16214436896601,-0.964425195209515));
#23846=CARTESIAN_POINT('Ctrl Pts',(96.1307458494782,-1.13316542289944,-0.972677657563592));
#23847=CARTESIAN_POINT('Ctrl Pts',(96.0588499218609,-1.1097204251828,-0.977390384017675));
#23848=CARTESIAN_POINT('Ctrl Pts',(95.9801727207678,-1.07541015065771,-0.983023647018109));
#23849=CARTESIAN_POINT('Ctrl Pts',(95.9707057633553,-1.07113175780031,-0.983709433781056));
#23850=CARTESIAN_POINT('Ctrl Pts',(95.9552057322682,-1.06387839726196,-0.98484609598705));
#23851=CARTESIAN_POINT('Ctrl Pts',(95.9491392174156,-1.06097592771404,-0.98529451216392));
#23852=CARTESIAN_POINT('Ctrl Pts',(95.9382215580635,-1.05563708563713,-0.986108099131242));
#23853=CARTESIAN_POINT('Ctrl Pts',(95.9333617349143,-1.05321880938616,-0.986472640373134));
#23854=CARTESIAN_POINT('Ctrl Pts',(95.9229669050034,-1.04795631540226,-0.987257597619469));
#23855=CARTESIAN_POINT('Ctrl Pts',(95.9174373965677,-1.04510166207645,-0.987678366856772));
#23856=CARTESIAN_POINT('Ctrl Pts',(95.9023448805737,-1.03715791401725,-0.988835824792488));
#23857=CARTESIAN_POINT('Ctrl Pts',(95.8928292558602,-1.03198059631003,-0.989575572150987));
#23858=CARTESIAN_POINT('Ctrl Pts',(95.8368804603039,-1.00053169979989,-0.99398591923486));
#23859=CARTESIAN_POINT('Ctrl Pts',(95.7922110089307,-0.97126467362705,-0.997762500058218));
#23860=CARTESIAN_POINT('Ctrl Pts',(95.7114429941515,-0.910130414409999,
-1.00508384332328));
#23861=CARTESIAN_POINT('Ctrl Pts',(95.6750076364499,-0.87887796122329,-1.00860611030077));
#23862=CARTESIAN_POINT('Ctrl Pts',(95.6203286827153,-0.825854152109581,
-1.01419435155083));
#23863=CARTESIAN_POINT('Ctrl Pts',(95.6007880204675,-0.805493062599604,
-1.01626050349363));
#23864=CARTESIAN_POINT('Ctrl Pts',(95.558919682293,-0.758605820046568,-1.02081808083479));
#23865=CARTESIAN_POINT('Ctrl Pts',(95.5369916386512,-0.731753713375162,
-1.02329704561381));
#23866=CARTESIAN_POINT('Ctrl Pts',(95.5126536833978,-0.699110360447521,
-1.02612715181856));
#23867=CARTESIAN_POINT('Ctrl Pts',(95.5090671600995,-0.694221598380876,
-1.0265463634253));
#23868=CARTESIAN_POINT('Ctrl Pts',(95.5032793506121,-0.686203175293688,
-1.02722614408863));
#23869=CARTESIAN_POINT('Ctrl Pts',(95.501055332221,-0.68309017314326,-1.02748816292223));
#23870=CARTESIAN_POINT('Ctrl Pts',(95.4970901992691,-0.677482530060515,
-1.02795668665863));
#23871=CARTESIAN_POINT('Ctrl Pts',(95.4953435499329,-0.674991938295483,
-1.02816355531423));
#23872=CARTESIAN_POINT('Ctrl Pts',(95.491515730881,-0.669488517307791,-1.0286179816869));
#23873=CARTESIAN_POINT('Ctrl Pts',(95.4894389510797,-0.66647273606291,-1.02886524777872));
#23874=CARTESIAN_POINT('Ctrl Pts',(95.483456303712,-0.657697747229589,-1.02957980500443));
#23875=CARTESIAN_POINT('Ctrl Pts',(95.4795872886293,-0.65191342755589,-1.03004473398207));
#23876=CARTESIAN_POINT('Ctrl Pts',(95.4471304308481,-0.602446034605347,
-1.03397239308707));
#23877=CARTESIAN_POINT('Ctrl Pts',(95.4214210890852,-0.556934978372629,
-1.03726857012283));
#23878=CARTESIAN_POINT('Ctrl Pts',(95.3627947996074,-0.434859718245381,
-1.04570414474662));
#23879=CARTESIAN_POINT('Ctrl Pts',(95.334825760757,-0.356255333865905,-1.05076727746285));
#23880=CARTESIAN_POINT('Ctrl Pts',(95.3081726300709,-0.245416176256265,
-1.0580384836508));
#23881=CARTESIAN_POINT('Ctrl Pts',(95.3021499059042,-0.215203392687433,
-1.06003091121837));
#23882=CARTESIAN_POINT('Ctrl Pts',(95.2958166060167,-0.175338632095473,
-1.06269108271575));
#23883=CARTESIAN_POINT('Ctrl Pts',(95.2944301970145,-0.165868329187757,
-1.06332528118222));
#23884=CARTESIAN_POINT('Ctrl Pts',(95.2923695648052,-0.150486673043233,
-1.0643594581132));
#23885=CARTESIAN_POINT('Ctrl Pts',(95.2916244217879,-0.144585134941193,
-1.064757221713));
#23886=CARTESIAN_POINT('Ctrl Pts',(95.2902785382022,-0.13323449455988,-1.0655242459885));
#23887=CARTESIAN_POINT('Ctrl Pts',(95.28967107375,-0.12778633358409,-1.06589328701754));
#23888=CARTESIAN_POINT('Ctrl Pts',(95.2883531287802,-0.115166695595001,
-1.0667502294786));
#23889=CARTESIAN_POINT('Ctrl Pts',(95.2876703982411,-0.107992605025229,
-1.06723897819552));
#23890=CARTESIAN_POINT('Ctrl Pts',(95.2857038142906,-0.0851022316291078,
-1.06880373721008));
#23891=CARTESIAN_POINT('Ctrl Pts',(95.2846697774355,-0.0693668014803647,
-1.06988738534283));
#23892=CARTESIAN_POINT('Ctrl Pts',(95.2829814992773,-0.0323198677853692,
-1.07245867997688));
#23893=CARTESIAN_POINT('Ctrl Pts',(95.2825894538957,-0.0110025455210621,
-1.07395381334175));
#23894=CARTESIAN_POINT('Ctrl Pts',(95.2832958240645,0.0696655465751871,
-1.07967091597221));
#23895=CARTESIAN_POINT('Ctrl Pts',(95.2883015500523,0.128888087748305,-1.0839953064675));
#23896=CARTESIAN_POINT('Ctrl Pts',(95.3089594990387,0.257010355248906,-1.09351567142917));
#23897=CARTESIAN_POINT('Ctrl Pts',(95.3263872522775,0.325406276291022,-1.09870646706054));
#23898=CARTESIAN_POINT('Ctrl Pts',(95.3530859251549,0.401082778088738,-1.10433096369587));
#23899=CARTESIAN_POINT('Ctrl Pts',(95.3564623499083,0.410285366747129,-1.10501267081146));
#23900=CARTESIAN_POINT('Ctrl Pts',(95.361341904844,0.423088197630725,-1.1059568866104));
#23901=CARTESIAN_POINT('Ctrl Pts',(95.3627485102137,0.426724448892171,-1.10622458552055));
#23902=CARTESIAN_POINT('Ctrl Pts',(95.3652134909631,0.433003882509279,-1.10668596653439));
#23903=CARTESIAN_POINT('Ctrl Pts',(95.3662634309993,0.435650307751988,-1.10688013221717));
#23904=CARTESIAN_POINT('Ctrl Pts',(95.3685078060775,0.441248062871026,-1.10729020049469));
#23905=CARTESIAN_POINT('Ctrl Pts',(95.3697046331004,0.444198409524226,-1.10750595419461));
#23906=CARTESIAN_POINT('Ctrl Pts',(95.3727200827119,0.451546236355939,-1.10804243420447));
#23907=CARTESIAN_POINT('Ctrl Pts',(95.3745534441821,0.455937673384402,-1.10836229647333));
#23908=CARTESIAN_POINT('Ctrl Pts',(95.3816772124449,0.47271443729813,-1.10958178577495));
#23909=CARTESIAN_POINT('Ctrl Pts',(95.3871535372487,0.485020356737484,-1.11047107029077));
#23910=CARTESIAN_POINT('Ctrl Pts',(95.4018801592111,0.516641006949897,-1.11274934481456));
#23911=CARTESIAN_POINT('Ctrl Pts',(95.41144852683,0.535802809709676,-1.11412330859376));
#23912=CARTESIAN_POINT('Ctrl Pts',(95.4482697276092,0.604769195517504,-1.11908177095763));
#23913=CARTESIAN_POINT('Ctrl Pts',(95.4785915650294,0.652848602089483,-1.12256750481667));
#23914=CARTESIAN_POINT('Ctrl Pts',(95.5567665849524,0.758963043773968,-1.13072926237198));
#23915=CARTESIAN_POINT('Ctrl Pts',(95.606932850112,0.814971171217068,-1.1354167201004));
#23916=CARTESIAN_POINT('Ctrl Pts',(95.6697228026192,0.872871515946718,-1.14102220016301));
#23917=CARTESIAN_POINT('Ctrl Pts',(95.6774578800606,0.87981702172781,-1.14170843478696));
#23918=CARTESIAN_POINT('Ctrl Pts',(95.6903482202763,0.891086919034153,-1.14284568830409));
#23919=CARTESIAN_POINT('Ctrl Pts',(95.6954505060365,0.895471236455041,-1.14329424347457));
#23920=CARTESIAN_POINT('Ctrl Pts',(95.7047373812196,0.903314003893071,-1.14410798187684));
#23921=CARTESIAN_POINT('Ctrl Pts',(95.7089088830186,0.906787713760465,-1.14447253452396));
#23922=CARTESIAN_POINT('Ctrl Pts',(95.7179124988047,0.914180433564817,-1.14525740417223));
#23923=CARTESIAN_POINT('Ctrl Pts',(95.7227519324678,0.918090226473729,-1.14567807361662));
#23924=CARTESIAN_POINT('Ctrl Pts',(95.7360967157749,0.928697875632763,-1.14683496313205));
#23925=CARTESIAN_POINT('Ctrl Pts',(95.744663618575,0.935316950267519,-1.1475742367799));
#23926=CARTESIAN_POINT('Ctrl Pts',(95.7958643740815,0.973760901476376,-1.151973883182));
#23927=CARTESIAN_POINT('Ctrl Pts',(95.8405177347913,1.00278095157837,-1.15573961903063));
#23928=CARTESIAN_POINT('Ctrl Pts',(95.8984801375937,1.03509598674158,-1.16053550934039));
#23929=CARTESIAN_POINT('Ctrl Pts',(95.9100911605651,1.04131626169847,-1.16149161118946));
#23930=CARTESIAN_POINT('Ctrl Pts',(95.921801693794,1.04733935373837,-1.1624507611287));
#23931=CARTESIAN_POINT('Origin',(96.460480949577,-7.19464945638997E-16,
0.924367114736168));
#23932=CARTESIAN_POINT('',(95.9218016575013,1.0473393350719,-1.76247028589786));
#23933=CARTESIAN_POINT('',(95.9218016746715,1.04733934390306,-1.66387871395933));
#23934=CARTESIAN_POINT('',(95.9218016730721,1.04733934308042,0.924367114736168));
#23935=CARTESIAN_POINT('Ctrl Pts',(95.9218016575013,1.04733933507189,-1.76247028589786));
#23936=CARTESIAN_POINT('Ctrl Pts',(95.9082726027725,1.04038092018214,-1.76139659336334));
#23937=CARTESIAN_POINT('Ctrl Pts',(95.8948780141389,1.0331601766951,-1.76031482866298));
#23938=CARTESIAN_POINT('Ctrl Pts',(95.8093131916082,0.984870631619995,-1.75328399601243));
#23939=CARTESIAN_POINT('Ctrl Pts',(95.7415231109389,0.936529175992813,-1.74712890009404));
#23940=CARTESIAN_POINT('Ctrl Pts',(95.6585733912026,0.863025380711787,-1.73905915718277));
#23941=CARTESIAN_POINT('Ctrl Pts',(95.6384167269154,0.843847829252905,-1.73705122289499));
#23942=CARTESIAN_POINT('Ctrl Pts',(95.6113422499949,0.816196661379392,-1.73430698233769));
#23943=CARTESIAN_POINT('Ctrl Pts',(95.6038355698102,0.808314439676538,-1.73354076290774));
#23944=CARTESIAN_POINT('Ctrl Pts',(95.5909225317782,0.794373413556894,-1.73221492723625));
#23945=CARTESIAN_POINT('Ctrl Pts',(95.5854676461171,0.788360761339344,-1.73165233667884));
#23946=CARTESIAN_POINT('Ctrl Pts',(95.5774879563995,0.779380271941437,-1.73082620460101));
#23947=CARTESIAN_POINT('Ctrl Pts',(95.5749151449545,0.776455691633554,-1.73055934831563));
#23948=CARTESIAN_POINT('Ctrl Pts',(95.5703561828224,0.771221266138187,-1.73008568216823));
#23949=CARTESIAN_POINT('Ctrl Pts',(95.5683644381285,0.768916427477689,-1.72987847231106));
#23950=CARTESIAN_POINT('Ctrl Pts',(95.5640341406872,0.763865948753644,-1.72942738408654));
#23951=CARTESIAN_POINT('Ctrl Pts',(95.5616992448567,0.761117282005081,-1.72918376721109));
#23952=CARTESIAN_POINT('Ctrl Pts',(95.5551857309607,0.753377726087125,-1.7285029212196));
#23953=CARTESIAN_POINT('Ctrl Pts',(95.5510357295146,0.748362764626964,-1.72806767741323));
#23954=CARTESIAN_POINT('Ctrl Pts',(95.5266580830309,0.718401940606776,-1.72550052277414));
#23955=CARTESIAN_POINT('Ctrl Pts',(95.5074141246462,0.692669138227843,-1.72343045443746));
#23956=CARTESIAN_POINT('Ctrl Pts',(95.4441108528227,0.600378005131332,-1.71633815159914));
#23957=CARTESIAN_POINT('Ctrl Pts',(95.4057791956269,0.530157979120159,-1.71150037427878));
#23958=CARTESIAN_POINT('Ctrl Pts',(95.3544497619237,0.40811351776157,-1.7032166424801));
#23959=CARTESIAN_POINT('Ctrl Pts',(95.3373313313498,0.358323202982892,-1.6998710901189));
#23960=CARTESIAN_POINT('Ctrl Pts',(95.3207784930459,0.29713628823021,-1.69570479021932));
#23961=CARTESIAN_POINT('Ctrl Pts',(95.3181022006873,0.286674806413331,-1.69499072256259));
#23962=CARTESIAN_POINT('Ctrl Pts',(95.3141126190428,0.270135798081966,-1.69385841661199));
#23963=CARTESIAN_POINT('Ctrl Pts',(95.3127029182374,0.264081970102343,-1.69344324265148));
#23964=CARTESIAN_POINT('Ctrl Pts',(95.3101517426805,0.252719722482748,-1.69266255170987));
#23965=CARTESIAN_POINT('Ctrl Pts',(95.3089989241989,0.247413996999744,-1.69229740472903));
#23966=CARTESIAN_POINT('Ctrl Pts',(95.3064981096364,0.23550805984902,-1.6914766003963));
#23967=CARTESIAN_POINT('Ctrl Pts',(95.3051699807429,0.228903916880639,-1.69102032977696));
#23968=CARTESIAN_POINT('Ctrl Pts',(95.3019310279625,0.212051450239034,-1.68985336781294));
#23969=CARTESIAN_POINT('Ctrl Pts',(95.3000995202083,0.201788663431317,-1.68914022269618));
#23970=CARTESIAN_POINT('Ctrl Pts',(95.2865479733121,0.119555398662598,-1.68340465649594));
#23971=CARTESIAN_POINT('Ctrl Pts',(95.2814007888031,0.0466752038606759,
-1.67817634337518));
#23972=CARTESIAN_POINT('Ctrl Pts',(95.2841857016304,-0.0784783313742113,
-1.66902693684432));
#23973=CARTESIAN_POINT('Ctrl Pts',(95.2888292263588,-0.130620235205284,
-1.66516808325462));
#23974=CARTESIAN_POINT('Ctrl Pts',(95.3008888164893,-0.207600457552029,
-1.65950649273449));
#23975=CARTESIAN_POINT('Ctrl Pts',(95.3056809509799,-0.232785306241036,
-1.65766067802005));
#23976=CARTESIAN_POINT('Ctrl Pts',(95.3135480325982,-0.267854877683472,
-1.65511576133304));
#23977=CARTESIAN_POINT('Ctrl Pts',(95.3159367712923,-0.2778848534677,-1.65439087583065));
#23978=CARTESIAN_POINT('Ctrl Pts',(95.320359592384,-0.295430091095904,-1.65312952485407));
#23979=CARTESIAN_POINT('Ctrl Pts',(95.322337025176,-0.302958847508151,-1.65259044851323));
#23980=CARTESIAN_POINT('Ctrl Pts',(95.3253985707482,-0.314161936595017,
-1.65179208734261));
#23981=CARTESIAN_POINT('Ctrl Pts',(95.3264261532751,-0.317851300390736,
-1.65152979293913));
#23982=CARTESIAN_POINT('Ctrl Pts',(95.3282221754511,-0.324180022176224,
-1.65108099599005));
#23983=CARTESIAN_POINT('Ctrl Pts',(95.3289818765067,-0.326821765720461,
-1.65089400504389));
#23984=CARTESIAN_POINT('Ctrl Pts',(95.330739525683,-0.332854125743456,-1.65046781716339));
#23985=CARTESIAN_POINT('Ctrl Pts',(95.3317434918459,-0.336242927397643,
-1.65022896827799));
#23986=CARTESIAN_POINT('Ctrl Pts',(95.3345477977624,-0.345554510183091,
-1.64957411211087));
#23987=CARTESIAN_POINT('Ctrl Pts',(95.3363796322809,-0.351467799997539,
-1.64915985659529));
#23988=CARTESIAN_POINT('Ctrl Pts',(95.3463556559357,-0.382795082268002,
-1.64697242188612));
#23989=CARTESIAN_POINT('Ctrl Pts',(95.3553159320286,-0.407943354416816,
-1.64524163841597));
#23990=CARTESIAN_POINT('Ctrl Pts',(95.3690877099279,-0.442800441347279,
-1.64284988405034));
#23991=CARTESIAN_POINT('Ctrl Pts',(95.3731893903721,-0.452778655434962,
-1.64216607702972));
#23992=CARTESIAN_POINT('Ctrl Pts',(95.3903670993518,-0.492986998862539,
-1.63940882894324));
#23993=CARTESIAN_POINT('Ctrl Pts',(95.4045718264469,-0.522719735397757,
-1.63736552703426));
#23994=CARTESIAN_POINT('Ctrl Pts',(95.4487989405111,-0.60611169766479,-1.63152284615702));
#23995=CARTESIAN_POINT('Ctrl Pts',(95.4817968221332,-0.658064355163386,
-1.62773934504428));
#23996=CARTESIAN_POINT('Ctrl Pts',(95.5398859289373,-0.73542173191228,-1.62159545349343));
#23997=CARTESIAN_POINT('Ctrl Pts',(95.562331071069,-0.762670792571765,-1.61931956368957));
#23998=CARTESIAN_POINT('Ctrl Pts',(95.5924415416781,-0.79605035915461,-1.6163576280381));
#23999=CARTESIAN_POINT('Ctrl Pts',(95.5990072210361,-0.80315104049503,-1.61571693189914));
#24000=CARTESIAN_POINT('Ctrl Pts',(95.6097665370224,-0.814503344261714,
-1.61467475417947));
#24001=CARTESIAN_POINT('Ctrl Pts',(95.6139064592765,-0.818805434577736,
-1.61427555216223));
#24002=CARTESIAN_POINT('Ctrl Pts',(95.6219056855958,-0.826992487444782,
-1.61350751844035));
#24003=CARTESIAN_POINT('Ctrl Pts',(95.6257597339867,-0.830882385273377,
-1.61313891935744));
#24004=CARTESIAN_POINT('Ctrl Pts',(95.6346304260632,-0.839711579875305,
-1.61229370890543));
#24005=CARTESIAN_POINT('Ctrl Pts',(95.6396644719234,-0.844633015488431,
-1.61181634042057));
#24006=CARTESIAN_POINT('Ctrl Pts',(95.6557588593057,-0.860087608395602,
-1.61029707767412));
#24007=CARTESIAN_POINT('Ctrl Pts',(95.6669797383753,-0.870450530791571,
-1.60924804774239));
#24008=CARTESIAN_POINT('Ctrl Pts',(95.7419014228874,-0.936990924926088,
-1.60230611248537));
#24009=CARTESIAN_POINT('Ctrl Pts',(95.8113073767031,-0.98634534483101,-1.59613743849432));
#24010=CARTESIAN_POINT('Ctrl Pts',(95.907465296868,-1.0401480873461,-1.5880514946744));
#24011=CARTESIAN_POINT('Ctrl Pts',(95.9299225201119,-1.05178046093339,-1.58619477140776));
#24012=CARTESIAN_POINT('Ctrl Pts',(95.9911596053007,-1.0810392498335,-1.58123812175992));
#24013=CARTESIAN_POINT('Ctrl Pts',(96.0305537898655,-1.09730204029909,-1.57815941045678));
#24014=CARTESIAN_POINT('Ctrl Pts',(96.0795967560218,-1.11450000501108,-1.57452214111982));
#24015=CARTESIAN_POINT('Ctrl Pts',(96.0884845569421,-1.11749797661593,-1.57387064391252));
#24016=CARTESIAN_POINT('Ctrl Pts',(96.1013349965504,-1.12166228940029,-1.57294059686305));
#24017=CARTESIAN_POINT('Ctrl Pts',(96.1052691674886,-1.12291437705579,-1.57265745989608));
#24018=CARTESIAN_POINT('Ctrl Pts',(96.1121408584445,-1.12506163059179,-1.57216579236993));
#24019=CARTESIAN_POINT('Ctrl Pts',(96.1150754105119,-1.12596603242809,-1.57195674075906));
#24020=CARTESIAN_POINT('Ctrl Pts',(96.121322380586,-1.12786456946756,-1.57151368939184));
#24021=CARTESIAN_POINT('Ctrl Pts',(96.1246356631346,-1.12885560030019,-1.57127986656484));
#24022=CARTESIAN_POINT('Ctrl Pts',(96.1337182303821,-1.13152874505723,-1.57064195669048));
#24023=CARTESIAN_POINT('Ctrl Pts',(96.1394961973081,-1.13318134830499,-1.57023951345349));
#24024=CARTESIAN_POINT('Ctrl Pts',(96.1677467692998,-1.14102810400831,-1.56828707838497));
#24025=CARTESIAN_POINT('Ctrl Pts',(96.1903889145981,-1.14659884052418,-1.56676916640249));
#24026=CARTESIAN_POINT('Ctrl Pts',(96.3131027410879,-1.17295316159636,-1.55871995838098));
#24027=CARTESIAN_POINT('Ctrl Pts',(96.4153960845011,-1.18131727589625,-1.55260344950045));
#24028=CARTESIAN_POINT('Ctrl Pts',(96.544786846687,-1.17504652183059,-1.54442455462622));
#24029=CARTESIAN_POINT('Ctrl Pts',(96.5720256436124,-1.17277424842285,-1.5426804801343));
#24030=CARTESIAN_POINT('Ctrl Pts',(96.6180475962657,-1.16731726317867,-1.5396770690334));
#24031=CARTESIAN_POINT('Ctrl Pts',(96.6368778088317,-1.16462050617781,-1.53843201620482));
#24032=CARTESIAN_POINT('Ctrl Pts',(96.6632835681097,-1.16018375002331,-1.5366593302508));
#24033=CARTESIAN_POINT('Ctrl Pts',(96.6709204447538,-1.1588228725649,-1.53614348475565));
#24034=CARTESIAN_POINT('Ctrl Pts',(96.6840201268697,-1.15635477280528,-1.53525294770259));
#24035=CARTESIAN_POINT('Ctrl Pts',(96.6894896066919,-1.15528401595648,-1.53487940964032));
#24036=CARTESIAN_POINT('Ctrl Pts',(96.6999278428868,-1.15316349095424,-1.53416315947789));
#24037=CARTESIAN_POINT('Ctrl Pts',(96.7048978247646,-1.15212032414988,-1.53382066310721));
#24038=CARTESIAN_POINT('Ctrl Pts',(96.716531060234,-1.14959992328384,-1.53301546668836));
#24039=CARTESIAN_POINT('Ctrl Pts',(96.7231884695421,-1.14809685930183,-1.5325519597336));
#24040=CARTESIAN_POINT('Ctrl Pts',(96.7428135652766,-1.14348640989986,-1.53117738976875));
#24041=CARTESIAN_POINT('Ctrl Pts',(96.7557415989595,-1.14021664572187,-1.53026123699735));
#24042=CARTESIAN_POINT('Ctrl Pts',(96.8574977933116,-1.11263386075306,-1.52296312473441));
#24043=CARTESIAN_POINT('Ctrl Pts',(96.9432358380313,-1.07820121045382,-1.5162483984759));
#24044=CARTESIAN_POINT('Ctrl Pts',(97.0408942486186,-1.02497928712206,-1.50808646596049));
#24045=CARTESIAN_POINT('Ctrl Pts',(97.0574913531786,-1.0154017595369,-1.50668137412397));
#24046=CARTESIAN_POINT('Ctrl Pts',(97.1007767006911,-0.988995186564692,
-1.50297876588771));
#24047=CARTESIAN_POINT('Ctrl Pts',(97.1270368029671,-0.971490448266343,
-1.50069265679511));
#24048=CARTESIAN_POINT('Ctrl Pts',(97.1667994164849,-0.94261276260187,-1.49719992070009));
#24049=CARTESIAN_POINT('Ctrl Pts',(97.180802411711,-0.931955830433972,-1.49596358878165));
#24050=CARTESIAN_POINT('Ctrl Pts',(97.1986660741304,-0.917717453954565,
-1.49438342389372));
#24051=CARTESIAN_POINT('Ctrl Pts',(97.2027481002315,-0.914418986600052,
-1.49402213507619));
#24052=CARTESIAN_POINT('Ctrl Pts',(97.2093532378976,-0.909008351560454,
-1.49343738256308));
#24053=CARTESIAN_POINT('Ctrl Pts',(97.2118897311067,-0.906912747256671,
-1.49321279052856));
#24054=CARTESIAN_POINT('Ctrl Pts',(97.2168020316673,-0.902819537657584,
-1.49277781856991));
#24055=CARTESIAN_POINT('Ctrl Pts',(97.2191787643677,-0.900823136312687,
-1.49256736238963));
#24056=CARTESIAN_POINT('Ctrl Pts',(97.2249928083513,-0.895900139433797,
-1.49205245605254));
#24057=CARTESIAN_POINT('Ctrl Pts',(97.2284212863593,-0.892963091537648,
-1.49174874993205));
#24058=CARTESIAN_POINT('Ctrl Pts',(97.2382577796243,-0.884437986132794,
-1.49087690510497));
#24059=CARTESIAN_POINT('Ctrl Pts',(97.2446224366942,-0.878800026684242,
-1.49031216970905));
#24060=CARTESIAN_POINT('Ctrl Pts',(97.310874998577,-0.818819058867857,-1.48442008640676));
#24061=CARTESIAN_POINT('Ctrl Pts',(97.3650841664702,-0.758506173936913,
-1.47947184314816));
#24062=CARTESIAN_POINT('Ctrl Pts',(97.4573567282219,-0.631739413014636,
-1.4697676914808));
#24063=CARTESIAN_POINT('Ctrl Pts',(97.4959818821612,-0.566208176884739,
-1.4650380406834));
#24064=CARTESIAN_POINT('Ctrl Pts',(97.5334061731822,-0.4858892882618,-1.45923570442599));
#24065=CARTESIAN_POINT('Ctrl Pts',(97.5385922954742,-0.474270852244039,
-1.45839668752515));
#24066=CARTESIAN_POINT('Ctrl Pts',(97.5461894595004,-0.456482125720178,
-1.45711142742656));
#24067=CARTESIAN_POINT('Ctrl Pts',(97.5487384595379,-0.45037150068393,-1.45666981226544));
#24068=CARTESIAN_POINT('Ctrl Pts',(97.553281064531,-0.439217911759139,-1.45586337669233));
#24069=CARTESIAN_POINT('Ctrl Pts',(97.5552916349992,-0.434182020192706,
-1.45549913372049));
#24070=CARTESIAN_POINT('Ctrl Pts',(97.5595642900659,-0.423261873297295,
-1.45470890712129));
#24071=CARTESIAN_POINT('Ctrl Pts',(97.56181403944,-0.417373004915716,-1.45428252798347));
#24072=CARTESIAN_POINT('Ctrl Pts',(97.5678280870048,-0.401243586871699,
-1.45311389294658));
#24073=CARTESIAN_POINT('Ctrl Pts',(97.5714974544921,-0.390968554613661,
-1.45236855317874));
#24074=CARTESIAN_POINT('Ctrl Pts',(97.5912316150979,-0.333186106953388,
-1.44817098244492));
#24075=CARTESIAN_POINT('Ctrl Pts',(97.6043898405513,-0.284747726472124,
-1.4446260171281));
#24076=CARTESIAN_POINT('Ctrl Pts',(97.6303012100591,-0.157849974318005,
-1.43528344026455));
#24077=CARTESIAN_POINT('Ctrl Pts',(97.6382775717925,-0.0786760906031083,
-1.4293903563793));
#24078=CARTESIAN_POINT('Ctrl Pts',(97.6382104892888,0.0350272723140157,
-1.4211485585674));
#24079=CARTESIAN_POINT('Ctrl Pts',(97.6366890021153,0.0693460825717339,
-1.41869282350173));
#24080=CARTESIAN_POINT('Ctrl Pts',(97.6331377382809,0.10957978262549,-1.41588559547943));
#24081=CARTESIAN_POINT('Ctrl Pts',(97.6325592875135,0.115602968991305,-1.41546725218207));
#24082=CARTESIAN_POINT('Ctrl Pts',(97.6315397229621,0.12542336749079,-1.41478857882479));
#24083=CARTESIAN_POINT('Ctrl Pts',(97.6311265059398,0.129223272826107,-1.41452680681317));
#24084=CARTESIAN_POINT('Ctrl Pts',(97.6303511924804,0.136043860613749,-1.41405852099923));
#24085=CARTESIAN_POINT('Ctrl Pts',(97.6299958862938,0.139065202956841,-1.41385164544526));
#24086=CARTESIAN_POINT('Ctrl Pts',(97.6291866674897,0.145723856763769,-1.41339696022696));
#24087=CARTESIAN_POINT('Ctrl Pts',(97.6287274802272,0.149360443390521,-1.41314944406939));
#24088=CARTESIAN_POINT('Ctrl Pts',(97.6273451445935,0.159911453309238,-1.41243350409842));
#24089=CARTESIAN_POINT('Ctrl Pts',(97.6263775158981,0.166820037671098,-1.41196745620071));
#24090=CARTESIAN_POINT('Ctrl Pts',(97.6175105570039,0.226276885297638,-1.40797696645354));
#24091=CARTESIAN_POINT('Ctrl Pts',(97.6061234777592,0.278250733213789,-1.4046251165657));
#24092=CARTESIAN_POINT('Ctrl Pts',(97.5673210615536,0.411500751045216,-1.39598481583607));
#24093=CARTESIAN_POINT('Ctrl Pts',(97.5344860528934,0.490856783442581,-1.3907739865543));
#24094=CARTESIAN_POINT('Ctrl Pts',(97.4798648457576,0.590540172471542,-1.38350037529658));
#24095=CARTESIAN_POINT('Ctrl Pts',(97.4655184772984,0.614638588035848,-1.3816820400867));
#24096=CARTESIAN_POINT('Ctrl Pts',(97.4453085703628,0.645984041414679,-1.3792223571452));
#24097=CARTESIAN_POINT('Ctrl Pts',(97.4401988256442,0.653707656122043,-1.37860838512267));
#24098=CARTESIAN_POINT('Ctrl Pts',(97.4316959333098,0.666236525985062,-1.37759898411688));
#24099=CARTESIAN_POINT('Ctrl Pts',(97.4283568643858,0.671078135981539,-1.37720557241859));
#24100=CARTESIAN_POINT('Ctrl Pts',(97.4218213238439,0.680404346325787,-1.37644114122446));
#24101=CARTESIAN_POINT('Ctrl Pts',(97.4186293793926,0.684891943571002,-1.3760702993751));
#24102=CARTESIAN_POINT('Ctrl Pts',(97.4110922690535,0.695332654548716,-1.37520033566449));
#24103=CARTESIAN_POINT('Ctrl Pts',(97.4067225023077,0.701267638501984,-1.37470028407919));
#24104=CARTESIAN_POINT('Ctrl Pts',(97.3922771249502,0.720506386248491,-1.37306090191753));
#24105=CARTESIAN_POINT('Ctrl Pts',(97.3819748008172,0.733636557004614,-1.37191287099129));
#24106=CARTESIAN_POINT('Ctrl Pts',(97.3568432121465,0.76430161304173,-1.36915984129998));
#24107=CARTESIAN_POINT('Ctrl Pts',(97.3417736822543,0.781629874074417,-1.36754584094923));
#24108=CARTESIAN_POINT('Ctrl Pts',(97.2801004289617,0.848495038659795,-1.36108127060843));
#24109=CARTESIAN_POINT('Ctrl Pts',(97.229754012008,0.894391964806232,-1.35609610884823));
#24110=CARTESIAN_POINT('Ctrl Pts',(97.155420475941,0.951213972321532,-1.34923074823891));
#24111=CARTESIAN_POINT('Ctrl Pts',(97.134603831427,0.966078344869045,-1.34735692141373));
#24112=CARTESIAN_POINT('Ctrl Pts',(97.100606094342,0.988720474715964,-1.3443877829417));
#24113=CARTESIAN_POINT('Ctrl Pts',(97.0877288751555,0.99693954141716,-1.34328313771873));
#24114=CARTESIAN_POINT('Ctrl Pts',(97.0541122957174,1.01748651272546,-1.34045638416391));
#24115=CARTESIAN_POINT('Ctrl Pts',(97.0331461634347,1.02943271954926,-1.33874775841688));
#24116=CARTESIAN_POINT('Ctrl Pts',(97.0065190053498,1.04353896709603,-1.33665750863426));
#24117=CARTESIAN_POINT('Ctrl Pts',(97.0011902137795,1.04631000646257,-1.3362430900528));
#24118=CARTESIAN_POINT('Ctrl Pts',(96.9927297841228,1.0506276390357,-1.33559153040377));
#24119=CARTESIAN_POINT('Ctrl Pts',(96.9896121540982,1.05220122932029,-1.33535279754543));
#24120=CARTESIAN_POINT('Ctrl Pts',(96.9840220081176,1.05499166628097,-1.33492722710426));
#24121=CARTESIAN_POINT('Ctrl Pts',(96.9815522284154,1.0562136992524,-1.33474007841071));
#24122=CARTESIAN_POINT('Ctrl Pts',(96.9755847900612,1.0591403280166,-1.33428996468118));
#24123=CARTESIAN_POINT('Ctrl Pts',(96.972082946296,1.06083627339469,-1.33402752985998));
#24124=CARTESIAN_POINT('Ctrl Pts',(96.9612690958165,1.06600742760915,-1.33322215745436));
#24125=CARTESIAN_POINT('Ctrl Pts',(96.9539294258324,1.06942471139089,-1.33268259090663));
#24126=CARTESIAN_POINT('Ctrl Pts',(96.9366760735207,1.07724226257554,-1.33142933201042));
#24127=CARTESIAN_POINT('Ctrl Pts',(96.926735547583,1.08158187694978,-1.33071879205294));
#24128=CARTESIAN_POINT('Ctrl Pts',(96.8912332916108,1.09650021404321,-1.32821691596611));
#24129=CARTESIAN_POINT('Ctrl Pts',(96.8653590177299,1.10631562391627,-1.32645862915693));
#24130=CARTESIAN_POINT('Ctrl Pts',(96.7612660731122,1.1416613606516,-1.31955217587822));
#24131=CARTESIAN_POINT('Ctrl Pts',(96.6808140874885,1.15987770949613,-1.31456574919788));
#24132=CARTESIAN_POINT('Ctrl Pts',(96.5576700132021,1.17447497852492,-1.30674391222853));
#24133=CARTESIAN_POINT('Ctrl Pts',(96.5159936281889,1.1771809339213,-1.30406810403586));
#24134=CARTESIAN_POINT('Ctrl Pts',(96.4637210677359,1.1777927434335,-1.3006302448838));
#24135=CARTESIAN_POINT('Ctrl Pts',(96.4531765949774,1.17777454525494,-1.29993268856936));
#24136=CARTESIAN_POINT('Ctrl Pts',(96.4364739489872,1.17752141471837,-1.29882066247037));
#24137=CARTESIAN_POINT('Ctrl Pts',(96.4303147651928,1.17737972510291,-1.29840907199176));
#24138=CARTESIAN_POINT('Ctrl Pts',(96.4192669656823,1.17703882941818,-1.29766793835094));
#24139=CARTESIAN_POINT('Ctrl Pts',(96.4143779094667,1.17685747092942,-1.29733895449875));
#24140=CARTESIAN_POINT('Ctrl Pts',(96.4029369731742,1.17636166995877,-1.29656667264818));
#24141=CARTESIAN_POINT('Ctrl Pts',(96.3963863628969,1.17602294566,-1.29612263405954));
#24142=CARTESIAN_POINT('Ctrl Pts',(96.3774387590434,1.17488441098329,-1.29483268715726));
#24143=CARTESIAN_POINT('Ctrl Pts',(96.3650514766685,1.17394317571243,-1.29398245084462));
#24144=CARTESIAN_POINT('Ctrl Pts',(96.3370586531064,1.17137019941065,-1.29204474471656));
#24145=CARTESIAN_POINT('Ctrl Pts',(96.3214664337683,1.16962221743233,-1.29095388098174));
#24146=CARTESIAN_POINT('Ctrl Pts',(96.2699753536126,1.16280562930156,-1.28731234023861));
#24147=CARTESIAN_POINT('Ctrl Pts',(96.2342783422136,1.15639148583936,-1.28472376420413));
#24148=CARTESIAN_POINT('Ctrl Pts',(96.1317538853162,1.13304070557294,-1.27711687863908));
#24149=CARTESIAN_POINT('Ctrl Pts',(96.0660445827209,1.1118731531171,-1.27201697087281));
#24150=CARTESIAN_POINT('Ctrl Pts',(95.9751778002837,1.07352677021072,-1.26483747684661));
#24151=CARTESIAN_POINT('Ctrl Pts',(95.9482364649276,1.06093558086044,-1.26269341367224));
#24152=CARTESIAN_POINT('Ctrl Pts',(95.9218016672795,1.04733934010109,-1.26059202888093));
#24153=CARTESIAN_POINT('',(97.638230523307,-0.0010337549458608,-1.3257271689311));
#24154=CARTESIAN_POINT('Ctrl Pts',(95.921801693794,1.04733935373837,-1.1624507611287));
#24155=CARTESIAN_POINT('Ctrl Pts',(95.9528161361363,1.0632910475803,-1.16499099562586));
#24156=CARTESIAN_POINT('Ctrl Pts',(95.9845285161482,1.07785965256847,-1.16755324028244));
#24157=CARTESIAN_POINT('Ctrl Pts',(96.0430244658817,1.10164594866506,-1.17218628727739));
#24158=CARTESIAN_POINT('Ctrl Pts',(96.0695787477456,1.11134570458929,-1.17425609947354));
#24159=CARTESIAN_POINT('Ctrl Pts',(96.1294093411433,1.1307905223701,-1.17881737716337));
#24160=CARTESIAN_POINT('Ctrl Pts',(96.1628218594441,1.14004174355271,-1.18129645098146));
#24161=CARTESIAN_POINT('Ctrl Pts',(96.2025058987115,1.1491652176112,-1.18412667177596));
#24162=CARTESIAN_POINT('Ctrl Pts',(96.2084254533261,1.15047809840734,-1.18454589250896));
#24163=CARTESIAN_POINT('Ctrl Pts',(96.2180963958937,1.15254476166447,-1.18522568807064));
#24164=CARTESIAN_POINT('Ctrl Pts',(96.2218416955003,1.15332606272377,-1.1854877126962));
#24165=CARTESIAN_POINT('Ctrl Pts',(96.2285717559479,1.15469582254118,-1.18595624623867));
#24166=CARTESIAN_POINT('Ctrl Pts',(96.2315550407432,1.15529097875302,-1.18616311892203));
#24167=CARTESIAN_POINT('Ctrl Pts',(96.2381343713958,1.15657704867463,-1.18661755383336));
#24168=CARTESIAN_POINT('Ctrl Pts',(96.2417313503988,1.15726275500444,-1.18686482443349));
#24169=CARTESIAN_POINT('Ctrl Pts',(96.2521732574641,1.1592029128502,-1.18757939762913));
#24170=CARTESIAN_POINT('Ctrl Pts',(96.2590263216784,1.16041351527325,-1.18804433798349));
#24171=CARTESIAN_POINT('Ctrl Pts',(96.3173837365965,1.17018984796761,-1.19197238446911));
#24172=CARTESIAN_POINT('Ctrl Pts',(96.3694014869336,1.17538380535976,-1.19526890411557));
#24173=CARTESIAN_POINT('Ctrl Pts',(96.504760152378,1.17985500349988,-1.20370504674461));
#24174=CARTESIAN_POINT('Ctrl Pts',(96.5879746719896,1.17378168149418,-1.20876842550522));
#24175=CARTESIAN_POINT('Ctrl Pts',(96.7001528274863,1.15351654926691,-1.2160394023406));
#24176=CARTESIAN_POINT('Ctrl Pts',(96.7302230259782,1.14685744323325,-1.218031295103));
#24177=CARTESIAN_POINT('Ctrl Pts',(96.7692516028882,1.13659462285538,-1.2206908571464));
#24178=CARTESIAN_POINT('Ctrl Pts',(96.7784770080952,1.13404812549228,-1.2213250014173));
#24179=CARTESIAN_POINT('Ctrl Pts',(96.7933842544064,1.12973706408474,-1.22235911472994));
#24180=CARTESIAN_POINT('Ctrl Pts',(96.799085681049,1.12804134585665,-1.2227568694905));
#24181=CARTESIAN_POINT('Ctrl Pts',(96.8100165216303,1.12469995971626,-1.22352389377642));
#24182=CARTESIAN_POINT('Ctrl Pts',(96.8152477819745,1.12306082132881,-1.22389294377697));
#24183=CARTESIAN_POINT('Ctrl Pts',(96.8273294552255,1.11918237020461,-1.22474993247296));
#24184=CARTESIAN_POINT('Ctrl Pts',(96.8341710770764,1.11691659871585,-1.22523871869568));
#24185=CARTESIAN_POINT('Ctrl Pts',(96.8555493944999,1.10961823342553,-1.22677726528749));
#24186=CARTESIAN_POINT('Ctrl Pts',(96.8700080466943,1.10436371639388,-1.2278341961928));
#24187=CARTESIAN_POINT('Ctrl Pts',(96.903827685184,1.09131762716354,-1.23034642019912));
#24188=CARTESIAN_POINT('Ctrl Pts',(96.9230921722096,1.08329186101098,-1.23180896367419));
#24189=CARTESIAN_POINT('Ctrl Pts',(96.9943087866705,1.05137625952308,-1.23733529804107));
#24190=CARTESIAN_POINT('Ctrl Pts',(97.0447077312792,1.02422749185506,-1.24149411469819));
#24191=CARTESIAN_POINT('Ctrl Pts',(97.1550813148808,0.953967122597752,-1.25108785501892));
#24192=CARTESIAN_POINT('Ctrl Pts',(97.213387325223,0.908656583792617,-1.25652746633866));
#24193=CARTESIAN_POINT('Ctrl Pts',(97.2741068951509,0.851587260583021,-1.26236588064343));
#24194=CARTESIAN_POINT('Ctrl Pts',(97.2810520667816,0.84489709324905,-1.26303635116878));
#24195=CARTESIAN_POINT('Ctrl Pts',(97.2906723862343,0.835399461024587,-1.26396788067598));
#24196=CARTESIAN_POINT('Ctrl Pts',(97.2934168081405,0.832663159724074,-1.26423394827541));
#24197=CARTESIAN_POINT('Ctrl Pts',(97.2983486914858,0.827697085595556,-1.26471259702662));
#24198=CARTESIAN_POINT('Ctrl Pts',(97.3005408791025,0.825472067384314,-1.26492553713432));
#24199=CARTESIAN_POINT('Ctrl Pts',(97.3050023873716,0.820907562370081,-1.26535923921244));
#24200=CARTESIAN_POINT('Ctrl Pts',(97.3072708903037,0.8185673349154,-1.26557993977021));
#24201=CARTESIAN_POINT('Ctrl Pts',(97.3128572014846,0.812756323308112,-1.26612396676726));
#24202=CARTESIAN_POINT('Ctrl Pts',(97.3161635922391,0.809274572018157,-1.26644643787242));
#24203=CARTESIAN_POINT('Ctrl Pts',(97.329275033217,0.795297546468507,-1.26772758310172));
#24204=CARTESIAN_POINT('Ctrl Pts',(97.3389095063395,0.784643016477904,-1.26867438407875));
#24205=CARTESIAN_POINT('Ctrl Pts',(97.3639686342907,0.755890442869172,-1.27116012739227));
#24206=CARTESIAN_POINT('Ctrl Pts',(97.3790447717457,0.737496445865733,-1.27268001000859));
#24207=CARTESIAN_POINT('Ctrl Pts',(97.4307687481324,0.670340284989563,-1.27803514766421));
#24208=CARTESIAN_POINT('Ctrl Pts',(97.464175270021,0.619203451886215,-1.28176759667203));
#24209=CARTESIAN_POINT('Ctrl Pts',(97.5256948141897,0.50686772041217,-1.28971715549704));
#24210=CARTESIAN_POINT('Ctrl Pts',(97.5528273768108,0.445390799849658,-1.29393387011441));
#24211=CARTESIAN_POINT('Ctrl Pts',(97.5779532258167,0.372100858340279,-1.29901855369894));
#24212=CARTESIAN_POINT('Ctrl Pts',(97.5811970405069,0.362213706569555,-1.29970543238965));
#24213=CARTESIAN_POINT('Ctrl Pts',(97.5863224613535,0.345863048827715,-1.3008435313082));
#24214=CARTESIAN_POINT('Ctrl Pts',(97.5882804601208,0.339423951784869,-1.30129228132681));
#24215=CARTESIAN_POINT('Ctrl Pts',(97.5917178923298,0.327761364405649,-1.30210622515762));
#24216=CARTESIAN_POINT('Ctrl Pts',(97.5932166118949,0.32254371839106,-1.30247078687717));
#24217=CARTESIAN_POINT('Ctrl Pts',(97.5963548025454,0.311326727691713,-1.30325551120589));
#24218=CARTESIAN_POINT('Ctrl Pts',(97.5979829254277,0.305324407160047,-1.30367602509131));
#24219=CARTESIAN_POINT('Ctrl Pts',(97.6012142107005,0.293027104562733,-1.30453889150354));
#24220=CARTESIAN_POINT('Ctrl Pts',(97.6028129823224,0.286731200035219,-1.30498136812705));
#24221=CARTESIAN_POINT('Ctrl Pts',(97.6067170486057,0.270806023099641,-1.30610250879798));
#24222=CARTESIAN_POINT('Ctrl Pts',(97.6089531083055,0.261160462460256,-1.30678332619533));
#24223=CARTESIAN_POINT('Ctrl Pts',(97.6292015829024,0.168521420327007,-1.31334017360846));
#24224=CARTESIAN_POINT('Ctrl Pts',(97.6383049869274,0.0838549416170599,
-1.31949861334066));
#24225=CARTESIAN_POINT('Ctrl Pts',(97.6382304961252,-0.00103349190011182,
-1.32572719717278));
#24226=CARTESIAN_POINT('Ctrl Pts',(97.6382304958974,-0.00103375145213981,
-1.32572721621709));
#24227=CARTESIAN_POINT('Ctrl Pts',(97.6381786364634,-0.0601170298897422,
-1.33006237874468));
#24228=CARTESIAN_POINT('Ctrl Pts',(97.6336808842862,-0.119118016426818,
-1.33440949445678));
#24229=CARTESIAN_POINT('Ctrl Pts',(97.6230081894834,-0.189109820144788,
-1.33944026940622));
#24230=CARTESIAN_POINT('Ctrl Pts',(97.6210709776267,-0.200656217023987,
-1.34026582966023));
#24231=CARTESIAN_POINT('Ctrl Pts',(97.6178794232858,-0.218082408309804,
-1.34150336246135));
#24232=CARTESIAN_POINT('Ctrl Pts',(97.6167517628187,-0.223984315984074,
-1.34192101841758));
#24233=CARTESIAN_POINT('Ctrl Pts',(97.6148340636484,-0.233620451222935,
-1.34260024560144));
#24234=CARTESIAN_POINT('Ctrl Pts',(97.6140709690408,-0.237359843235196,
-1.34286316229607));
#24235=CARTESIAN_POINT('Ctrl Pts',(97.6125578758646,-0.244594764189681,
-1.34337047790921));
#24236=CARTESIAN_POINT('Ctrl Pts',(97.6118101124284,-0.248090714007503,
-1.34361499324002));
#24237=CARTESIAN_POINT('Ctrl Pts',(97.6103950753012,-0.254562101861767,
-1.34406639664736));
#24238=CARTESIAN_POINT('Ctrl Pts',(97.6097321669646,-0.257538346506306,
-1.34427351298786));
#24239=CARTESIAN_POINT('Ctrl Pts',(97.6081867961326,-0.264351761467536,
-1.34474656983993));
#24240=CARTESIAN_POINT('Ctrl Pts',(97.6072966450381,-0.268187109635949,
-1.34501207479532));
#24241=CARTESIAN_POINT('Ctrl Pts',(97.6049008192955,-0.278279794426113,
-1.34570885501609));
#24242=CARTESIAN_POINT('Ctrl Pts',(97.6033630352048,-0.284529480149041,
-1.34613839903327));
#24243=CARTESIAN_POINT('Ctrl Pts',(97.5879410279131,-0.345062711105292,
-1.35028298525217));
#24244=CARTESIAN_POINT('Ctrl Pts',(97.570248914536,-0.398310566002967,-1.3538060619574));
#24245=CARTESIAN_POINT('Ctrl Pts',(97.5310509963207,-0.493091224595534,
-1.36018115368523));
#24246=CARTESIAN_POINT('Ctrl Pts',(97.5107410117661,-0.534988787641947,
-1.36303983225609));
#24247=CARTESIAN_POINT('Ctrl Pts',(97.4632903385721,-0.6196984038992,-1.36908574055397));
#24248=CARTESIAN_POINT('Ctrl Pts',(97.4357606536005,-0.662179333190469,
-1.37227423470518));
#24249=CARTESIAN_POINT('Ctrl Pts',(97.3954078520451,-0.716448072030846,
-1.37666795698601));
#24250=CARTESIAN_POINT('Ctrl Pts',(97.384931571883,-0.729915852624672,-1.37778657816324));
#24251=CARTESIAN_POINT('Ctrl Pts',(97.3693669059224,-0.749052232816067,
-1.37942034593786));
#24252=CARTESIAN_POINT('Ctrl Pts',(97.3645099762238,-0.754906910542223,
-1.37992638316302));
#24253=CARTESIAN_POINT('Ctrl Pts',(97.3560145110696,-0.764948012626519,
-1.38080529992986));
#24254=CARTESIAN_POINT('Ctrl Pts',(97.3524024475681,-0.769156590956274,
-1.38117710456824));
#24255=CARTESIAN_POINT('Ctrl Pts',(97.3454059165284,-0.777193007494497,
-1.38189377627657));
#24256=CARTESIAN_POINT('Ctrl Pts',(97.3420259929671,-0.781024649477084,
-1.38223845191753));
#24257=CARTESIAN_POINT('Ctrl Pts',(97.3330949358673,-0.791017489057584,
-1.38314529602009));
#24258=CARTESIAN_POINT('Ctrl Pts',(97.3275035528655,-0.797142168220407,
-1.38370912708849));
#24259=CARTESIAN_POINT('Ctrl Pts',(97.307538749851,-0.818552616224517,-1.38570912013949));
#24260=CARTESIAN_POINT('Ctrl Pts',(97.2928227560247,-0.833512040909031,
-1.3871596543547));
#24261=CARTESIAN_POINT('Ctrl Pts',(97.2139538062443,-0.909513414495519,
-1.39481836081925));
#24262=CARTESIAN_POINT('Ctrl Pts',(97.14347490574,-0.963561214934663,-1.40130969597968));
#24263=CARTESIAN_POINT('Ctrl Pts',(97.0324279018609,-1.03036827166546,-1.41081360125513));
#24264=CARTESIAN_POINT('Ctrl Pts',(96.9961468498718,-1.04968784255756,-1.41381413822792));
#24265=CARTESIAN_POINT('Ctrl Pts',(96.9463017429934,-1.07297131382178,-1.41774261419488));
#24266=CARTESIAN_POINT('Ctrl Pts',(96.9335707525378,-1.07864514960123,-1.4187296361128));
#24267=CARTESIAN_POINT('Ctrl Pts',(96.9117953508952,-1.08789008298886,-1.42038692295335));
#24268=CARTESIAN_POINT('Ctrl Pts',(96.902802193782,-1.09157750695109,-1.42106257706736));
#24269=CARTESIAN_POINT('Ctrl Pts',(96.8900232754545,-1.09663331914765,-1.42200926786348));
#24270=CARTESIAN_POINT('Ctrl Pts',(96.8862748588287,-1.09809416464252,-1.42228534479176));
#24271=CARTESIAN_POINT('Ctrl Pts',(96.8796138040812,-1.10065089658564,-1.42277299342649));
#24272=CARTESIAN_POINT('Ctrl Pts',(96.8767041808321,-1.10175449559545,-1.42298500975249));
#24273=CARTESIAN_POINT('Ctrl Pts',(96.8710488184689,-1.10387393202832,-1.4233951350146));
#24274=CARTESIAN_POINT('Ctrl Pts',(96.8683036414395,-1.10489107393181,-1.4235933252255));
#24275=CARTESIAN_POINT('Ctrl Pts',(96.860795808329,-1.10764107970035,-1.42413300806459));
#24276=CARTESIAN_POINT('Ctrl Pts',(96.8560256451163,-1.10935348006256,-1.42447332375885));
#24277=CARTESIAN_POINT('Ctrl Pts',(96.8435545320998,-1.1137397106476,-1.42535670886852));
#24278=CARTESIAN_POINT('Ctrl Pts',(96.8358364694029,-1.11636452610495,-1.42589714475116));
#24279=CARTESIAN_POINT('Ctrl Pts',(96.7611920487,-1.14088848339568,-1.43106935529451));
#24280=CARTESIAN_POINT('Ctrl Pts',(96.6924464063933,-1.15682690149822,-1.43541727252204));
#24281=CARTESIAN_POINT('Ctrl Pts',(96.5638863914899,-1.17470249364689,-1.44344613274062));
#24282=CARTESIAN_POINT('Ctrl Pts',(96.5045624191325,-1.17842046800066,-1.44711303053659));
#24283=CARTESIAN_POINT('Ctrl Pts',(96.4238955017707,-1.17737466057927,-1.45225418597847));
#24284=CARTESIAN_POINT('Ctrl Pts',(96.4025901999534,-1.17651951366322,-1.45362612777498));
#24285=CARTESIAN_POINT('Ctrl Pts',(96.3655870892173,-1.17402678389165,-1.45604181904048));
#24286=CARTESIAN_POINT('Ctrl Pts',(96.3498769422466,-1.17265103478291,-1.45707777184707));
#24287=CARTESIAN_POINT('Ctrl Pts',(96.3270345783134,-1.1701876195918,-1.4586013034187));
#24288=CARTESIAN_POINT('Ctrl Pts',(96.3198768029197,-1.16934916476345,-1.45908118563653));
#24289=CARTESIAN_POINT('Ctrl Pts',(96.3072885966879,-1.1677573455315,-1.45992970942614));
#24290=CARTESIAN_POINT('Ctrl Pts',(96.301854837416,-1.16703164902894,-1.46029748101796));
#24291=CARTESIAN_POINT('Ctrl Pts',(96.2905359930017,-1.16543946986313,-1.46106679832068));
#24292=CARTESIAN_POINT('Ctrl Pts',(96.2846520232026,-1.16456628518632,-1.46146854326036));
#24293=CARTESIAN_POINT('Ctrl Pts',(96.2693186064281,-1.16217194301288,-1.46252036783486));
#24294=CARTESIAN_POINT('Ctrl Pts',(96.2598808022519,-1.1605801299703,-1.46317263431387));
#24295=CARTESIAN_POINT('Ctrl Pts',(96.2201611560394,-1.15338192286718,-1.46593895809901));
#24296=CARTESIAN_POINT('Ctrl Pts',(96.1900883345962,-1.14670440636737,-1.46808605790689));
#24297=CARTESIAN_POINT('Ctrl Pts',(96.0798497808304,-1.11764897403433,-1.47615827416963));
#24298=CARTESIAN_POINT('Ctrl Pts',(96.0018679202524,-1.08797519369787,-1.48229136440521));
#24299=CARTESIAN_POINT('Ctrl Pts',(95.8811166873791,-1.02672181671144,-1.49220296594283));
#24300=CARTESIAN_POINT('Ctrl Pts',(95.836173526215,-1.00003108995239,-1.4959907504425));
#24301=CARTESIAN_POINT('Ctrl Pts',(95.7874118429878,-0.966499593404055,
-1.50010675487966));
#24302=CARTESIAN_POINT('Ctrl Pts',(95.7817128786653,-0.962505791181802,
-1.50058786974931));
#24303=CARTESIAN_POINT('Ctrl Pts',(95.7730696027791,-0.956333681544294,
-1.5013172390303));
#24304=CARTESIAN_POINT('Ctrl Pts',(95.7700996157875,-0.954191849176072,
-1.50156780715301));
#24305=CARTESIAN_POINT('Ctrl Pts',(95.7646805524564,-0.950245296786186,
-1.50202482057208));
#24306=CARTESIAN_POINT('Ctrl Pts',(95.7622284695233,-0.948444933163378,
-1.50223154189108));
#24307=CARTESIAN_POINT('Ctrl Pts',(95.7567082401577,-0.94435886866627,-1.50269677367462));
#24308=CARTESIAN_POINT('Ctrl Pts',(95.7536442370983,-0.942067705781955,
-1.50295490599978));
#24309=CARTESIAN_POINT('Ctrl Pts',(95.7457534361408,-0.936107048239926,
-1.50361959221005));
#24310=CARTESIAN_POINT('Ctrl Pts',(95.7409436404996,-0.93241508401061,-1.50402466216824));
#24311=CARTESIAN_POINT('Ctrl Pts',(95.7088402568908,-0.907376401805629,
-1.50672937877678));
#24312=CARTESIAN_POINT('Ctrl Pts',(95.682468815932,-0.884869081143158,-1.50895645400073));
#24313=CARTESIAN_POINT('Ctrl Pts',(95.636504489084,-0.841993531899366,-1.51292823667213));
#24314=CARTESIAN_POINT('Ctrl Pts',(95.6165798026714,-0.822022682303489,
-1.51468418008077));
#24315=CARTESIAN_POINT('Ctrl Pts',(95.5647670924743,-0.766218396758312,
-1.51940558532152));
#24316=CARTESIAN_POINT('Ctrl Pts',(95.5343202578391,-0.729122915702506,
-1.52235409159086));
#24317=CARTESIAN_POINT('Ctrl Pts',(95.4749438125358,-0.647038776814336,
-1.52868927915255));
#24318=CARTESIAN_POINT('Ctrl Pts',(95.4466464945641,-0.601731866680707,
-1.53208141320341));
#24319=CARTESIAN_POINT('Ctrl Pts',(95.4164179239082,-0.545109917806109,
-1.53629994721787));
#24320=CARTESIAN_POINT('Ctrl Pts',(95.411448153655,-0.535483523891176,-1.5370163018179));
#24321=CARTESIAN_POINT('Ctrl Pts',(95.4038338185561,-0.520221711805234,
-1.53815139336462));
#24322=CARTESIAN_POINT('Ctrl Pts',(95.4010998453958,-0.514631385095465,
-1.53856703979477));
#24323=CARTESIAN_POINT('Ctrl Pts',(95.396064269581,-0.504124647180466,-1.53934811221355));
#24324=CARTESIAN_POINT('Ctrl Pts',(95.3937520961522,-0.499213461487374,
-1.53971316411224));
#24325=CARTESIAN_POINT('Ctrl Pts',(95.3886516271823,-0.488182538277522,
-1.54053308832544));
#24326=CARTESIAN_POINT('Ctrl Pts',(95.3858816495482,-0.482054590434231,
-1.54098856841987));
#24327=CARTESIAN_POINT('Ctrl Pts',(95.3789667575312,-0.466401143769895,
-1.54215220981922));
#24328=CARTESIAN_POINT('Ctrl Pts',(95.374895185102,-0.456844076785939,-1.54286280127476));
#24329=CARTESIAN_POINT('Ctrl Pts',(95.3422954176212,-0.377426185720986,
-1.54877035576747));
#24330=CARTESIAN_POINT('Ctrl Pts',(95.320420827739,-0.305038435815673,-1.55418894460636));
#24331=CARTESIAN_POINT('Ctrl Pts',(95.2942797097766,-0.174387896560006,
-1.56393571869398));
#24332=CARTESIAN_POINT('Ctrl Pts',(95.2871268082519,-0.11694776599024,-1.56820505755745));
#24333=CARTESIAN_POINT('Ctrl Pts',(95.2831896174929,-0.0387369023930222,
-1.57386002803975));
#24334=CARTESIAN_POINT('Ctrl Pts',(95.2826936169924,-0.0182353273264383,
-1.57532720582229));
#24335=CARTESIAN_POINT('Ctrl Pts',(95.2827582967303,0.0153242075192261,
-1.57769401404468));
#24336=CARTESIAN_POINT('Ctrl Pts',(95.2830005001584,0.0283778963087294,
-1.57860598951886));
#24337=CARTESIAN_POINT('Ctrl Pts',(95.2836251139981,0.0461250198445256,
-1.57983177549765));
#24338=CARTESIAN_POINT('Ctrl Pts',(95.2838186617399,0.0508235915674019,
-1.58015495859122));
#24339=CARTESIAN_POINT('Ctrl Pts',(95.2841898885381,0.0586895604090173,
-1.5806936144164));
#24340=CARTESIAN_POINT('Ctrl Pts',(95.2843522301988,0.0618575865423896,
-1.58090990848106));
#24341=CARTESIAN_POINT('Ctrl Pts',(95.2846851081383,0.0678775653389548,
-1.58131963338843));
#24342=CARTESIAN_POINT('Ctrl Pts',(95.2848532245011,0.070729605518265,-1.5815131999688));
#24343=CARTESIAN_POINT('Ctrl Pts',(95.2852777492193,0.077511342003848,-1.58197223505135));
#24344=CARTESIAN_POINT('Ctrl Pts',(95.2855434940812,0.0814404509278922,
-1.58223719526481));
#24345=CARTESIAN_POINT('Ctrl Pts',(95.2865548293043,0.0953562489598012,
-1.58317233856358));
#24346=CARTESIAN_POINT('Ctrl Pts',(95.2874081042898,0.105335018066843,-1.58383694081671));
#24347=CARTESIAN_POINT('Ctrl Pts',(95.2945024366643,0.177451774578565,-1.58860464650549));
#24348=CARTESIAN_POINT('Ctrl Pts',(95.305550661497,0.239025319525307,-1.59248803843815));
#24349=CARTESIAN_POINT('Ctrl Pts',(95.3373896729268,0.360139172666509,-1.60024199521176));
#24350=CARTESIAN_POINT('Ctrl Pts',(95.3581724698459,0.419463596016934,-1.60410200588416));
#24351=CARTESIAN_POINT('Ctrl Pts',(95.393159674064,0.498477605156671,-1.60958774454999));
#24352=CARTESIAN_POINT('Ctrl Pts',(95.4033861410053,0.519812549143089,-1.61110491782931));
#24353=CARTESIAN_POINT('Ctrl Pts',(95.4220860185346,0.555987775463909,-1.6137518872214));
#24354=CARTESIAN_POINT('Ctrl Pts',(95.4302528622754,0.570978527913612,-1.61487160911008));
#24355=CARTESIAN_POINT('Ctrl Pts',(95.4424405707272,0.592236555563929,-1.61649540078107));
#24356=CARTESIAN_POINT('Ctrl Pts',(95.4461998028688,0.598651903793953,-1.61699023940071));
#24357=CARTESIAN_POINT('Ctrl Pts',(95.4528537103137,0.609764584079147,-1.61785603579512));
#24358=CARTESIAN_POINT('Ctrl Pts',(95.4557211455949,0.614478019005303,-1.61822600723145));
#24359=CARTESIAN_POINT('Ctrl Pts',(95.4617002350169,0.624152577886072,-1.61899116705584));
#24360=CARTESIAN_POINT('Ctrl Pts',(95.4648159811583,0.629110979707698,-1.61938649674319));
#24361=CARTESIAN_POINT('Ctrl Pts',(95.4728919091673,0.64175274481016,-1.62040269392431));
#24362=CARTESIAN_POINT('Ctrl Pts',(95.477904764649,0.649401825407263,-1.62102548029165));
#24363=CARTESIAN_POINT('Ctrl Pts',(95.4981121723117,0.679466493345246,-1.62350551178803));
#24364=CARTESIAN_POINT('Ctrl Pts',(95.5139877537221,0.701412006233222,-1.62538783303082));
#24365=CARTESIAN_POINT('Ctrl Pts',(95.5902907372503,0.799576625296967,-1.63415234517379));
#24366=CARTESIAN_POINT('Ctrl Pts',(95.6592533348924,0.868667149739692,-1.64135766762612));
#24367=CARTESIAN_POINT('Ctrl Pts',(95.7590107633359,0.946516656059798,-1.65058278238766));
#24368=CARTESIAN_POINT('Ctrl Pts',(95.7827850247087,0.963681828214781,-1.65270231931335));
#24369=CARTESIAN_POINT('Ctrl Pts',(95.821115308615,0.989235707126706,-1.65597216811415));
#24370=CARTESIAN_POINT('Ctrl Pts',(95.8352517222745,0.998230530375245,-1.65714818706774));
#24371=CARTESIAN_POINT('Ctrl Pts',(95.8539854918529,1.00959641523064,-1.65866339181127));
#24372=CARTESIAN_POINT('Ctrl Pts',(95.858412506144,1.01224268521555,-1.65901835712953));
#24373=CARTESIAN_POINT('Ctrl Pts',(95.8656746143812,1.01651914842308,-1.65959542884377));
#24374=CARTESIAN_POINT('Ctrl Pts',(95.8684993084213,1.01816673128626,-1.65981861040835));
#24375=CARTESIAN_POINT('Ctrl Pts',(95.8740290684058,1.02136132862835,-1.66025297676189));
#24376=CARTESIAN_POINT('Ctrl Pts',(95.8767334615111,1.0229094012002,-1.66046422430594));
#24377=CARTESIAN_POINT('Ctrl Pts',(95.88279073516,1.02634491396403,-1.66093480469614));
#24378=CARTESIAN_POINT('Ctrl Pts',(95.8861468167274,1.02822671193159,-1.6611937849441));
#24379=CARTESIAN_POINT('Ctrl Pts',(95.8978045097898,1.03468844445868,-1.6620875523738));
#24380=CARTESIAN_POINT('Ctrl Pts',(95.906152423961,1.03918470573194,-1.66271738188609));
#24381=CARTESIAN_POINT('Ctrl Pts',(95.9169657544763,1.04484147278675,-1.663521385413));
#24382=CARTESIAN_POINT('Ctrl Pts',(95.9193816458742,1.04609464764928,-1.66370026126829));
#24383=CARTESIAN_POINT('Ctrl Pts',(95.9218016746715,1.04733934390307,-1.66387871395933));
#24384=CARTESIAN_POINT('Origin',(96.460480949577,-7.19464945638997E-16,
0.924367114736168));
#24385=CARTESIAN_POINT('',(95.9218015453622,1.04733927739526,-2.26182855819541));
#24386=CARTESIAN_POINT('',(95.9218016761257,1.04733934465099,-2.16205147885552));
#24387=CARTESIAN_POINT('',(95.9218016730721,1.04733934308042,0.924367114736168));
#24388=CARTESIAN_POINT('',(97.6382305799192,0.000395899098767113,-1.92539805293419));
#24389=CARTESIAN_POINT('Ctrl Pts',(95.9218015453623,1.04733927739527,-2.26182855819541));
#24390=CARTESIAN_POINT('Ctrl Pts',(95.9005594358515,1.03641379494418,-2.26034392312565));
#24391=CARTESIAN_POINT('Ctrl Pts',(95.8796424425559,1.02483833332954,-2.25885102568976));
#24392=CARTESIAN_POINT('Ctrl Pts',(95.8233247093762,0.991391149828253,-2.25471890233259));
#24393=CARTESIAN_POINT('Ctrl Pts',(95.7887222002028,0.968278933968751,-2.25205254613741));
#24394=CARTESIAN_POINT('Ctrl Pts',(95.7470775398636,0.937154749242537,-2.24863341212708));
#24395=CARTESIAN_POINT('Ctrl Pts',(95.7388215705449,0.930812106880061,-2.24794471874761));
#24396=CARTESIAN_POINT('Ctrl Pts',(95.7257922833405,0.920524822855528,-2.24683974067127));
#24397=CARTESIAN_POINT('Ctrl Pts',(95.7209639871069,0.916650448938913,-2.24642621059659));
#24398=CARTESIAN_POINT('Ctrl Pts',(95.7119966644007,0.90933782943845,-2.24565042748322));
#24399=CARTESIAN_POINT('Ctrl Pts',(95.7078502044114,0.905908920912824,-2.24528855275363));
#24400=CARTESIAN_POINT('Ctrl Pts',(95.6985575877115,0.898116570660832,-2.24447031584675));
#24401=CARTESIAN_POINT('Ctrl Pts',(95.6934251746797,0.893737108311844,-2.24401331385242));
#24402=CARTESIAN_POINT('Ctrl Pts',(95.678251952764,0.880562900034642,-2.2426468162873));
#24403=CARTESIAN_POINT('Ctrl Pts',(95.6683230107008,0.871641554117464,-2.2417321646485));
#24404=CARTESIAN_POINT('Ctrl Pts',(95.645956617397,0.850847087847731,-2.23962346779264));
#24405=CARTESIAN_POINT('Ctrl Pts',(95.6336235012992,0.838866713085102,-2.23842509959699));
#24406=CARTESIAN_POINT('Ctrl Pts',(95.5922893391359,0.796917395141394,-2.23428343663299));
#24407=CARTESIAN_POINT('Ctrl Pts',(95.5646221749364,0.765682995937537,-2.23128976342374));
#24408=CARTESIAN_POINT('Ctrl Pts',(95.4992507602404,0.683478555557929,-2.22365264124503));
#24409=CARTESIAN_POINT('Ctrl Pts',(95.4638940352677,0.630809525430696,-2.21896744349422));
#24410=CARTESIAN_POINT('Ctrl Pts',(95.4264117929955,0.563892458077927,-2.21339450110199));
#24411=CARTESIAN_POINT('Ctrl Pts',(95.4200785450134,0.552120079552428,-2.21242771296679));
#24412=CARTESIAN_POINT('Ctrl Pts',(95.402353501441,0.517783878816849,-2.20965153540369));
#24413=CARTESIAN_POINT('Ctrl Pts',(95.3914850024866,0.494956285895658,-2.20785925717368));
#24414=CARTESIAN_POINT('Ctrl Pts',(95.3789180781401,0.46621233145495,-2.20568251341245));
#24415=CARTESIAN_POINT('Ctrl Pts',(95.3765207132462,0.46061089099608,-2.20526202261331));
#24416=CARTESIAN_POINT('Ctrl Pts',(95.3728100856315,0.451751578409685,-2.20460306201076));
#24417=CARTESIAN_POINT('Ctrl Pts',(95.3714677835833,0.448506100267409,-2.20436294159042));
#24418=CARTESIAN_POINT('Ctrl Pts',(95.3690995194883,0.442706687409642,-2.2039362060559));
#24419=CARTESIAN_POINT('Ctrl Pts',(95.3680679932508,0.440155165943464,-2.20374926875774));
#24420=CARTESIAN_POINT('Ctrl Pts',(95.3656107301693,0.434015177297052,-2.2033013401377));
#24421=CARTESIAN_POINT('Ctrl Pts',(95.3641936855554,0.430423288490405,-2.20304086445674));
#24422=CARTESIAN_POINT('Ctrl Pts',(95.3599154471199,0.419420719667989,-2.20224755909827));
#24423=CARTESIAN_POINT('Ctrl Pts',(95.357111470279,0.411987822499146,-2.20171795614181));
#24424=CARTESIAN_POINT('Ctrl Pts',(95.3507476502651,0.394587224893803,-2.20049156483722));
#24425=CARTESIAN_POINT('Ctrl Pts',(95.3472464837898,0.384598641450425,-2.19979774640875));
#24426=CARTESIAN_POINT('Ctrl Pts',(95.3354019767762,0.349289349370133,-2.19737626073909));
#24427=CARTESIAN_POINT('Ctrl Pts',(95.3277836407308,0.323732518242791,-2.19567939298498));
#24428=CARTESIAN_POINT('Ctrl Pts',(95.3012415214691,0.222223958700894,-2.18907884191828));
#24429=CARTESIAN_POINT('Ctrl Pts',(95.2890395472296,0.144724961393674,-2.18432873531507));
#24430=CARTESIAN_POINT('Ctrl Pts',(95.2819767318031,0.0200009348604612,
-2.1764817983415));
#24431=CARTESIAN_POINT('Ctrl Pts',(95.2821096897527,-0.0266951193868056,
-2.17350215372494));
#24432=CARTESIAN_POINT('Ctrl Pts',(95.2856790785276,-0.0839692340116455,
-2.16973079514788));
#24433=CARTESIAN_POINT('Ctrl Pts',(95.2864930952421,-0.0946719278948646,
-2.16902113109647));
#24434=CARTESIAN_POINT('Ctrl Pts',(95.2880136276566,-0.111600530014013,
-2.16789016987684));
#24435=CARTESIAN_POINT('Ctrl Pts',(95.2886237534646,-0.117834666523381,
-2.16747185785962));
#24436=CARTESIAN_POINT('Ctrl Pts',(95.2898550552628,-0.129458528349032,
-2.16668835411016));
#24437=CARTESIAN_POINT('Ctrl Pts',(95.2904638019322,-0.13484942540551,-2.16632355785077));
#24438=CARTESIAN_POINT('Ctrl Pts',(95.2919041485002,-0.146859904881965,
-2.16550755293036));
#24439=CARTESIAN_POINT('Ctrl Pts',(95.2927547883248,-0.153476971686341,
-2.16505576317506));
#24440=CARTESIAN_POINT('Ctrl Pts',(95.2954248036017,-0.172937879822967,
-2.16372031209844));
#24441=CARTESIAN_POINT('Ctrl Pts',(95.2974001597513,-0.185758947520191,
-2.16283183907709));
#24442=CARTESIAN_POINT('Ctrl Pts',(95.3124385354089,-0.273688736979836,
-2.15667649584193));
#24443=CARTESIAN_POINT('Ctrl Pts',(95.3325534937224,-0.347394090762805,
-2.15118695028902));
#24444=CARTESIAN_POINT('Ctrl Pts',(95.3880866840082,-0.493426418705865,
-2.1397466839498));
#24445=CARTESIAN_POINT('Ctrl Pts',(95.4240827137434,-0.565136902108412,
-2.13381739521637));
#24446=CARTESIAN_POINT('Ctrl Pts',(95.4721789399126,-0.640659385052763,
-2.12754924634726));
#24447=CARTESIAN_POINT('Ctrl Pts',(95.4773789069225,-0.648610590424305,
-2.12688922290188));
#24448=CARTESIAN_POINT('Ctrl Pts',(95.484758562989,-0.65960204850743,-2.12597762413243));
#24449=CARTESIAN_POINT('Ctrl Pts',(95.4868572101564,-0.66269589788906,-2.12572111862893));
#24450=CARTESIAN_POINT('Ctrl Pts',(95.4907165276595,-0.668327440321926,
-2.1252544565966));
#24451=CARTESIAN_POINT('Ctrl Pts',(95.4924725162134,-0.67086829953477,-2.1250439969197));
#24452=CARTESIAN_POINT('Ctrl Pts',(95.4961355750922,-0.67612430022902,-2.12460887308832));
#24453=CARTESIAN_POINT('Ctrl Pts',(95.4980441480668,-0.678838327172358,
-2.12438431187135));
#24454=CARTESIAN_POINT('Ctrl Pts',(95.5030737313303,-0.685926639747509,
-2.12379803607577));
#24455=CARTESIAN_POINT('Ctrl Pts',(95.506213297219,-0.690287756717486,-2.1234375461586));
#24456=CARTESIAN_POINT('Ctrl Pts',(95.5204915848825,-0.709837886752784,
-2.12182176509973));
#24457=CARTESIAN_POINT('Ctrl Pts',(95.5319645517462,-0.724780813459593,
-2.12058738963753));
#24458=CARTESIAN_POINT('Ctrl Pts',(95.5657811065641,-0.76670326749975,-2.11710557389248));
#24459=CARTESIAN_POINT('Ctrl Pts',(95.5889771512939,-0.792971124343236,
-2.11490053461892));
#24460=CARTESIAN_POINT('Ctrl Pts',(95.6690318115688,-0.875863529872492,
-2.10771720322605));
#24461=CARTESIAN_POINT('Ctrl Pts',(95.7304982371159,-0.927714227479524,
-2.10283547142644));
#24462=CARTESIAN_POINT('Ctrl Pts',(95.8250614602941,-0.99222534983343,-2.09556207790121));
#24463=CARTESIAN_POINT('Ctrl Pts',(95.8541929099756,-1.01028884117017,-2.09335203219231));
#24464=CARTESIAN_POINT('Ctrl Pts',(95.8927337380447,-1.03191904141595,-2.0904417659188));
#24465=CARTESIAN_POINT('Ctrl Pts',(95.9014601672429,-1.03667234902755,-2.08978374278048));
#24466=CARTESIAN_POINT('Ctrl Pts',(95.9155756555645,-1.04413103890086,-2.08872028685138));
#24467=CARTESIAN_POINT('Ctrl Pts',(95.9209272886428,-1.04690651470306,-2.08831731030366));
#24468=CARTESIAN_POINT('Ctrl Pts',(95.9311664056757,-1.05211738539997,-2.08754659256149));
#24469=CARTESIAN_POINT('Ctrl Pts',(95.9360499934765,-1.05456012138142,-2.08717911799213));
#24470=CARTESIAN_POINT('Ctrl Pts',(95.9472705941701,-1.06007537014422,-2.08633498867518));
#24471=CARTESIAN_POINT('Ctrl Pts',(95.9536184820173,-1.06312515469032,-2.0858575688254));
#24472=CARTESIAN_POINT('Ctrl Pts',(95.9734589309661,-1.07243923000943,-2.08436556910142));
#24473=CARTESIAN_POINT('Ctrl Pts',(95.9870426337823,-1.07850474024511,-2.08334432002806));
#24474=CARTESIAN_POINT('Ctrl Pts',(96.0189326617879,-1.09202599401455,-2.08094626354754));
#24475=CARTESIAN_POINT('Ctrl Pts',(96.0373186052977,-1.09928122599583,-2.07956326888352));
#24476=CARTESIAN_POINT('Ctrl Pts',(96.1048444589781,-1.12398236757368,-2.07448175662579));
#24477=CARTESIAN_POINT('Ctrl Pts',(96.1549417252228,-1.13862127031158,-2.07070424602856));
#24478=CARTESIAN_POINT('Ctrl Pts',(96.2854227773387,-1.16751612461275,-2.06092205002118));
#24479=CARTESIAN_POINT('Ctrl Pts',(96.3666263727511,-1.17683155982532,-2.05487788752936));
#24480=CARTESIAN_POINT('Ctrl Pts',(96.4575079124201,-1.17778346188621,-2.04851729712666));
#24481=CARTESIAN_POINT('Ctrl Pts',(96.4668712744328,-1.17776988394416,-2.04786696012004));
#24482=CARTESIAN_POINT('Ctrl Pts',(96.4803148424791,-1.17759005463347,-2.04694130317679));
#24483=CARTESIAN_POINT('Ctrl Pts',(96.4843956128269,-1.17751425053449,-2.04666139026731));
#24484=CARTESIAN_POINT('Ctrl Pts',(96.4915492608569,-1.17734416077578,-2.04617266734272));
#24485=CARTESIAN_POINT('Ctrl Pts',(96.4946222842756,-1.17725905519267,-2.04596336434827));
#24486=CARTESIAN_POINT('Ctrl Pts',(96.5011385281733,-1.17705305456441,-2.04552093061628));
#24487=CARTESIAN_POINT('Ctrl Pts',(96.5045815769757,-1.17692908341408,-2.04528796897155));
#24488=CARTESIAN_POINT('Ctrl Pts',(96.5139692244004,-1.17654981590141,-2.04465487882865));
#24489=CARTESIAN_POINT('Ctrl Pts',(96.519912610302,-1.17626457322564,-2.0442563528917));
#24490=CARTESIAN_POINT('Ctrl Pts',(96.5517314567133,-1.17449569331199,-2.04213381626362));
#24491=CARTESIAN_POINT('Ctrl Pts',(96.5775569439145,-1.17220315410673,-2.04045014000125));
#24492=CARTESIAN_POINT('Ctrl Pts',(96.7101369196081,-1.15600780121043,-2.03191227135534));
#24493=CARTESIAN_POINT('Ctrl Pts',(96.8146964297244,-1.12836926041473,-2.02548763647532));
#24494=CARTESIAN_POINT('Ctrl Pts',(96.9452826567516,-1.07387500567844,-2.01649285745702));
#24495=CARTESIAN_POINT('Ctrl Pts',(96.975933930004,-1.05950371251568,-2.01430935942239));
#24496=CARTESIAN_POINT('Ctrl Pts',(97.0146937859113,-1.03925028156982,-2.01142934542412));
#24497=CARTESIAN_POINT('Ctrl Pts',(97.0234072102067,-1.03455644166486,-2.01077391122977));
#24498=CARTESIAN_POINT('Ctrl Pts',(97.0373236404962,-1.02683192941039,-2.00971363541899));
#24499=CARTESIAN_POINT('Ctrl Pts',(97.0425644892387,-1.02387013429646,-2.00931122331163));
#24500=CARTESIAN_POINT('Ctrl Pts',(97.0524230002938,-1.01819857328577,-2.00854821457269));
#24501=CARTESIAN_POINT('Ctrl Pts',(97.0570453546711,-1.01549723534819,-2.00818792540718));
#24502=CARTESIAN_POINT('Ctrl Pts',(97.0671571730133,-1.00949494883088,-2.00739407998663));
#24503=CARTESIAN_POINT('Ctrl Pts',(97.0726384193169,-1.00618056095106,-2.00696004818888));
#24504=CARTESIAN_POINT('Ctrl Pts',(97.0843157588999,-0.998988796768864,
-2.00602726223556));
#24505=CARTESIAN_POINT('Ctrl Pts',(97.0905033133298,-0.995098137063567,
-2.00552803852777));
#24506=CARTESIAN_POINT('Ctrl Pts',(97.106653721477,-0.984731941841143,-2.00421171745379));
#24507=CARTESIAN_POINT('Ctrl Pts',(97.1165552786883,-0.978162923726331,
-2.00339125282272));
#24508=CARTESIAN_POINT('Ctrl Pts',(97.1462315183982,-0.957821429680231,
-2.00089055685106));
#24509=CARTESIAN_POINT('Ctrl Pts',(97.1656835017828,-0.943591519510457,
-1.99919410556129));
#24510=CARTESIAN_POINT('Ctrl Pts',(97.235910573339,-0.888832690868671,-1.99285372455286));
#24511=CARTESIAN_POINT('Ctrl Pts',(97.2837397689966,-0.844723599532997,
-1.9880932340306));
#24512=CARTESIAN_POINT('Ctrl Pts',(97.3679207513842,-0.753116368535732,
-1.97896360230924));
#24513=CARTESIAN_POINT('Ctrl Pts',(97.4047874258182,-0.706341247486207,
-1.97461025231344));
#24514=CARTESIAN_POINT('Ctrl Pts',(97.4435535785153,-0.648662946639332,
-1.96973694503724));
#24515=CARTESIAN_POINT('Ctrl Pts',(97.4490354917982,-0.640277553681871,
-1.9690399615192));
#24516=CARTESIAN_POINT('Ctrl Pts',(97.4565229461797,-0.628498939443639,
-1.96807792372593));
#24517=CARTESIAN_POINT('Ctrl Pts',(97.4586192769795,-0.625164343482821,
-1.9678074345278));
#24518=CARTESIAN_POINT('Ctrl Pts',(97.4622074447231,-0.619392650511335,
-1.96734255687311));
#24519=CARTESIAN_POINT('Ctrl Pts',(97.4637071974763,-0.61696055186336,-1.96714766795057));
#24520=CARTESIAN_POINT('Ctrl Pts',(97.4668533511026,-0.61181673366493,-1.96673763493402));
#24521=CARTESIAN_POINT('Ctrl Pts',(97.468497673958,-0.609103776011535,-1.96652263148782));
#24522=CARTESIAN_POINT('Ctrl Pts',(97.4725521360846,-0.602352959972884,
-1.96599065220529));
#24523=CARTESIAN_POINT('Ctrl Pts',(97.4749491248026,-0.598307193898127,
-1.96567450909875));
#24524=CARTESIAN_POINT('Ctrl Pts',(97.4839075824221,-0.582978004483678,
-1.96448628793706));
#24525=CARTESIAN_POINT('Ctrl Pts',(97.4903058464082,-0.571599635406815,
-1.96362388383606));
#24526=CARTESIAN_POINT('Ctrl Pts',(97.5062624156401,-0.542085191527672,
-1.96143054585596));
#24527=CARTESIAN_POINT('Ctrl Pts',(97.5155390735839,-0.523801187775625,
-1.96011326980412));
#24528=CARTESIAN_POINT('Ctrl Pts',(97.5734463777405,-0.40187973268035,-1.95153871084709));
#24529=CARTESIAN_POINT('Ctrl Pts',(97.6072219320987,-0.291868963456379,
-1.94471740784097));
#24530=CARTESIAN_POINT('Ctrl Pts',(97.6282670699309,-0.154779459729459,
-1.9357990309268));
#24531=CARTESIAN_POINT('Ctrl Pts',(97.6312015066026,-0.130745367146268,
-1.93422350831416));
#24532=CARTESIAN_POINT('Ctrl Pts',(97.6341863923211,-0.0979149514149447,
-1.93204677610304));
#24533=CARTESIAN_POINT('Ctrl Pts',(97.6348822049479,-0.0891823332805456,
-1.93146544699207));
#24534=CARTESIAN_POINT('Ctrl Pts',(97.6358354863779,-0.0752581151963874,
-1.93053444410522));
#24535=CARTESIAN_POINT('Ctrl Pts',(97.6361561246045,-0.0700710527880929,
-1.93018672841799));
#24536=CARTESIAN_POINT('Ctrl Pts',(97.6367305047784,-0.0596606488056806,
-1.92948698531686));
#24537=CARTESIAN_POINT('Ctrl Pts',(97.6369838083924,-0.054437402706353,
-1.92913495253947));
#24538=CARTESIAN_POINT('Ctrl Pts',(97.6374250731574,-0.043886355395171,
-1.9284218537882));
#24539=CARTESIAN_POINT('Ctrl Pts',(97.6376116616151,-0.0385586226547256,
-1.92806075377877));
#24540=CARTESIAN_POINT('Ctrl Pts',(97.6379190328841,-0.0276689542300539,
-1.92732052551768));
#24541=CARTESIAN_POINT('Ctrl Pts',(97.6380365901767,-0.0221070690059054,
-1.9269413067899));
#24542=CARTESIAN_POINT('Ctrl Pts',(97.6381940702366,-0.0108977695560703,
-1.92617466258363));
#24543=CARTESIAN_POINT('Ctrl Pts',(97.6382327850347,-0.00525050195161463,
-1.92578721105986));
#24544=CARTESIAN_POINT('Ctrl Pts',(97.6382308827581,0.000396726675349013,
-1.92539852201626));
#24545=CARTESIAN_POINT('Ctrl Pts',(97.6382308830244,0.000395935232192423,
-1.92539857648991));
#24546=CARTESIAN_POINT('Ctrl Pts',(97.6382265374016,0.0133224357143192,
-1.92450886793651));
#24547=CARTESIAN_POINT('Ctrl Pts',(97.6380093786908,0.0262476305489435,
-1.92361273883065));
#24548=CARTESIAN_POINT('Ctrl Pts',(97.6340026413434,0.146665539748613,-1.91520159267001));
#24549=CARTESIAN_POINT('Ctrl Pts',(97.6157159879922,0.253154930688317,-1.90723146849538));
#24550=CARTESIAN_POINT('Ctrl Pts',(97.5745577916515,0.383087365134138,-1.8972993930315));
#24551=CARTESIAN_POINT('Ctrl Pts',(97.5648648723803,0.410194480244713,-1.89521967475728));
#24552=CARTESIAN_POINT('Ctrl Pts',(97.5480497718657,0.452286294200139,-1.89200350308879));
#24553=CARTESIAN_POINT('Ctrl Pts',(97.541588004908,0.467521591985525,-1.89084226700691));
#24554=CARTESIAN_POINT('Ctrl Pts',(97.5327027430685,0.487300580287322,-1.88934302041255));
#24555=CARTESIAN_POINT('Ctrl Pts',(97.5305679007914,0.49197088253236,-1.88898962966034));
#24556=CARTESIAN_POINT('Ctrl Pts',(97.5270256584936,0.499587938464253,-1.88841445409155));
#24557=CARTESIAN_POINT('Ctrl Pts',(97.5256364561683,0.502543004942228,-1.88819160730473));
#24558=CARTESIAN_POINT('Ctrl Pts',(97.5228959461513,0.508310112603684,-1.88775733158221));
#24559=CARTESIAN_POINT('Ctrl Pts',(97.5215457298677,0.511122615330469,-1.88754584338941));
#24560=CARTESIAN_POINT('Ctrl Pts',(97.5184996252597,0.517403565974013,-1.88707414224255));
#24561=CARTESIAN_POINT('Ctrl Pts',(97.5167978095243,0.520869139621444,-1.88681428733463));
#24562=CARTESIAN_POINT('Ctrl Pts',(97.5108244764237,0.532883537244145,-1.88591463980817));
#24563=CARTESIAN_POINT('Ctrl Pts',(97.5064658387097,0.541388967961465,-1.88527989069258));
#24564=CARTESIAN_POINT('Ctrl Pts',(97.4669072691013,0.61632186985188,-1.87969848995107));
#24565=CARTESIAN_POINT('Ctrl Pts',(97.4255206016595,0.67929986111712,-1.87507585288536));
#24566=CARTESIAN_POINT('Ctrl Pts',(97.3332435553384,0.794088350413717,-1.86596539129276));
#24567=CARTESIAN_POINT('Ctrl Pts',(97.2830243565291,0.845997443456439,-1.86149606498231));
#24568=CARTESIAN_POINT('Ctrl Pts',(97.2187048511936,0.90130703189762,-1.85599591993341));
#24569=CARTESIAN_POINT('Ctrl Pts',(97.2088966591738,0.909467842644396,-1.85516306220863));
#24570=CARTESIAN_POINT('Ctrl Pts',(97.1929873035577,0.922273414766934,-1.85382000104842));
#24571=CARTESIAN_POINT('Ctrl Pts',(97.186969841719,0.927020871013304,-1.85331376463745));
#24572=CARTESIAN_POINT('Ctrl Pts',(97.1756448223154,0.935777717666839,-1.85236396946781));
#24573=CARTESIAN_POINT('Ctrl Pts',(97.1703487826643,0.939801552597389,-1.85192098935931));
#24574=CARTESIAN_POINT('Ctrl Pts',(97.1649361907103,0.943842087654171,-1.85146936149807));
#24575=CARTESIAN_POINT('Ctrl Pts',(97.1648533396377,0.94390391953186,-1.85146244864693));
#24576=CARTESIAN_POINT('Ctrl Pts',(97.164683929823,0.944030315600954,-1.85144831411957));
#24577=CARTESIAN_POINT('Ctrl Pts',(97.1645973702088,0.944094878896012,-1.85144109239429));
#24578=CARTESIAN_POINT('Ctrl Pts',(97.1644200597669,0.944227093689571,-1.85142629984869));
#24579=CARTESIAN_POINT('Ctrl Pts',(97.1643293081691,0.944294743933026,-1.85141872899212));
#24580=CARTESIAN_POINT('Ctrl Pts',(97.1600480405124,0.947485229598423,-1.85106158341241));
#24581=CARTESIAN_POINT('Ctrl Pts',(97.1558368532831,0.950580107464455,-1.85071094649116));
#24582=CARTESIAN_POINT('Ctrl Pts',(97.1468005336648,0.957128884350087,-1.84995987962198));
#24583=CARTESIAN_POINT('Ctrl Pts',(97.141969633464,0.960574538634427,-1.84955914885511));
#24584=CARTESIAN_POINT('Ctrl Pts',(97.1293353117628,0.969442726550406,-1.84851304672887));
#24585=CARTESIAN_POINT('Ctrl Pts',(97.1214920662787,0.974807494994599,-1.84786553274616));
#24586=CARTESIAN_POINT('Ctrl Pts',(97.0885082505502,0.996787268299319,-1.84514967697788));
#24587=CARTESIAN_POINT('Ctrl Pts',(97.062801588149,1.01252788335023,-1.84304979373217));
#24588=CARTESIAN_POINT('Ctrl Pts',(96.9548714637412,1.07304992323332,-1.83429476235444));
#24589=CARTESIAN_POINT('Ctrl Pts',(96.8680604937866,1.10893303302928,-1.82735888733692));
#24590=CARTESIAN_POINT('Ctrl Pts',(96.7498076825339,1.1420325681494,-1.81840722328497));
#24591=CARTESIAN_POINT('Ctrl Pts',(96.7213926840502,1.14885753705859,-1.816295139538));
#24592=CARTESIAN_POINT('Ctrl Pts',(96.6817320533384,1.15683592389939,-1.81342382391201));
#24593=CARTESIAN_POINT('Ctrl Pts',(96.6706809314123,1.15889490205243,-1.81263191720072));
#24594=CARTESIAN_POINT('Ctrl Pts',(96.6513987829117,1.16220252509426,-1.81126621562524));
#24595=CARTESIAN_POINT('Ctrl Pts',(96.643181000078,1.16352268124223,-1.81068920924578));
#24596=CARTESIAN_POINT('Ctrl Pts',(96.6310586186805,1.16533849200656,-1.80984611217004));
#24597=CARTESIAN_POINT('Ctrl Pts',(96.6271646421,1.16590183545736,-1.80957651310455));
#24598=CARTESIAN_POINT('Ctrl Pts',(96.6202479264211,1.16686711888864,-1.80909988916422));
#24599=CARTESIAN_POINT('Ctrl Pts',(96.617226371315,1.16727684528748,-1.80889244378358));
#24600=CARTESIAN_POINT('Ctrl Pts',(96.6106562409375,1.16814179060423,-1.8084430482769));
#24601=CARTESIAN_POINT('Ctrl Pts',(96.6071071649316,1.16859257866669,-1.80820134366274));
#24602=CARTESIAN_POINT('Ctrl Pts',(96.5972226145616,1.16980233054787,-1.80753095765668));
#24603=CARTESIAN_POINT('Ctrl Pts',(96.5908828287067,1.17052600565403,-1.80710416599151));
#24604=CARTESIAN_POINT('Ctrl Pts',(96.5549688957119,1.17433010277992,-1.80470285810397));
#24605=CARTESIAN_POINT('Ctrl Pts',(96.5252896045336,1.17634150528124,-1.8027812045559));
#24606=CARTESIAN_POINT('Ctrl Pts',(96.4161091922748,1.17959517452041,-1.79583885398311));
#24607=CARTESIAN_POINT('Ctrl Pts',(96.3366156143811,1.17391335454048,-1.79101798267954));
#24608=CARTESIAN_POINT('Ctrl Pts',(96.222129885758,1.15396342425084,-1.7837600418481));
#24609=CARTESIAN_POINT('Ctrl Pts',(96.1862800958604,1.14597399117042,-1.78144292815811));
#24610=CARTESIAN_POINT('Ctrl Pts',(96.1355998615186,1.1321650175806,-1.77806032880301));
#24611=CARTESIAN_POINT('Ctrl Pts',(96.1204218300319,1.12769903243303,-1.7770333684734));
#24612=CARTESIAN_POINT('Ctrl Pts',(96.0934164567984,1.11915820266238,-1.775177919535));
#24613=CARTESIAN_POINT('Ctrl Pts',(96.0815552253899,1.11519805440487,-1.77435306444595));
#24614=CARTESIAN_POINT('Ctrl Pts',(96.063555870699,1.10886824776053,-1.77308508003484));
#24615=CARTESIAN_POINT('Ctrl Pts',(96.0573705773663,1.10663468859501,-1.77264638680972));
#24616=CARTESIAN_POINT('Ctrl Pts',(96.046615419615,1.1026487822053,-1.77187824271381));
#24617=CARTESIAN_POINT('Ctrl Pts',(96.0420371270102,1.10091951563691,-1.77154955824596));
#24618=CARTESIAN_POINT('Ctrl Pts',(96.0317316808656,1.09695347657279,-1.77080580047142));
#24619=CARTESIAN_POINT('Ctrl Pts',(96.0260110346347,1.09470030406605,-1.77039019184144));
#24620=CARTESIAN_POINT('Ctrl Pts',(96.0105812905629,1.08848304426616,-1.76926162753148));
#24621=CARTESIAN_POINT('Ctrl Pts',(96.0009072628689,1.08443397908109,-1.76854586396962));
#24622=CARTESIAN_POINT('Ctrl Pts',(95.9677690356828,1.07004091986321,-1.76606499384043));
#24623=CARTESIAN_POINT('Ctrl Pts',(95.9445945127439,1.05906241155277,-1.76427917195862));
#24624=CARTESIAN_POINT('Ctrl Pts',(95.9218016575013,1.04733933507189,-1.76247028589786));
#24625=CARTESIAN_POINT('Ctrl Pts',(95.9218016746715,1.04733934390307,-1.66387871395933));
#24626=CARTESIAN_POINT('Ctrl Pts',(95.9874065823963,1.08108199314961,-1.66871641355271));
#24627=CARTESIAN_POINT('Ctrl Pts',(96.0560516960037,1.10859344400043,-1.67324998907324));
#24628=CARTESIAN_POINT('Ctrl Pts',(96.1798847932374,1.14517280797898,-1.68123788313726));
#24629=CARTESIAN_POINT('Ctrl Pts',(96.2339704036729,1.15708569258995,-1.68466684759082));
#24630=CARTESIAN_POINT('Ctrl Pts',(96.3089401753641,1.16813931648903,-1.68950332679055));
#24631=CARTESIAN_POINT('Ctrl Pts',(96.329264336922,1.17059651313738,-1.69082223599255));
#24632=CARTESIAN_POINT('Ctrl Pts',(96.3648574137405,1.17396115743478,-1.69315282719167));
#24633=CARTESIAN_POINT('Ctrl Pts',(96.3800994239755,1.17510315939306,-1.6941574650653));
#24634=CARTESIAN_POINT('Ctrl Pts',(96.4024659588175,1.17634178285479,-1.6956433513529));
#24635=CARTESIAN_POINT('Ctrl Pts',(96.4095764147224,1.17667091994869,-1.69611744143678));
#24636=CARTESIAN_POINT('Ctrl Pts',(96.4221552805284,1.17713895697171,-1.69695937082973));
#24637=CARTESIAN_POINT('Ctrl Pts',(96.4276225425088,1.17730425306818,-1.69732638473655));
#24638=CARTESIAN_POINT('Ctrl Pts',(96.4390787353004,1.17757075538391,-1.69809778303085));
#24639=CARTESIAN_POINT('Ctrl Pts',(96.4450676687329,1.1776643695043,-1.69850239123021));
#24640=CARTESIAN_POINT('Ctrl Pts',(96.4608169346172,1.17779039424939,-1.69957006866021));
#24641=CARTESIAN_POINT('Ctrl Pts',(96.4705772375064,1.1777471633159,-1.70023544804834));
#24642=CARTESIAN_POINT('Ctrl Pts',(96.5128753048144,1.17703399513266,-1.70313577864109));
#24643=CARTESIAN_POINT('Ctrl Pts',(96.5453752487215,1.17513692738986,-1.70540789179309));
#24644=CARTESIAN_POINT('Ctrl Pts',(96.5911907809928,1.17055217775959,-1.70867466683405));
#24645=CARTESIAN_POINT('Ctrl Pts',(96.6046046154995,1.16897639331651,-1.70963881378869));
#24646=CARTESIAN_POINT('Ctrl Pts',(96.697363342933,1.15645880893665,-1.71635763159815));
#24647=CARTESIAN_POINT('Ctrl Pts',(96.7754359834501,1.13767821608332,-1.72229515390929));
#24648=CARTESIAN_POINT('Ctrl Pts',(96.876669926672,1.10209925641833,-1.73010393818607));
#24649=CARTESIAN_POINT('Ctrl Pts',(96.902032010247,1.09218537439806,-1.73206796963107));
#24650=CARTESIAN_POINT('Ctrl Pts',(96.9368819535102,1.0771500779737,-1.73475840160834));
#24651=CARTESIAN_POINT('Ctrl Pts',(96.9466764950858,1.072764707066,-1.73551357681964));
#24652=CARTESIAN_POINT('Ctrl Pts',(96.9636926020061,1.06486504326818,-1.73682221424171));
#24653=CARTESIAN_POINT('Ctrl Pts',(96.9709405861838,1.06140967385204,-1.73737855158689));
#24654=CARTESIAN_POINT('Ctrl Pts',(96.9816359074506,1.0561759363987,-1.73819729657352));
#24655=CARTESIAN_POINT('Ctrl Pts',(96.9851105287744,1.0544543159644,-1.73846293664237));
#24656=CARTESIAN_POINT('Ctrl Pts',(96.9910381017498,1.05148074364423,-1.73891543248546));
#24657=CARTESIAN_POINT('Ctrl Pts',(96.9934952338924,1.05023731569194,-1.7391028006834));
#24658=CARTESIAN_POINT('Ctrl Pts',(96.9990656815541,1.04739381379419,-1.73952709955042));
#24659=CARTESIAN_POINT('Ctrl Pts',(97.0021762423927,1.04578847059808,-1.73976370091689));
#24660=CARTESIAN_POINT('Ctrl Pts',(97.0106366038505,1.04137424953121,-1.7404064571907));
#24661=CARTESIAN_POINT('Ctrl Pts',(97.0159721096619,1.03853798506619,-1.74081096439893));
#24662=CARTESIAN_POINT('Ctrl Pts',(97.0429148130358,1.02394865513482,-1.74285051377832));
#24663=CARTESIAN_POINT('Ctrl Pts',(97.0641735631732,1.01156091434871,-1.74444968237002));
#24664=CARTESIAN_POINT('Ctrl Pts',(97.1781815782754,0.940251406274959,-1.75305684475485));
#24665=CARTESIAN_POINT('Ctrl Pts',(97.2627259096116,0.869237568568173,-1.75960485505639));
#24666=CARTESIAN_POINT('Ctrl Pts',(97.3510290968172,0.771045040579024,-1.7680085092121));
#24667=CARTESIAN_POINT('Ctrl Pts',(97.3653827705877,0.754147903970396,-1.76943325672768));
#24668=CARTESIAN_POINT('Ctrl Pts',(97.3894153944185,0.724182176632936,-1.77193333585525));
#24669=CARTESIAN_POINT('Ctrl Pts',(97.3993165196055,0.711299345245394,-1.77300007966956));
#24670=CARTESIAN_POINT('Ctrl Pts',(97.4132707338397,0.692343748391156,-1.77456053789185));
#24671=CARTESIAN_POINT('Ctrl Pts',(97.4175391277476,0.686431262788284,-1.7750460077719));
#24672=CARTESIAN_POINT('Ctrl Pts',(97.4249269249468,0.675994980496577,-1.77590094643916));
#24673=CARTESIAN_POINT('Ctrl Pts',(97.4280701187247,0.671488235986576,-1.7762695020053));
#24674=CARTESIAN_POINT('Ctrl Pts',(97.4345294084826,0.662087313216371,-1.77703707545382));
#24675=CARTESIAN_POINT('Ctrl Pts',(97.4378404132863,0.657189841005155,-1.77743627005851));
#24676=CARTESIAN_POINT('Ctrl Pts',(97.4463214954682,0.64443919861429,-1.77847395690659));
#24677=CARTESIAN_POINT('Ctrl Pts',(97.451434569016,0.636548802423145,-1.77911452816184));
#24678=CARTESIAN_POINT('Ctrl Pts',(97.472069136209,0.603854720695765,-1.78176295789987));
#24679=CARTESIAN_POINT('Ctrl Pts',(97.4867569813319,0.578539912404008,-1.78380043219542));
#24680=CARTESIAN_POINT('Ctrl Pts',(97.5401676937403,0.478039140287111,-1.79184460287288));
#24681=CARTESIAN_POINT('Ctrl Pts',(97.5716883899895,0.399323475348345,-1.79807431120318));
#24682=CARTESIAN_POINT('Ctrl Pts',(97.6082085949057,0.269057959989549,-1.80797950668187));
#24683=CARTESIAN_POINT('Ctrl Pts',(97.6187374865789,0.219348781594485,-1.8116644356084));
#24684=CARTESIAN_POINT('Ctrl Pts',(97.6272038178963,0.160996968519254,-1.81577919279866));
#24685=CARTESIAN_POINT('Ctrl Pts',(97.6282962919561,0.152871222990137,-1.8163474489432));
#24686=CARTESIAN_POINT('Ctrl Pts',(97.629784415835,0.140853674689231,-1.81718023996038));
#24687=CARTESIAN_POINT('Ctrl Pts',(97.6302456477839,0.136970455985371,-1.8174481652073));
#24688=CARTESIAN_POINT('Ctrl Pts',(97.6310318523547,0.130057414186865,-1.81792296334277));
#24689=CARTESIAN_POINT('Ctrl Pts',(97.6313644169031,0.127028554451477,-1.81813024433745));
#24690=CARTESIAN_POINT('Ctrl Pts',(97.6320636612878,0.120423965173217,-1.81858059722782));
#24691=CARTESIAN_POINT('Ctrl Pts',(97.6324257295137,0.116847830151574,-1.81882341415583));
#24692=CARTESIAN_POINT('Ctrl Pts',(97.6333923449253,0.106843824659397,-1.81949993489929));
#24693=CARTESIAN_POINT('Ctrl Pts',(97.633960429977,0.100412439147494,-1.81993169298631));
#24694=CARTESIAN_POINT('Ctrl Pts',(97.6369579194472,0.0629665291762586,
-1.82242884890476));
#24695=CARTESIAN_POINT('Ctrl Pts',(97.6382108437233,0.0318672258974681,
-1.82443628325917));
#24696=CARTESIAN_POINT('Ctrl Pts',(97.6382605139807,-0.0459298935289674,
-1.82937244222079));
#24697=CARTESIAN_POINT('Ctrl Pts',(97.6355148373996,-0.0925748096218537,
-1.83225609327581));
#24698=CARTESIAN_POINT('Ctrl Pts',(97.6206686781264,-0.217546054248038,
-1.84004046210982));
#24699=CARTESIAN_POINT('Ctrl Pts',(97.6034297959604,-0.295004754101485,
-1.84494164946959));
#24700=CARTESIAN_POINT('Ctrl Pts',(97.5736905230242,-0.384836338535954,
-1.85110819682083));
#24701=CARTESIAN_POINT('Ctrl Pts',(97.5685378736786,-0.399430067267293,
-1.85212521556819));
#24702=CARTESIAN_POINT('Ctrl Pts',(97.5606123859008,-0.420542459712869,
-1.85362089413242));
#24703=CARTESIAN_POINT('Ctrl Pts',(97.5580657988696,-0.427144744270413,
-1.85409214337672));
#24704=CARTESIAN_POINT('Ctrl Pts',(97.5534415482593,-0.438819132312755,
-1.8549318828774));
#24705=CARTESIAN_POINT('Ctrl Pts',(97.5513876665051,-0.443900478019776,
-1.8552995758933));
#24706=CARTESIAN_POINT('Ctrl Pts',(97.547029319414,-0.454470168053956,-1.85606908909231));
#24707=CARTESIAN_POINT('Ctrl Pts',(97.5447185679568,-0.459955735146672,
-1.85647111091044));
#24708=CARTESIAN_POINT('Ctrl Pts',(97.5385768631842,-0.474232241061616,
-1.85752446885855));
#24709=CARTESIAN_POINT('Ctrl Pts',(97.5346800168592,-0.482994173690746,
-1.85817800364721));
#24710=CARTESIAN_POINT('Ctrl Pts',(97.5163293005834,-0.522934312399349,
-1.86119030221261));
#24711=CARTESIAN_POINT('Ctrl Pts',(97.500623440765,-0.553515327286324,-1.86359110997501));
#24712=CARTESIAN_POINT('Ctrl Pts',(97.4504137820354,-0.641574805470655,
-1.87079290214668));
#24713=CARTESIAN_POINT('Ctrl Pts',(97.4123188258956,-0.696841492116763,
-1.87570160157661));
#24714=CARTESIAN_POINT('Ctrl Pts',(97.3317802821103,-0.794669116662105,
-1.88500044629635));
#24715=CARTESIAN_POINT('Ctrl Pts',(97.2903672780105,-0.837825543313859,
-1.88937327245381));
#24716=CARTESIAN_POINT('Ctrl Pts',(97.2383605747578,-0.884363894894569,
-1.8942676152662));
#24717=CARTESIAN_POINT('Ctrl Pts',(97.2307800504178,-0.890974478804823,
-1.89496741043804));
#24718=CARTESIAN_POINT('Ctrl Pts',(97.2201091218693,-0.900042036004292,
-1.89593266403938));
#24719=CARTESIAN_POINT('Ctrl Pts',(97.2170899052438,-0.902581584145772,
-1.89620360364056));
#24720=CARTESIAN_POINT('Ctrl Pts',(97.2118609580602,-0.906935123305624,
-1.89666903385385));
#24721=CARTESIAN_POINT('Ctrl Pts',(97.2096573026681,-0.908756308064865,
-1.89686402773852));
#24722=CARTESIAN_POINT('Ctrl Pts',(97.2049960683024,-0.912580051288523,
-1.89727401811257));
#24723=CARTESIAN_POINT('Ctrl Pts',(97.202536995926,-0.914580743579433,-1.89748887538521));
#24724=CARTESIAN_POINT('Ctrl Pts',(97.1964179716491,-0.91951823334458,-1.89802004799025));
#24725=CARTESIAN_POINT('Ctrl Pts',(97.1927484399336,-0.922443172414382,
-1.89833553597576));
#24726=CARTESIAN_POINT('Ctrl Pts',(97.1788612707817,-0.933377373063629,
-1.8995184657339));
#24727=CARTESIAN_POINT('Ctrl Pts',(97.1685284767702,-0.941239788765041,
-1.90037634373999));
#24728=CARTESIAN_POINT('Ctrl Pts',(97.1416739331571,-0.960981349964681,
-1.90255552620151));
#24729=CARTESIAN_POINT('Ctrl Pts',(97.1249700737067,-0.972606465951632,
-1.90386339315204));
#24730=CARTESIAN_POINT('Ctrl Pts',(97.0593589304402,-1.01578895622613,-1.90885462969111));
#24731=CARTESIAN_POINT('Ctrl Pts',(97.0084378516857,-1.04413892500902,-1.91242766571903));
#24732=CARTESIAN_POINT('Ctrl Pts',(96.8872956799053,-1.10027080822645,-1.92069505608037));
#24733=CARTESIAN_POINT('Ctrl Pts',(96.8160951131574,-1.12530130705123,-1.92539903317699));
#24734=CARTESIAN_POINT('Ctrl Pts',(96.7329126849427,-1.14585511199141,-1.93102252777811));
#24735=CARTESIAN_POINT('Ctrl Pts',(96.7227950213598,-1.14821352746912,-1.93170831843164));
#24736=CARTESIAN_POINT('Ctrl Pts',(96.7060785763117,-1.15187763910823,-1.9328449861449));
#24737=CARTESIAN_POINT('Ctrl Pts',(96.699497318131,-1.15326122892853,-1.93329340389738));
#24738=CARTESIAN_POINT('Ctrl Pts',(96.6875831576846,-1.15565960203979,-1.9341069930619));
#24739=CARTESIAN_POINT('Ctrl Pts',(96.6822543662831,-1.15669402984175,-1.93447153491668));
#24740=CARTESIAN_POINT('Ctrl Pts',(96.670801761285,-1.15883516657506,-1.93525649277245));
#24741=CARTESIAN_POINT('Ctrl Pts',(96.6646759690419,-1.1599302472946,-1.9356772620017));
#24742=CARTESIAN_POINT('Ctrl Pts',(96.6478634735958,-1.16279843453487,-1.93683471821879));
#24743=CARTESIAN_POINT('Ctrl Pts',(96.6371607571133,-1.1644726882509,-1.93757446383531));
#24744=CARTESIAN_POINT('Ctrl Pts',(96.5736196088846,-1.17351645522519,-1.94198479108199));
#24745=CARTESIAN_POINT('Ctrl Pts',(96.5203604817114,-1.17743543172055,-1.94576135206359));
#24746=CARTESIAN_POINT('Ctrl Pts',(96.4190680711731,-1.17799831779682,-1.95308254129094));
#24747=CARTESIAN_POINT('Ctrl Pts',(96.3711411256809,-1.17533528221762,-1.9566046712098));
#24748=CARTESIAN_POINT('Ctrl Pts',(96.2954957105057,-1.16647788133756,-1.96219259277469));
#24749=CARTESIAN_POINT('Ctrl Pts',(96.2676047627264,-1.16219174298689,-1.96425856314758));
#24750=CARTESIAN_POINT('Ctrl Pts',(96.2058590884811,-1.15041872861541,-1.96881599617489));
#24751=CARTESIAN_POINT('Ctrl Pts',(96.1721235347652,-1.14242988414127,-1.97129499455205));
#24752=CARTESIAN_POINT('Ctrl Pts',(96.132953736093,-1.13130798094432,-1.97412513785748));
#24753=CARTESIAN_POINT('Ctrl Pts',(96.1271339448916,-1.12960683499036,-1.97454435338091));
#24754=CARTESIAN_POINT('Ctrl Pts',(96.1176636671205,-1.12675907364142,-1.9752241408954));
#24755=CARTESIAN_POINT('Ctrl Pts',(96.1140052593695,-1.12563950548969,-1.97548616266111));
#24756=CARTESIAN_POINT('Ctrl Pts',(96.1074477932438,-1.12359775146555,-1.97595469207535));
#24757=CARTESIAN_POINT('Ctrl Pts',(96.1045468020532,-1.12268214550473,-1.9761615634761));
#24758=CARTESIAN_POINT('Ctrl Pts',(96.0981617034755,-1.12063965404669,-1.97661599682087));
#24759=CARTESIAN_POINT('Ctrl Pts',(96.094679286976,-1.11950775560829,-1.97686326712941));
#24760=CARTESIAN_POINT('Ctrl Pts',(96.0845942405277,-1.11617770521514,-1.97757783958933));
#24761=CARTESIAN_POINT('Ctrl Pts',(96.0780056044128,-1.11393720818433,-1.9780427794997));
#24762=CARTESIAN_POINT('Ctrl Pts',(96.0221564836363,-1.09439149808431,-1.98197082297189));
#24763=CARTESIAN_POINT('Ctrl Pts',(95.9740704020626,-1.07388422725954,-1.98526734000446));
#24764=CARTESIAN_POINT('Ctrl Pts',(95.8532897133958,-1.01259029501949,-1.99370416261204));
#24765=CARTESIAN_POINT('Ctrl Pts',(95.7832845678811,-0.967173702669729,
-1.99876819556398));
#24766=CARTESIAN_POINT('Ctrl Pts',(95.6947438146386,-0.895370948082752,
-2.00603938127244));
#24767=CARTESIAN_POINT('Ctrl Pts',(95.6716077258846,-0.875055013142423,
-2.00803071755667));
#24768=CARTESIAN_POINT('Ctrl Pts',(95.6423575451058,-0.847266622960754,
-2.01068964197776));
#24769=CARTESIAN_POINT('Ctrl Pts',(95.6355006037616,-0.840591491429218,
-2.01132372590403));
#24770=CARTESIAN_POINT('Ctrl Pts',(95.6245147643332,-0.829633038820408,
-2.01235776537758));
#24771=CARTESIAN_POINT('Ctrl Pts',(95.6203355512092,-0.825400599332993,
-2.01275550724539));
#24772=CARTESIAN_POINT('Ctrl Pts',(95.6123664543246,-0.817206778744284,
-2.01352252353536));
#24773=CARTESIAN_POINT('Ctrl Pts',(95.6085718098671,-0.813250227308947,
-2.01389157855539));
#24774=CARTESIAN_POINT('Ctrl Pts',(95.5998524921288,-0.804030887944494,
-2.01474860396121));
#24775=CARTESIAN_POINT('Ctrl Pts',(95.5949482742703,-0.798749143673022,
-2.01523742210443));
#24776=CARTESIAN_POINT('Ctrl Pts',(95.5794665227027,-0.78176560013576,-2.01680261402721));
#24777=CARTESIAN_POINT('Ctrl Pts',(95.5690758420639,-0.769896594638083,
-2.01788663143811));
#24778=CARTESIAN_POINT('Ctrl Pts',(95.5452039149818,-0.741497048947946,
-2.02045895531311));
#24779=CARTESIAN_POINT('Ctrl Pts',(95.5319275382242,-0.724802309666254,
-2.02195475662898));
#24780=CARTESIAN_POINT('Ctrl Pts',(95.4834162532731,-0.660278773097111,
-2.02767581048405));
#24781=CARTESIAN_POINT('Ctrl Pts',(95.451366895428,-0.610172826389735,-2.03200363925536));
#24782=CARTESIAN_POINT('Ctrl Pts',(95.3899054552065,-0.495897761151994,
-2.04152244327016));
#24783=CARTESIAN_POINT('Ctrl Pts',(95.362192718275,-0.431058259368894,-2.0467080650873));
#24784=CARTESIAN_POINT('Ctrl Pts',(95.3373936634184,-0.354776947256575,
-2.05233001573151));
#24785=CARTESIAN_POINT('Ctrl Pts',(95.3344709065608,-0.345388380519731,
-2.05301383583765));
#24786=CARTESIAN_POINT('Ctrl Pts',(95.3305565283764,-0.332236347547889,
-2.05395945255309));
#24787=CARTESIAN_POINT('Ctrl Pts',(95.3294655539239,-0.328503217833987,
-2.05422648470844));
#24788=CARTESIAN_POINT('Ctrl Pts',(95.3276086492878,-0.322030287390161,
-2.05468703632373));
#24789=CARTESIAN_POINT('Ctrl Pts',(95.3268341245526,-0.31929301794782,-2.05488103531357));
#24790=CARTESIAN_POINT('Ctrl Pts',(95.3252129797206,-0.313483420095382,
-2.05529113359179));
#24791=CARTESIAN_POINT('Ctrl Pts',(95.3243688958972,-0.310410405840028,
-2.05550708195386));
#24792=CARTESIAN_POINT('Ctrl Pts',(95.3222918089693,-0.302726481838246,
-2.05604470500677));
#24793=CARTESIAN_POINT('Ctrl Pts',(95.3210743258583,-0.29811137244346,-2.05636550770561));
#24794=CARTESIAN_POINT('Ctrl Pts',(95.31650229571,-0.28034293330303,-2.05759299582215));
#24795=CARTESIAN_POINT('Ctrl Pts',(95.3133470291543,-0.267138780883901,
-2.05848916391478));
#24796=CARTESIAN_POINT('Ctrl Pts',(95.305753650268,-0.232741572011814,-2.06078936372328));
#24797=CARTESIAN_POINT('Ctrl Pts',(95.3016702261665,-0.211474814148675,
-2.06217800425422));
#24798=CARTESIAN_POINT('Ctrl Pts',(95.2816534953787,-0.0890929820410691,
-2.07003976284231));
#24799=CARTESIAN_POINT('Ctrl Pts',(95.2783694083926,0.0136439714255365,
-2.07617658459706));
#24800=CARTESIAN_POINT('Ctrl Pts',(95.2915904042699,0.147789031022744,-2.08475842122349));
#24801=CARTESIAN_POINT('Ctrl Pts',(95.2961024178252,0.179913992057985,-2.08685341434649));
#24802=CARTESIAN_POINT('Ctrl Pts',(95.303686783858,0.221398596969202,-2.08963160044901));
#24803=CARTESIAN_POINT('Ctrl Pts',(95.3055587718141,0.230965007125942,-2.09027730355239));
#24804=CARTESIAN_POINT('Ctrl Pts',(95.3087718284124,0.246367623958067,-2.09132560597837));
#24805=CARTESIAN_POINT('Ctrl Pts',(95.3100390646057,0.252218898923648,-2.09172587506654));
#24806=CARTESIAN_POINT('Ctrl Pts',(95.3125495019763,0.26339776159507,-2.09249460044943));
#24807=CARTESIAN_POINT('Ctrl Pts',(95.3137853221664,0.268726860490963,-2.09286281410708));
#24808=CARTESIAN_POINT('Ctrl Pts',(95.3167158035357,0.280975266883418,-2.09371325295312));
#24809=CARTESIAN_POINT('Ctrl Pts',(95.3184361926592,0.287888136673279,-2.09419628392865));
#24810=CARTESIAN_POINT('Ctrl Pts',(95.3240523328934,0.309612015123492,-2.09572409499397));
#24811=CARTESIAN_POINT('Ctrl Pts',(95.328174182506,0.32436237098646,-2.09677601280118));
#24812=CARTESIAN_POINT('Ctrl Pts',(95.3384901252528,0.35868210911169,-2.09925886757043));
#24813=CARTESIAN_POINT('Ctrl Pts',(95.3449103518647,0.378177761334242,-2.10069661058697));
#24814=CARTESIAN_POINT('Ctrl Pts',(95.3705899389253,0.449800181929712,-2.10608127203403));
#24815=CARTESIAN_POINT('Ctrl Pts',(95.3930196824107,0.500707332150847,-2.11011792912098));
#24816=CARTESIAN_POINT('Ctrl Pts',(95.4545027180122,0.617171342732483,-2.11977013420041));
#24817=CARTESIAN_POINT('Ctrl Pts',(95.4964986029307,0.68090572496438,-2.12539964852766));
#24818=CARTESIAN_POINT('Ctrl Pts',(95.5503250319758,0.747530235764814,-2.13139870292436));
#24819=CARTESIAN_POINT('Ctrl Pts',(95.5563824195848,0.754845090088789,-2.13205885514755));
#24820=CARTESIAN_POINT('Ctrl Pts',(95.5650192417168,0.765021709966009,-2.13297847466055));
#24821=CARTESIAN_POINT('Ctrl Pts',(95.5675250487094,0.767945080791811,-2.13324278901702));
#24822=CARTESIAN_POINT('Ctrl Pts',(95.5720851644442,0.773212587646627,-2.13371922149339));
#24823=CARTESIAN_POINT('Ctrl Pts',(95.5741345246612,0.775560953496885,-2.13393168838374));
#24824=CARTESIAN_POINT('Ctrl Pts',(95.578352361229,0.780355625430431,-2.13436556575212));
#24825=CARTESIAN_POINT('Ctrl Pts',(95.5805217367298,0.782801081314822,-2.13458690760109));
#24826=CARTESIAN_POINT('Ctrl Pts',(95.5861366793817,0.789077758534844,-2.13515524262775));
#24827=CARTESIAN_POINT('Ctrl Pts',(95.5895973023677,0.792895508432947,-2.13550114534366));
#24828=CARTESIAN_POINT('Ctrl Pts',(95.6043853220042,0.808995987230278,-2.1369614641421));
#24829=CARTESIAN_POINT('Ctrl Pts',(95.6159489887381,0.821060331371248,-2.13805958305258));
#24830=CARTESIAN_POINT('Ctrl Pts',(95.6484130874932,0.853518175164644,-2.14103866602832));
#24831=CARTESIAN_POINT('Ctrl Pts',(95.669821961519,0.873387709907603,-2.14289050491705));
#24832=CARTESIAN_POINT('Ctrl Pts',(95.7622086602951,0.952947103714888,-2.15053576523997));
#24833=CARTESIAN_POINT('Ctrl Pts',(95.8393593761262,1.00493669980411,-2.15613886709878));
#24834=CARTESIAN_POINT('Ctrl Pts',(95.9218016761257,1.04733934465099,-2.16205147885552));
#24835=CARTESIAN_POINT('Origin',(96.460480949577,-7.19464945638997E-16,
0.924367114736168));
#24836=CARTESIAN_POINT('',(95.9218016730065,1.04733934304672,-2.76054963702842));
#24837=CARTESIAN_POINT('',(95.9218019448245,1.0473394828511,-2.66237442964626));
#24838=CARTESIAN_POINT('',(95.9218016730721,1.04733934308042,0.924367114736168));
#24839=CARTESIAN_POINT('Ctrl Pts',(95.9218016730066,1.04733934304671,-2.76054963702842));
#24840=CARTESIAN_POINT('Ctrl Pts',(95.9132326700124,1.04293203765476,-2.75987336368931));
#24841=CARTESIAN_POINT('Ctrl Pts',(95.9047176184765,1.03841949818406,-2.75920210559037));
#24842=CARTESIAN_POINT('Ctrl Pts',(95.892070821155,1.03151720700366,-2.75820730834097));
#24843=CARTESIAN_POINT('Ctrl Pts',(95.8878970085419,1.02920622562853,-2.75787935535442));
#24844=CARTESIAN_POINT('Ctrl Pts',(95.880958974298,1.02530946377949,-2.75733495101369));
#24845=CARTESIAN_POINT('Ctrl Pts',(95.8781869792196,1.02373773455601,-2.75711764169615));
#24846=CARTESIAN_POINT('Ctrl Pts',(95.8729518840646,1.02074127761324,-2.75670766670104));
#24847=CARTESIAN_POINT('Ctrl Pts',(95.870487517152,1.01931884549374,-2.756514854594));
#24848=CARTESIAN_POINT('Ctrl Pts',(95.8646652080301,1.01593002053431,-2.7560596834621));
#24849=CARTESIAN_POINT('Ctrl Pts',(95.8613117824295,1.01395587414073,-2.75579781249062));
#24850=CARTESIAN_POINT('Ctrl Pts',(95.8495100623163,1.00692926083719,-2.75487701030639));
#24851=CARTESIAN_POINT('Ctrl Pts',(95.8411151079147,1.00178736822337,-2.75422346941753));
#24852=CARTESIAN_POINT('Ctrl Pts',(95.773446678617,0.959164740115963,-2.74895905624444));
#24853=CARTESIAN_POINT('Ctrl Pts',(95.7175563549036,0.916558161321671,-2.74462789144687));
#24854=CARTESIAN_POINT('Ctrl Pts',(95.6218308237605,0.829040268364834,-2.73660475868495));
#24855=CARTESIAN_POINT('Ctrl Pts',(95.5809914824081,0.785582216163863,-2.73292642696949));
#24856=CARTESIAN_POINT('Ctrl Pts',(95.5302086309947,0.722595810722305,-2.72777066552846));
#24857=CARTESIAN_POINT('Ctrl Pts',(95.5172576316956,0.70560681908888,-2.72639623289441));
#24858=CARTESIAN_POINT('Ctrl Pts',(95.495547289152,0.675460945201987,-2.72397653692191));
#24859=CARTESIAN_POINT('Ctrl Pts',(95.4865773762583,0.662462262333529,-2.72293910632019));
#24860=CARTESIAN_POINT('Ctrl Pts',(95.4738963523066,0.643271246522407,-2.72141377573689));
#24861=CARTESIAN_POINT('Ctrl Pts',(95.4699762599913,0.637218581191932,-2.72093359796891));
#24862=CARTESIAN_POINT('Ctrl Pts',(95.463173819102,0.626501088529011,-2.72008470958096));
#24863=CARTESIAN_POINT('Ctrl Pts',(95.4602679755132,0.621851373887671,-2.71971687105228));
#24864=CARTESIAN_POINT('Ctrl Pts',(95.4542781979452,0.61211637337145,-2.71894756972824));
#24865=CARTESIAN_POINT('Ctrl Pts',(95.4512001104402,0.607027690847516,-2.71854590871304));
#24866=CARTESIAN_POINT('Ctrl Pts',(95.4432728702976,0.593695422780612,-2.71749465214029));
#24867=CARTESIAN_POINT('Ctrl Pts',(95.4384854407034,0.585415836879434,-2.71684287444403));
#24868=CARTESIAN_POINT('Ctrl Pts',(95.4187449981887,0.550295612979295,-2.71408199030836));
#24869=CARTESIAN_POINT('Ctrl Pts',(95.4047456371014,0.522935660261184,-2.71194000590012));
#24870=CARTESIAN_POINT('Ctrl Pts',(95.3568293065428,0.419502723563992,-2.70386919794851));
#24871=CARTESIAN_POINT('Ctrl Pts',(95.3299418540142,0.340451820068217,-2.69773171614675));
#24872=CARTESIAN_POINT('Ctrl Pts',(95.3001198958196,0.208291414447175,-2.68781384935152));
#24873=CARTESIAN_POINT('Ctrl Pts',(95.2920237059147,0.15662714272836,-2.68402429129148));
#24874=CARTESIAN_POINT('Ctrl Pts',(95.2867661979487,0.0976584868549712,
-2.67990658432241));
#24875=CARTESIAN_POINT('Ctrl Pts',(95.2862095877352,0.0907208512844635,
-2.67942540920466));
#24876=CARTESIAN_POINT('Ctrl Pts',(95.285453997222,0.0801257395010773,-2.67869595457418));
#24877=CARTESIAN_POINT('Ctrl Pts',(95.2852105351485,0.0764717384222711,
-2.67844536076252));
#24878=CARTESIAN_POINT('Ctrl Pts',(95.284796017663,0.0697800774980152,-2.67798830329868));
#24879=CARTESIAN_POINT('Ctrl Pts',(95.2846196878171,0.0667428789052191,
-2.67778156355324));
#24880=CARTESIAN_POINT('Ctrl Pts',(95.2842481656671,0.0598843872547714,
-2.67731629199523));
#24881=CARTESIAN_POINT('Ctrl Pts',(95.2840598239468,0.0560628039403301,
-2.67705813837584));
#24882=CARTESIAN_POINT('Ctrl Pts',(95.283621147861,0.0461826494926399,-2.6763933993011));
#24883=CARTESIAN_POINT('Ctrl Pts',(95.2833989683099,0.0401228513938409,
-2.6759882979907));
#24884=CARTESIAN_POINT('Ctrl Pts',(95.2822214008785,-0.000577114962096968,
-2.6732833319678));
#24885=CARTESIAN_POINT('Ctrl Pts',(95.2827483543245,-0.0352467980099046,
-2.6710560519316));
#24886=CARTESIAN_POINT('Ctrl Pts',(95.2864756322027,-0.0979857646210639,
-2.66708476957346));
#24887=CARTESIAN_POINT('Ctrl Pts',(95.2891571902659,-0.12605739482188,-2.66532950534991));
#24888=CARTESIAN_POINT('Ctrl Pts',(95.2991116459099,-0.201529397122044,
-2.66060953932032));
#24889=CARTESIAN_POINT('Ctrl Pts',(95.3082749595134,-0.248624258484052,
-2.65766179375882));
#24890=CARTESIAN_POINT('Ctrl Pts',(95.3336540176208,-0.346706615069992,
-2.6513264108395));
#24891=CARTESIAN_POINT('Ctrl Pts',(95.3505217365088,-0.397408946056569,
-2.64793326244505));
#24892=CARTESIAN_POINT('Ctrl Pts',(95.3748779750875,-0.456813568012807,
-2.64371355054553));
#24893=CARTESIAN_POINT('Ctrl Pts',(95.3791262430919,-0.466780933756201,
-2.64299710562028));
#24894=CARTESIAN_POINT('Ctrl Pts',(95.3860303154601,-0.482379136910381,
-2.64186188057145));
#24895=CARTESIAN_POINT('Ctrl Pts',(95.3885943526769,-0.488050118080993,
-2.64144619183088));
#24896=CARTESIAN_POINT('Ctrl Pts',(95.3934788448068,-0.498629162894915,
-2.64066504532463));
#24897=CARTESIAN_POINT('Ctrl Pts',(95.3957885312433,-0.503542040276796,
-2.64029996176263));
#24898=CARTESIAN_POINT('Ctrl Pts',(95.4010354462312,-0.514505120431153,
-2.63947997312528));
#24899=CARTESIAN_POINT('Ctrl Pts',(95.4039906802311,-0.520546444655338,
-2.63902446021902));
#24900=CARTESIAN_POINT('Ctrl Pts',(95.4116421135927,-0.535854534768218,
-2.63786074671339));
#24901=CARTESIAN_POINT('Ctrl Pts',(95.4164093985132,-0.545084920518406,
-2.63715011576225));
#24902=CARTESIAN_POINT('Ctrl Pts',(95.4568102221068,-0.620833745483993,
-2.6312424878994));
#24903=CARTESIAN_POINT('Ctrl Pts',(95.4986325805745,-0.683837190365049,
-2.62582386383385));
#24904=CARTESIAN_POINT('Ctrl Pts',(95.5826232342057,-0.787275482515682,
-2.61607681347653));
#24905=CARTESIAN_POINT('Ctrl Pts',(95.6223178531364,-0.829409264769488,
-2.61180722784019));
#24906=CARTESIAN_POINT('Ctrl Pts',(95.6800625896936,-0.882305204673697,
-2.60615228369523));
#24907=CARTESIAN_POINT('Ctrl Pts',(95.6955385149769,-0.895755804946732,
-2.60468535183273));
#24908=CARTESIAN_POINT('Ctrl Pts',(95.7214307611859,-0.917098829506772,
-2.6023188779206));
#24909=CARTESIAN_POINT('Ctrl Pts',(95.7316408326781,-0.925233788525854,
-2.6014069955598));
#24910=CARTESIAN_POINT('Ctrl Pts',(95.7457105973547,-0.936066514414634,
-2.6001812959823));
#24911=CARTESIAN_POINT('Ctrl Pts',(95.7494538660239,-0.938913022683455,
-2.5998581083639));
#24912=CARTESIAN_POINT('Ctrl Pts',(95.7557507696648,-0.943642145952737,
-2.59931943395281));
#24913=CARTESIAN_POINT('Ctrl Pts',(95.7582951114067,-0.94553697735684,-2.59910312587095));
#24914=CARTESIAN_POINT('Ctrl Pts',(95.7631456115349,-0.949118882335257,
-2.5986933650031));
#24915=CARTESIAN_POINT('Ctrl Pts',(95.7654502949104,-0.95080787544305,-2.59849977651576));
#24916=CARTESIAN_POINT('Ctrl Pts',(95.7709464485528,-0.95480508337946,-2.5980406764789));
#24917=CARTESIAN_POINT('Ctrl Pts',(95.7741434211886,-0.957105727482686,
-2.59777567343577));
#24918=CARTESIAN_POINT('Ctrl Pts',(95.7855117915613,-0.965200517928264,
-2.59684030872439));
#24919=CARTESIAN_POINT('Ctrl Pts',(95.7937457778294,-0.970906602694444,
-2.59617553101507));
#24920=CARTESIAN_POINT('Ctrl Pts',(95.8512878314194,-1.00970545766571,-2.59160946754066));
#24921=CARTESIAN_POINT('Ctrl Pts',(95.9029707410279,-1.03913692330457,-2.58790632066354));
#24922=CARTESIAN_POINT('Ctrl Pts',(96.0078716847108,-1.08878375329629,-2.58071482083196));
#24923=CARTESIAN_POINT('Ctrl Pts',(96.0607642823805,-1.10929325087114,-2.57723288641729));
#24924=CARTESIAN_POINT('Ctrl Pts',(96.1567222586179,-1.13874367171073,-2.57090918349167));
#24925=CARTESIAN_POINT('Ctrl Pts',(96.1991955152977,-1.14923268047579,-2.5681087357492));
#24926=CARTESIAN_POINT('Ctrl Pts',(96.2522749173291,-1.15924607773393,-2.56455466162513));
#24927=CARTESIAN_POINT('Ctrl Pts',(96.2624239905387,-1.1610231050887,-2.56387278567349));
#24928=CARTESIAN_POINT('Ctrl Pts',(96.2786250135422,-1.16364117920164,-2.56278002424777));
#24929=CARTESIAN_POINT('Ctrl Pts',(96.2846626045186,-1.16456871097074,-2.56237184692209));
#24930=CARTESIAN_POINT('Ctrl Pts',(96.2960943641671,-1.16623400402922,-2.56159708921766));
#24931=CARTESIAN_POINT('Ctrl Pts',(96.3014869830829,-1.16698141310375,-2.56123082055764));
#24932=CARTESIAN_POINT('Ctrl Pts',(96.3137255388461,-1.16859125501356,-2.56039767340886));
#24933=CARTESIAN_POINT('Ctrl Pts',(96.3205742108226,-1.16943096111729,-2.55993010060691));
#24934=CARTESIAN_POINT('Ctrl Pts',(96.3414664401814,-1.1718063769318,-2.55849943774581));
#24935=CARTESIAN_POINT('Ctrl Pts',(96.3555301615037,-1.17314958145816,-2.55753044246678));
#24936=CARTESIAN_POINT('Ctrl Pts',(96.4677409338544,-1.18183284990217,-2.54974864701727));
#24937=CARTESIAN_POINT('Ctrl Pts',(96.5664149179669,-1.17709468562892,-2.54254993508713));
#24938=CARTESIAN_POINT('Ctrl Pts',(96.6737418331414,-1.15832925665328,-2.5345588502835));
#24939=CARTESIAN_POINT('Ctrl Pts',(96.6841328731772,-1.15636788774511,-2.53378402479718));
#24940=CARTESIAN_POINT('Ctrl Pts',(96.7276895862205,-1.14753723154596,-2.53053399668305));
#24941=CARTESIAN_POINT('Ctrl Pts',(96.7605796149405,-1.1393784508278,-2.52807416702513));
#24942=CARTESIAN_POINT('Ctrl Pts',(96.8107558610486,-1.12460761312354,-2.52435190151598));
#24943=CARTESIAN_POINT('Ctrl Pts',(96.8283141461546,-1.11898777010534,-2.52305536999265));
#24944=CARTESIAN_POINT('Ctrl Pts',(96.8507746358994,-1.11121300777785,-2.52141076602248));
#24945=CARTESIAN_POINT('Ctrl Pts',(96.8558030662223,-1.10943406160253,-2.52104348669315));
#24946=CARTESIAN_POINT('Ctrl Pts',(96.8639313669201,-1.10649616946514,-2.5204514680714));
#24947=CARTESIAN_POINT('Ctrl Pts',(96.8670386721522,-1.10535823658944,-2.52022554916265));
#24948=CARTESIAN_POINT('Ctrl Pts',(96.873041241769,-1.10313128670861,-2.51978995775108));
#24949=CARTESIAN_POINT('Ctrl Pts',(96.8759370572823,-1.10204394342511,-2.51958019645816));
#24950=CARTESIAN_POINT('Ctrl Pts',(96.8823408312129,-1.09961057645859,-2.51911711164722));
#24951=CARTESIAN_POINT('Ctrl Pts',(96.8858467329977,-1.09825913647596,-2.51886410315168));
#24952=CARTESIAN_POINT('Ctrl Pts',(96.8983054391025,-1.09338799969193,-2.51796664718892));
#24953=CARTESIAN_POINT('Ctrl Pts',(96.9072218125448,-1.08977530595421,-2.51732739449785));
#24954=CARTESIAN_POINT('Ctrl Pts',(96.9883047012481,-1.05576007689642,-2.5115332611692));
#24955=CARTESIAN_POINT('Ctrl Pts',(97.0573257710082,-1.01833545942506,-2.50673121529573));
#24956=CARTESIAN_POINT('Ctrl Pts',(97.1669000083131,-0.943925914991809,
-2.49853612655973));
#24957=CARTESIAN_POINT('Ctrl Pts',(97.2095209644715,-0.910473751476987,
-2.49517783287065));
#24958=CARTESIAN_POINT('Ctrl Pts',(97.2646882657054,-0.860670680325778,
-2.49043221028096));
#24959=CARTESIAN_POINT('Ctrl Pts',(97.2793364466014,-0.846746143664709,
-2.48912964590121));
#24960=CARTESIAN_POINT('Ctrl Pts',(97.3043150722962,-0.821746952825859,
-2.48682533905843));
#24961=CARTESIAN_POINT('Ctrl Pts',(97.314803824049,-0.810836896909026,-2.48583041692453));
#24962=CARTESIAN_POINT('Ctrl Pts',(97.3298937954042,-0.79452290230653,-2.48435620485798));
#24963=CARTESIAN_POINT('Ctrl Pts',(97.3346613177015,-0.789274362364304,
-2.48388390996832));
#24964=CARTESIAN_POINT('Ctrl Pts',(97.3430199499101,-0.779903749603985,
-2.48304398486726));
#24965=CARTESIAN_POINT('Ctrl Pts',(97.3466303290093,-0.775799085697534,
-2.48267716611391));
#24966=CARTESIAN_POINT('Ctrl Pts',(97.3541458291074,-0.767133752321216,
-2.48190497617916));
#24967=CARTESIAN_POINT('Ctrl Pts',(97.3580449020178,-0.762568068983827,
-2.48149937305658));
#24968=CARTESIAN_POINT('Ctrl Pts',(97.3682316772607,-0.750453329889654,
-2.48042629140322));
#24969=CARTESIAN_POINT('Ctrl Pts',(97.3744600124358,-0.742855198855763,
-2.47975646042801));
#24970=CARTESIAN_POINT('Ctrl Pts',(97.4012576065385,-0.709316792701429,
-2.47681283682992));
#24971=CARTESIAN_POINT('Ctrl Pts',(97.4208211952784,-0.682595979410996,
-2.47450051388395));
#24972=CARTESIAN_POINT('Ctrl Pts',(97.4957537622936,-0.570641210241875,
-2.46493643583014));
#24973=CARTESIAN_POINT('Ctrl Pts',(97.5411051168979,-0.479236541255961,
-2.45735951257017));
#24974=CARTESIAN_POINT('Ctrl Pts',(97.5811851486512,-0.362744745057588,
-2.44845009689676));
#24975=CARTESIAN_POINT('Ctrl Pts',(97.5876499191631,-0.342128454431495,
-2.4469020651035));
#24976=CARTESIAN_POINT('Ctrl Pts',(97.5972420268341,-0.308306638459812,
-2.44442038685505));
#24977=CARTESIAN_POINT('Ctrl Pts',(97.6007146305804,-0.295204881632774,
-2.44347295933262));
#24978=CARTESIAN_POINT('Ctrl Pts',(97.6051028414988,-0.277414026042835,
-2.44220775933716));
#24979=CARTESIAN_POINT('Ctrl Pts',(97.6062170770942,-0.272775631939352,
-2.44187984385729));
#24980=CARTESIAN_POINT('Ctrl Pts',(97.6080285496197,-0.265027774515217,
-2.44133548468442));
#24981=CARTESIAN_POINT('Ctrl Pts',(97.60874139372,-0.261922066207795,-2.44111818331832));
#24982=CARTESIAN_POINT('Ctrl Pts',(97.6100669345032,-0.256037541028123,
-2.44070821035799));
#24983=CARTESIAN_POINT('Ctrl Pts',(97.6106821782182,-0.253259339857263,
-2.44051539241732));
#24984=CARTESIAN_POINT('Ctrl Pts',(97.6121150114231,-0.246676295779057,
-2.44006019145954));
#24985=CARTESIAN_POINT('Ctrl Pts',(97.6129238295065,-0.242869547020777,
-2.4397982966511));
#24986=CARTESIAN_POINT('Ctrl Pts',(97.6157122932551,-0.229417843759671,
-2.43887732551677));
#24987=CARTESIAN_POINT('Ctrl Pts',(97.6175899138848,-0.219751825293636,
-2.43822364210268));
#24988=CARTESIAN_POINT('Ctrl Pts',(97.6318464937271,-0.141101832452653,
-2.4329619885993));
#24989=CARTESIAN_POINT('Ctrl Pts',(97.6381680957031,-0.0711524774354224,
-2.42863335731764));
#24990=CARTESIAN_POINT('Ctrl Pts',(97.6383030814189,0.0805299389287755,
-2.41925057438884));
#24991=CARTESIAN_POINT('Ctrl Pts',(97.6299002013654,0.161884590980388,-2.41420906871187));
#24992=CARTESIAN_POINT('Ctrl Pts',(97.6099982017247,0.256792756807976,-2.4078889105746));
#24993=CARTESIAN_POINT('Ctrl Pts',(97.6065407504146,0.271807524029241,-2.40687633979508));
#24994=CARTESIAN_POINT('Ctrl Pts',(97.6010699376831,0.293601305789225,-2.40538597542467));
#24995=CARTESIAN_POINT('Ctrl Pts',(97.5992884016742,0.300437264602398,-2.40491551607905));
#24996=CARTESIAN_POINT('Ctrl Pts',(97.5960160250482,0.31254628200428,-2.4040766558953));
#24997=CARTESIAN_POINT('Ctrl Pts',(97.5945496662619,0.317825785811986,-2.40370904618093));
#24998=CARTESIAN_POINT('Ctrl Pts',(97.5914118184313,0.328825091880758,-2.40293916890459));
#24999=CARTESIAN_POINT('Ctrl Pts',(97.5897336564111,0.334542811963291,-2.40253669607429));
#25000=CARTESIAN_POINT('Ctrl Pts',(97.5852337036935,0.349455009413571,-2.40148094315736));
#25001=CARTESIAN_POINT('Ctrl Pts',(97.5823425979218,0.358627932482312,-2.40082544624442));
#25002=CARTESIAN_POINT('Ctrl Pts',(97.5685107475972,0.400708932075501,-2.39778952706867));
#25003=CARTESIAN_POINT('Ctrl Pts',(97.5562332357401,0.433156071046556,-2.39536624628245));
#25004=CARTESIAN_POINT('Ctrl Pts',(97.5156337119749,0.527629438455172,-2.38805827740896));
#25005=CARTESIAN_POINT('Ctrl Pts',(97.4833419703187,0.58778704486304,-2.38306170778515));
#25006=CARTESIAN_POINT('Ctrl Pts',(97.4312999513706,0.667330430498391,-2.37608704485976));
#25007=CARTESIAN_POINT('Ctrl Pts',(97.4157965552207,0.689341429891389,-2.37411511549226));
#25008=CARTESIAN_POINT('Ctrl Pts',(97.3930575780121,0.719382860231116,-2.37137929811483));
#25009=CARTESIAN_POINT('Ctrl Pts',(97.3864454226472,0.727874077618951,-2.37060084261849));
#25010=CARTESIAN_POINT('Ctrl Pts',(97.3629914327436,0.757156353660903,-2.36790095450983));
#25011=CARTESIAN_POINT('Ctrl Pts',(97.3455569049934,0.777464933731278,-2.36600081347821));
#25012=CARTESIAN_POINT('Ctrl Pts',(97.32325121528,0.801723709791192,-2.36371342182215));
#25013=CARTESIAN_POINT('Ctrl Pts',(97.3190222087448,0.806250797645612,-2.36328577202934));
#25014=CARTESIAN_POINT('Ctrl Pts',(97.3123238844396,0.813308782407185,-2.36261809377447));
#25015=CARTESIAN_POINT('Ctrl Pts',(97.3098786293201,0.815862208765486,-2.36237634422714));
#25016=CARTESIAN_POINT('Ctrl Pts',(97.3055118452146,0.82038125477079,-2.36194820581087));
#25017=CARTESIAN_POINT('Ctrl Pts',(97.3035949341689,0.822351157964499,-2.36176148184408));
#25018=CARTESIAN_POINT('Ctrl Pts',(97.2989916447623,0.827048687976497,-2.36131596266371));
#25019=CARTESIAN_POINT('Ctrl Pts',(97.2962988455441,0.829769946454978,-2.36105766686682));
#25020=CARTESIAN_POINT('Ctrl Pts',(97.2880960785796,0.837978958071862,-2.36027766604826));
#25021=CARTESIAN_POINT('Ctrl Pts',(97.2825448512507,0.843425447468989,-2.35975903230613));
#25022=CARTESIAN_POINT('Ctrl Pts',(97.233000190216,0.891081414489478,-2.35520654296209));
#25023=CARTESIAN_POINT('Ctrl Pts',(97.1858384366024,0.929876701316887,-2.3513959652217));
#25024=CARTESIAN_POINT('Ctrl Pts',(97.0576039709581,1.01964120048432,-2.34169016205082));
#25025=CARTESIAN_POINT('Ctrl Pts',(96.9729630635093,1.06469905205022,-2.33584668920782));
#25026=CARTESIAN_POINT('Ctrl Pts',(96.8703203451406,1.10423538820051,-2.3286663653343));
#25027=CARTESIAN_POINT('Ctrl Pts',(96.856733697695,1.10918341703275,-2.32771500340941));
#25028=CARTESIAN_POINT('Ctrl Pts',(96.8364738446412,1.11614197038542,-2.3262933521774));
#25029=CARTESIAN_POINT('Ctrl Pts',(96.8298680077757,1.11834554272876,-2.32582934932997));
#25030=CARTESIAN_POINT('Ctrl Pts',(96.8180570595007,1.12216937338215,-2.32499872089301));
#25031=CARTESIAN_POINT('Ctrl Pts',(96.8128594658271,1.12381233154201,-2.32463284336382));
#25032=CARTESIAN_POINT('Ctrl Pts',(96.8018491813494,1.12720878885444,-2.32385696782679));
#25033=CARTESIAN_POINT('Ctrl Pts',(96.7960339790446,1.12895353552237,-2.32344669939144));
#25034=CARTESIAN_POINT('Ctrl Pts',(96.7804778810286,1.1334900543463,-2.32234778301256));
#25035=CARTESIAN_POINT('Ctrl Pts',(96.7707141904808,1.13620115496903,-2.32165657463997));
#25036=CARTESIAN_POINT('Ctrl Pts',(96.7210795480756,1.14929583414746,-2.31813435583294));
#25037=CARTESIAN_POINT('Ctrl Pts',(96.6807227087198,1.15770696118784,-2.31524172957488));
#25038=CARTESIAN_POINT('Ctrl Pts',(96.5397754449183,1.17944642192583,-2.30503905919362));
#25039=CARTESIAN_POINT('Ctrl Pts',(96.4379756879237,1.181893222004,-2.29745394790259));
#25040=CARTESIAN_POINT('Ctrl Pts',(96.313164369762,1.16874869978967,-2.28844981335566));
#25041=CARTESIAN_POINT('Ctrl Pts',(96.2892815642239,1.16548987999856,-2.28674311631785));
#25042=CARTESIAN_POINT('Ctrl Pts',(96.2595927263151,1.1605063680388,-2.28465487241569));
#25043=CARTESIAN_POINT('Ctrl Pts',(96.2536792589954,1.15946719362418,-2.28424060371162));
#25044=CARTESIAN_POINT('Ctrl Pts',(96.2443395767925,1.15775220203899,-2.28358922677905));
#25045=CARTESIAN_POINT('Ctrl Pts',(96.2409080758883,1.15710630812177,-2.28335052820112));
#25046=CARTESIAN_POINT('Ctrl Pts',(96.2347735876527,1.15592337253678,-2.28292498609885));
#25047=CARTESIAN_POINT('Ctrl Pts',(96.2320696207874,1.15539210725295,-2.28273783173883));
#25048=CARTESIAN_POINT('Ctrl Pts',(96.2255515543974,1.15408768560123,-2.28228766210228));
#25049=CARTESIAN_POINT('Ctrl Pts',(96.2217393923493,1.15330510998306,-2.28202517741097));
#25050=CARTESIAN_POINT('Ctrl Pts',(96.2100051333279,1.15083557970825,-2.28121949679517));
#25051=CARTESIAN_POINT('Ctrl Pts',(96.2020963033408,1.14908574509046,-2.28067967563223));
#25052=CARTESIAN_POINT('Ctrl Pts',(96.1836346210007,1.14480083181942,-2.2794257286249));
#25053=CARTESIAN_POINT('Ctrl Pts',(96.1730973553807,1.14220117420704,-2.27871475992251));
#25054=CARTESIAN_POINT('Ctrl Pts',(96.1358084948056,1.13245288460476,-2.27621080742166));
#25055=CARTESIAN_POINT('Ctrl Pts',(96.1092732684615,1.12450660921455,-2.27445093206241));
#25056=CARTESIAN_POINT('Ctrl Pts',(96.0276435188413,1.09688968634833,-2.26903711044708));
#25057=CARTESIAN_POINT('Ctrl Pts',(95.9737502177826,1.07405810720824,-2.26545930969229));
#25058=CARTESIAN_POINT('Ctrl Pts',(95.9218015453623,1.04733927739527,-2.26182855819541));
#25059=CARTESIAN_POINT('',(97.6382309079769,0.000313031882164676,-2.32461928099262));
#25060=CARTESIAN_POINT('Ctrl Pts',(95.9218016761257,1.04733934465099,-2.16205147885552));
#25061=CARTESIAN_POINT('Ctrl Pts',(95.923776767422,1.04835519567381,-2.16219312880972));
#25062=CARTESIAN_POINT('Ctrl Pts',(95.9257548970161,1.0493655444312,-2.1623349385917));
#25063=CARTESIAN_POINT('Ctrl Pts',(95.9536565712311,1.06351719527435,-2.16433444469047));
#25064=CARTESIAN_POINT('Ctrl Pts',(95.9800529867209,1.07569908887628,-2.16621756057492));
#25065=CARTESIAN_POINT('Ctrl Pts',(96.0155274916952,1.09050422435866,-2.16875199961619));
#25066=CARTESIAN_POINT('Ctrl Pts',(96.0242263090449,1.09401321896232,-2.16937372951873));
#25067=CARTESIAN_POINT('Ctrl Pts',(96.0384698571873,1.09956199970929,-2.17039261553777));
#25068=CARTESIAN_POINT('Ctrl Pts',(96.043989772075,1.10166467231015,-2.17078767933817));
#25069=CARTESIAN_POINT('Ctrl Pts',(96.0546761099257,1.10564357043754,-2.17155301889669));
#25070=CARTESIAN_POINT('Ctrl Pts',(96.0598403193523,1.10752532990896,-2.17192310061477));
#25071=CARTESIAN_POINT('Ctrl Pts',(96.0718973938471,1.11182338141111,-2.17278777173518));
#25072=CARTESIAN_POINT('Ctrl Pts',(96.0787998786354,1.11421181431584,-2.17328325752817));
#25073=CARTESIAN_POINT('Ctrl Pts',(96.1011898151476,1.12172682992846,-2.17489228176829));
#25074=CARTESIAN_POINT('Ctrl Pts',(96.1167611047304,1.12659567828579,-2.17601407992511));
#25075=CARTESIAN_POINT('Ctrl Pts',(96.1538326898989,1.13734718185568,-2.17869269852132));
#25076=CARTESIAN_POINT('Ctrl Pts',(96.1754081486719,1.14294582308083,-2.18025788142672));
#25077=CARTESIAN_POINT('Ctrl Pts',(96.2598062163596,1.16230804930326,-2.18640468460287));
#25078=CARTESIAN_POINT('Ctrl Pts',(96.3235501720313,1.17152832806506,-2.19110657832467));
#25079=CARTESIAN_POINT('Ctrl Pts',(96.4510044990657,1.17941743096837,-2.20047865283491));
#25080=CARTESIAN_POINT('Ctrl Pts',(96.5145078386278,1.17821812116155,-2.20513196611785));
#25081=CARTESIAN_POINT('Ctrl Pts',(96.587561799582,1.17091653344803,-2.21028014466323));
#25082=CARTESIAN_POINT('Ctrl Pts',(96.5974999781431,1.16979522697559,-2.21097592148257));
#25083=CARTESIAN_POINT('Ctrl Pts',(96.6113279924709,1.1680563863511,-2.21193656108579));
#25084=CARTESIAN_POINT('Ctrl Pts',(96.6152305008229,1.16754577192768,-2.21220683914772));
#25085=CARTESIAN_POINT('Ctrl Pts',(96.6219607666877,1.16663082846654,-2.21267144165468));
#25086=CARTESIAN_POINT('Ctrl Pts',(96.6247897172272,1.16623576114777,-2.21286626533859));
#25087=CARTESIAN_POINT('Ctrl Pts',(96.6307579314682,1.16538014338993,-2.21327626417096));
#25088=CARTESIAN_POINT('Ctrl Pts',(96.6338968230044,1.1649171921021,-2.21349129814852));
#25089=CARTESIAN_POINT('Ctrl Pts',(96.641686312499,1.16373614794759,-2.21402352509463));
#25090=CARTESIAN_POINT('Ctrl Pts',(96.6463346128452,1.16300284750899,-2.21433988344908));
#25091=CARTESIAN_POINT('Ctrl Pts',(96.6638841034802,1.16012639345783,-2.2155300091557));
#25092=CARTESIAN_POINT('Ctrl Pts',(96.6767542519017,1.15779617615168,-2.21639406201771));
#25093=CARTESIAN_POINT('Ctrl Pts',(96.7097449234824,1.15125366473016,-2.21859260745331));
#25094=CARTESIAN_POINT('Ctrl Pts',(96.7297993863679,1.14672804503017,-2.21991335978148));
#25095=CARTESIAN_POINT('Ctrl Pts',(96.8057058485788,1.1274970906121,-2.22488733680801));
#25096=CARTESIAN_POINT('Ctrl Pts',(96.8605698145117,1.10921576668435,-2.22843325469929));
#25097=CARTESIAN_POINT('Ctrl Pts',(96.9834563742727,1.05795835245181,-2.23667773722027));
#25098=CARTESIAN_POINT('Ctrl Pts',(97.0500815666287,1.02232484078564,-2.24138643512437));
#25099=CARTESIAN_POINT('Ctrl Pts',(97.1215043092217,0.974808428180691,-2.247016312561));
#25100=CARTESIAN_POINT('Ctrl Pts',(97.1300913924227,0.968929923798267,-2.24770324335967));
#25101=CARTESIAN_POINT('Ctrl Pts',(97.1441021119463,0.959063328402978,-2.24884141115399));
#25102=CARTESIAN_POINT('Ctrl Pts',(97.149571572297,0.955141074422934,-2.24929017742411));
#25103=CARTESIAN_POINT('Ctrl Pts',(97.1592826016369,0.948050283836848,-2.25009512827424));
#25104=CARTESIAN_POINT('Ctrl Pts',(97.1635370235418,0.944899595143934,-2.25045062451046));
#25105=CARTESIAN_POINT('Ctrl Pts',(97.1679704359065,0.941569833878451,-2.25082411290007));
#25106=CARTESIAN_POINT('Ctrl Pts',(97.1681708235175,0.941419230554903,-2.25084100088488));
#25107=CARTESIAN_POINT('Ctrl Pts',(97.1684691668083,0.941194858570143,-2.25086615397441));
#25108=CARTESIAN_POINT('Ctrl Pts',(97.1685671591592,0.941121138502763,-2.25087441719745));
#25109=CARTESIAN_POINT('Ctrl Pts',(97.1688499985442,0.940908288033998,-2.25089827219897));
#25110=CARTESIAN_POINT('Ctrl Pts',(97.1690348160209,0.940769118526424,-2.25091386549126));
#25111=CARTESIAN_POINT('Ctrl Pts',(97.1693844352018,0.940505690131086,-2.25094337387004));
#25112=CARTESIAN_POINT('Ctrl Pts',(97.1695492453095,0.940381442334309,-2.25095728852732));
#25113=CARTESIAN_POINT('Ctrl Pts',(97.1698622988547,0.940145307009476,-2.25098372758335));
#25114=CARTESIAN_POINT('Ctrl Pts',(97.1700105485751,0.94003342767192,-2.25099625166744));
#25115=CARTESIAN_POINT('Ctrl Pts',(97.1702931590239,0.939820045634109,-2.25102013336215));
#25116=CARTESIAN_POINT('Ctrl Pts',(97.1704275243918,0.939718549228576,-2.25103149072401));
#25117=CARTESIAN_POINT('Ctrl Pts',(97.1706844805693,0.939524364072526,-2.25105321585586));
#25118=CARTESIAN_POINT('Ctrl Pts',(97.1708070751032,0.939431680067642,-2.25106358344609));
#25119=CARTESIAN_POINT('Ctrl Pts',(97.1710421855001,0.939253859407281,-2.25108347102667));
#25120=CARTESIAN_POINT('Ctrl Pts',(97.171154704097,0.939168726611208,-2.25109299086033));
#25121=CARTESIAN_POINT('Ctrl Pts',(97.171371039975,0.939004983390202,-2.25111129834054));
#25122=CARTESIAN_POINT('Ctrl Pts',(97.1714748595427,0.938926375947189,-2.25112008587203));
#25123=CARTESIAN_POINT('Ctrl Pts',(97.1716749296677,0.938774839759563,-2.25113702369568));
#25124=CARTESIAN_POINT('Ctrl Pts',(97.1717711820611,0.93870191341848,-2.25114517389478));
#25125=CARTESIAN_POINT('Ctrl Pts',(97.1719570583077,0.938561037895266,-2.25116091596767));
#25126=CARTESIAN_POINT('Ctrl Pts',(97.1720466836554,0.938493090669798,-2.25116850776564));
#25127=CARTESIAN_POINT('Ctrl Pts',(97.1722200941324,0.938361584714113,-2.25118319922394));
#25128=CARTESIAN_POINT('Ctrl Pts',(97.1723038805654,0.93829802753639,-2.25119029882822));
#25129=CARTESIAN_POINT('Ctrl Pts',(97.1724662798504,0.938174803389857,-2.25120406190202));
#25130=CARTESIAN_POINT('Ctrl Pts',(97.1725448937546,0.938115137732225,-2.25121072532245));
#25131=CARTESIAN_POINT('Ctrl Pts',(97.1726975160203,0.937999271651833,-2.2512236637736));
#25132=CARTESIAN_POINT('Ctrl Pts',(97.1727715252011,0.937943072373122,-2.25122993875799));
#25133=CARTESIAN_POINT('Ctrl Pts',(97.1729154252949,0.937833774190707,-2.25124214131381));
#25134=CARTESIAN_POINT('Ctrl Pts',(97.1729853169115,0.937780676242318,-2.25124806884723));
#25135=CARTESIAN_POINT('Ctrl Pts',(97.1783526532904,0.93370206553356,-2.25170333666591));
#25136=CARTESIAN_POINT('Ctrl Pts',(97.1836158009689,0.929631816222444,-2.25215441206328));
#25137=CARTESIAN_POINT('Ctrl Pts',(97.1948067862384,0.920824739924879,-2.2531236686561));
#25138=CARTESIAN_POINT('Ctrl Pts',(97.2007238741347,0.916074802631856,-2.25364235293484));
#25139=CARTESIAN_POINT('Ctrl Pts',(97.2163195049459,0.903305660609151,-2.25502623790589));
#25140=CARTESIAN_POINT('Ctrl Pts',(97.2259160537355,0.895188314618927,-2.25589528334289));
#25141=CARTESIAN_POINT('Ctrl Pts',(97.2867901785082,0.842002709301719,-2.26152316361044));
#25142=CARTESIAN_POINT('Ctrl Pts',(97.334189277498,0.792708395767236,-2.26645253863819));
#25143=CARTESIAN_POINT('Ctrl Pts',(97.427157567031,0.677494612334315,-2.27729371065023));
#25144=CARTESIAN_POINT('Ctrl Pts',(97.4708304130329,0.610457633925246,-2.28320537883991));
#25145=CARTESIAN_POINT('Ctrl Pts',(97.5117503363909,0.531053985602217,-2.28945910929593));
#25146=CARTESIAN_POINT('Ctrl Pts',(97.5160079870279,0.522540282547612,-2.29012042956892));
#25147=CARTESIAN_POINT('Ctrl Pts',(97.5217947533331,0.510609506677832,-2.29103349392651));
#25148=CARTESIAN_POINT('Ctrl Pts',(97.5234113686458,0.507235629201593,-2.29129018879512));
#25149=CARTESIAN_POINT('Ctrl Pts',(97.5263334129011,0.501062002969849,-2.29175707317118));
#25150=CARTESIAN_POINT('Ctrl Pts',(97.5276439553577,0.498264713145047,-2.29196756701761));
#25151=CARTESIAN_POINT('Ctrl Pts',(97.5303385477354,0.492453834099509,-2.29240260844135));
#25152=CARTESIAN_POINT('Ctrl Pts',(97.5317208947603,0.489439515760631,-2.29262705408531));
#25153=CARTESIAN_POINT('Ctrl Pts',(97.5353068796261,0.48153201445163,-2.2932127437687));
#25154=CARTESIAN_POINT('Ctrl Pts',(97.5374898688845,0.476629469623854,-2.2935727674455));
#25155=CARTESIAN_POINT('Ctrl Pts',(97.5471555366222,0.454516856476531,-2.29518350425007));
#25156=CARTESIAN_POINT('Ctrl Pts',(97.5542602160511,0.437143275807816,-2.29641346038068));
#25157=CARTESIAN_POINT('Ctrl Pts',(97.5733543660441,0.38706663788295,-2.29987837637098));
#25158=CARTESIAN_POINT('Ctrl Pts',(97.584313251963,0.353990310149442,-2.30207142337862));
#25159=CARTESIAN_POINT('Ctrl Pts',(97.6059723893391,0.277396073812628,-2.30703395720238));
#25160=CARTESIAN_POINT('Ctrl Pts',(97.6156880700367,0.233657523860515,-2.30978598829603));
#25161=CARTESIAN_POINT('Ctrl Pts',(97.6330852460752,0.126925754816465,-2.31649823683831));
#25162=CARTESIAN_POINT('Ctrl Pts',(97.6382140687699,0.0636688003235982,
-2.32047834256884));
#25163=CARTESIAN_POINT('Ctrl Pts',(97.6382309079769,0.000313031882164676,
-2.32461928099262));
#25164=CARTESIAN_POINT('Ctrl Pts',(97.6382309082176,0.000312125111502949,
-2.32461934025923));
#25165=CARTESIAN_POINT('Ctrl Pts',(97.6382328579085,-0.0070446953100704,
-2.32510018283114));
#25166=CARTESIAN_POINT('Ctrl Pts',(97.6381658759582,-0.0144012708024564,
-2.32558298598406));
#25167=CARTESIAN_POINT('Ctrl Pts',(97.6379025479175,-0.0286535485738951,
-2.32652247595264));
#25168=CARTESIAN_POINT('Ctrl Pts',(97.6377145311526,-0.0355490813513412,
-2.32697889396367));
#25169=CARTESIAN_POINT('Ctrl Pts',(97.6372714975406,-0.0478349875681682,
-2.32779564503261));
#25170=CARTESIAN_POINT('Ctrl Pts',(97.6370399857497,-0.053226051780862,
-2.32815525229364));
#25171=CARTESIAN_POINT('Ctrl Pts',(97.636513796166,-0.0637856193376086,
-2.32886209862418));
#25172=CARTESIAN_POINT('Ctrl Pts',(97.6362220711656,-0.0689541517168208,
-2.32920923895953));
#25173=CARTESIAN_POINT('Ctrl Pts',(97.635530697521,-0.0799180676014652,
-2.32994817268879));
#25174=CARTESIAN_POINT('Ctrl Pts',(97.6351222277693,-0.0857127362598701,
-2.33034022983032));
#25175=CARTESIAN_POINT('Ctrl Pts',(97.6339773990083,-0.100403302701495,
-2.33133812831642));
#25176=CARTESIAN_POINT('Ctrl Pts',(97.6331827530157,-0.109294156422362,
-2.33194575564432));
#25177=CARTESIAN_POINT('Ctrl Pts',(97.6297339128789,-0.143492381775446,
-2.33429770114478));
#25178=CARTESIAN_POINT('Ctrl Pts',(97.6263610501183,-0.168718626095907,
-2.33606394816952));
#25179=CARTESIAN_POINT('Ctrl Pts',(97.605738354346,-0.292327926404079,-2.34487953628559));
#25180=CARTESIAN_POINT('Ctrl Pts',(97.5768390992368,-0.3883406980941,-2.3522810097997));
#25181=CARTESIAN_POINT('Ctrl Pts',(97.5243954119919,-0.505983868348584,
-2.36166852019092));
#25182=CARTESIAN_POINT('Ctrl Pts',(97.5116322941545,-0.531991290739224,
-2.36376180114208));
#25183=CARTESIAN_POINT('Ctrl Pts',(97.4900569622962,-0.572140194747069,
-2.36699626033148));
#25184=CARTESIAN_POINT('Ctrl Pts',(97.4818819679298,-0.586609919678346,
-2.3681625352486));
#25185=CARTESIAN_POINT('Ctrl Pts',(97.470779240575,-0.60532542534575,-2.36966721114221));
#25186=CARTESIAN_POINT('Ctrl Pts',(97.468126495448,-0.609731058494446,-2.37002112812063));
#25187=CARTESIAN_POINT('Ctrl Pts',(97.4637415386422,-0.616906738803622,
-2.37059692886359));
#25188=CARTESIAN_POINT('Ctrl Pts',(97.4620265427629,-0.619687146376543,
-2.37081987905521));
#25189=CARTESIAN_POINT('Ctrl Pts',(97.4586518996869,-0.625107623264932,
-2.37125416006126));
#25190=CARTESIAN_POINT('Ctrl Pts',(97.4569933053892,-0.627748286632585,
-2.37146555134721));
#25191=CARTESIAN_POINT('Ctrl Pts',(97.4532603752451,-0.633639442071233,
-2.37193683121053));
#25192=CARTESIAN_POINT('Ctrl Pts',(97.4511805051736,-0.636886427990322,
-2.37219636370014));
#25193=CARTESIAN_POINT('Ctrl Pts',(97.4439053656858,-0.648122124710818,
-2.37309388787792));
#25194=CARTESIAN_POINT('Ctrl Pts',(97.4386289493937,-0.656058210334721,
-2.37372686696199));
#25195=CARTESIAN_POINT('Ctrl Pts',(97.3906637980103,-0.726335728807615,
-2.37933184282137));
#25196=CARTESIAN_POINT('Ctrl Pts',(97.3421581806821,-0.784507662320379,
-2.38397629970982));
#25197=CARTESIAN_POINT('Ctrl Pts',(97.2373985954766,-0.88805270252227,-2.39308791372061));
#25198=CARTESIAN_POINT('Ctrl Pts',(97.1818984494767,-0.933699035627461,
-2.39753581569024));
#25199=CARTESIAN_POINT('Ctrl Pts',(97.1120342595478,-0.981191326117177,
-2.40301298316904));
#25200=CARTESIAN_POINT('Ctrl Pts',(97.1013576392536,-0.988197947380445,
-2.40384654789385));
#25201=CARTESIAN_POINT('Ctrl Pts',(97.084090333313,-0.999132229586126,-2.40519059967739));
#25202=CARTESIAN_POINT('Ctrl Pts',(97.0775713607598,-1.00317161821522,-2.40569711158367));
#25203=CARTESIAN_POINT('Ctrl Pts',(97.0651127805488,-1.01072401052339,-2.40666370213664));
#25204=CARTESIAN_POINT('Ctrl Pts',(97.0591808198162,-1.01424905149447,-2.40712332843813));
#25205=CARTESIAN_POINT('Ctrl Pts',(97.0485760879944,-1.02042541675402,-2.40794413195134));
#25206=CARTESIAN_POINT('Ctrl Pts',(97.0439154683067,-1.02309729924003,-2.40830456293504));
#25207=CARTESIAN_POINT('Ctrl Pts',(97.0340541162283,-1.0286614099814,-2.40906665303262));
#25208=CARTESIAN_POINT('Ctrl Pts',(97.0288494310593,-1.03154628636073,-2.40946855961641));
#25209=CARTESIAN_POINT('Ctrl Pts',(97.0152078034377,-1.03897304531625,-2.41052127933083));
#25210=CARTESIAN_POINT('Ctrl Pts',(97.0067370455216,-1.0434515511149,-2.41117428619939));
#25211=CARTESIAN_POINT('Ctrl Pts',(96.9707237959743,-1.06193312114183,-2.41394835536683));
#25212=CARTESIAN_POINT('Ctrl Pts',(96.9426927294797,-1.07495172503206,-2.41610269288748));
#25213=CARTESIAN_POINT('Ctrl Pts',(96.8181518184083,-1.12694097816416,-2.42565966814911));
#25214=CARTESIAN_POINT('Ctrl Pts',(96.7172339855009,-1.15412158665157,-2.4334200967969));
#25215=CARTESIAN_POINT('Ctrl Pts',(96.5925134182985,-1.17052804421296,-2.44251948849054));
#25216=CARTESIAN_POINT('Ctrl Pts',(96.5708653584615,-1.17276761245956,-2.44407912058409));
#25217=CARTESIAN_POINT('Ctrl Pts',(96.5355825280345,-1.17543200157612,-2.44657718529343));
#25218=CARTESIAN_POINT('Ctrl Pts',(96.5219810955612,-1.17622209186339,-2.44752961105701));
#25219=CARTESIAN_POINT('Ctrl Pts',(96.5035929673586,-1.17697037263742,-2.44880033320075));
#25220=CARTESIAN_POINT('Ctrl Pts',(96.4988163838866,-1.17713563389972,-2.44912888370799));
#25221=CARTESIAN_POINT('Ctrl Pts',(96.4908520013777,-1.17736265687577,-2.44967399475973));
#25222=CARTESIAN_POINT('Ctrl Pts',(96.4876647669246,-1.17744055789687,-2.44989141796297));
#25223=CARTESIAN_POINT('Ctrl Pts',(96.4816341644796,-1.1775634548524,-2.45030139095582));
#25224=CARTESIAN_POINT('Ctrl Pts',(96.4787908905804,-1.1776110967558,-2.45049408853775));
#25225=CARTESIAN_POINT('Ctrl Pts',(96.4720628814343,-1.17769945813993,-2.4509487200334));
#25226=CARTESIAN_POINT('Ctrl Pts',(96.4681780322624,-1.17773125577461,-2.45121016857687));
#25227=CARTESIAN_POINT('Ctrl Pts',(96.4544881023195,-1.17777556685114,-2.45212797565867));
#25228=CARTESIAN_POINT('Ctrl Pts',(96.4446827688482,-1.17768486147239,-2.45277898968393));
#25229=CARTESIAN_POINT('Ctrl Pts',(96.3638539789832,-1.17592741086032,-2.45810150107689));
#25230=CARTESIAN_POINT('Ctrl Pts',(96.2931036554623,-1.16795963376462,-2.46248557709005));
#25231=CARTESIAN_POINT('Ctrl Pts',(96.165767767085,-1.14180220629355,-2.47052650241691));
#25232=CARTESIAN_POINT('Ctrl Pts',(96.1090157398355,-1.12562857411263,-2.4741683301309));
#25233=CARTESIAN_POINT('Ctrl Pts',(96.0337888096943,-1.09794339272785,-2.47927749036081));
#25234=CARTESIAN_POINT('Ctrl Pts',(96.0140658993834,-1.09007311602649,-2.48064399574213));
#25235=CARTESIAN_POINT('Ctrl Pts',(95.980129844637,-1.0754557133577,-2.48305097963976));
#25236=CARTESIAN_POINT('Ctrl Pts',(95.9658189104747,-1.06894883161682,-2.48408374056681));
#25237=CARTESIAN_POINT('Ctrl Pts',(95.9451517104817,-1.05904799011359,-2.48560343926336));
#25238=CARTESIAN_POINT('Ctrl Pts',(95.9386891680595,-1.05587887701475,-2.48608273622605));
#25239=CARTESIAN_POINT('Ctrl Pts',(95.9273576121539,-1.05019265287333,-2.48693059109396));
#25240=CARTESIAN_POINT('Ctrl Pts',(95.9224763166676,-1.04770039338141,-2.48729828353467));
#25241=CARTESIAN_POINT('Ctrl Pts',(95.9123302760931,-1.04243049319861,-2.48806779815115));
#25242=CARTESIAN_POINT('Ctrl Pts',(95.9070688499076,-1.0396468341165,-2.48846982197968));
#25243=CARTESIAN_POINT('Ctrl Pts',(95.8933868366295,-1.03227481177002,-2.48952319108248));
#25244=CARTESIAN_POINT('Ctrl Pts',(95.8850009326934,-1.02762335546255,-2.49017673510176));
#25245=CARTESIAN_POINT('Ctrl Pts',(95.8497748040735,-1.00751787561376,-2.49295642419129));
#25246=CARTESIAN_POINT('Ctrl Pts',(95.8234950375911,-0.991111955026462,
-2.49511601383429));
#25247=CARTESIAN_POINT('Ctrl Pts',(95.7292249391886,-0.926962110574596,
-2.50319149766311));
#25248=CARTESIAN_POINT('Ctrl Pts',(95.6656985624145,-0.873104640273444,
-2.50931367745915));
#25249=CARTESIAN_POINT('Ctrl Pts',(95.5723750103773,-0.775295018995918,
-2.51920970710001));
#25250=CARTESIAN_POINT('Ctrl Pts',(95.5389169839887,-0.735211318289734,
-2.52299307191744));
#25251=CARTESIAN_POINT('Ctrl Pts',(95.5041291478889,-0.687411596383303,
-2.52710491508794));
#25252=CARTESIAN_POINT('Ctrl Pts',(95.5000847807433,-0.681749716665959,
-2.52758595499823));
#25253=CARTESIAN_POINT('Ctrl Pts',(95.4939889751718,-0.673054033451855,
-2.52831523465734));
#25254=CARTESIAN_POINT('Ctrl Pts',(95.4919011998323,-0.670046071428197,
-2.52856578726807));
#25255=CARTESIAN_POINT('Ctrl Pts',(95.4881045419205,-0.664521210047747,
-2.52902278588614));
#25256=CARTESIAN_POINT('Ctrl Pts',(95.4863913761397,-0.66200741698106,-2.5292295077953));
#25257=CARTESIAN_POINT('Ctrl Pts',(95.4825454750405,-0.656316927258143,
-2.52969475769526));
#25258=CARTESIAN_POINT('Ctrl Pts',(95.4804184666913,-0.653136457438748,
-2.52995290741091));
#25259=CARTESIAN_POINT('Ctrl Pts',(95.4749605094935,-0.644888592663324,
-2.5306176686929));
#25260=CARTESIAN_POINT('Ctrl Pts',(95.4716530806006,-0.639805661216511,
-2.53102279577577));
#25261=CARTESIAN_POINT('Ctrl Pts',(95.4497003870847,-0.605491383199052,
-2.53372899480658));
#25262=CARTESIAN_POINT('Ctrl Pts',(95.4323125595053,-0.575471483685733,
-2.53595740401788));
#25263=CARTESIAN_POINT('Ctrl Pts',(95.4031992262114,-0.519662836059172,
-2.53993469764894));
#25264=CARTESIAN_POINT('Ctrl Pts',(95.3910312076051,-0.494137102975158,
-2.54169473144999));
#25265=CARTESIAN_POINT('Ctrl Pts',(95.360659664446,-0.42403385263733,-2.54643153055104));
#25266=CARTESIAN_POINT('Ctrl Pts',(95.3442517499036,-0.378739812221549,
-2.54939129353727));
#25267=CARTESIAN_POINT('Ctrl Pts',(95.3156641840501,-0.281620848485254,
-2.55572323273594));
#25268=CARTESIAN_POINT('Ctrl Pts',(95.3041322544921,-0.229722334389208,
-2.55909997911316));
#25269=CARTESIAN_POINT('Ctrl Pts',(95.294513387777,-0.166528721727784,-2.56330124523728));
#25270=CARTESIAN_POINT('Ctrl Pts',(95.2930325292862,-0.155808676108142,
-2.56401683801274));
#25271=CARTESIAN_POINT('Ctrl Pts',(95.2909334234786,-0.138896874160968,
-2.56515099415849));
#25272=CARTESIAN_POINT('Ctrl Pts',(95.2902161383819,-0.132717845932983,
-2.56556647569134));
#25273=CARTESIAN_POINT('Ctrl Pts',(95.2889646255899,-0.121136426956502,
-2.5663474019905));
#25274=CARTESIAN_POINT('Ctrl Pts',(95.2884187339504,-0.115735441049098,
-2.56671247401288));
#25275=CARTESIAN_POINT('Ctrl Pts',(95.2872798936071,-0.10363212047389,-2.56753265851575));
#25276=CARTESIAN_POINT('Ctrl Pts',(95.2867070073179,-0.0969281349678226,
-2.56798838051139));
#25277=CARTESIAN_POINT('Ctrl Pts',(95.2853949601245,-0.0798506832053449,
-2.56915305861647));
#25278=CARTESIAN_POINT('Ctrl Pts',(95.2847357112633,-0.0694718416145498,
-2.56986445233853));
#25279=CARTESIAN_POINT('Ctrl Pts',(95.2804512557265,0.0158219819775928,
-2.57574139306761));
#25280=CARTESIAN_POINT('Ctrl Pts',(95.2838531182857,0.0909040437030932,
-2.58112567076266));
#25281=CARTESIAN_POINT('Ctrl Pts',(95.3023252624909,0.221342520139699,-2.59076127423558));
#25282=CARTESIAN_POINT('Ctrl Pts',(95.3143371025519,0.276896359071611,-2.59495309411392));
#25283=CARTESIAN_POINT('Ctrl Pts',(95.3363379791686,0.351933121332829,-2.60060695087666));
#25284=CARTESIAN_POINT('Ctrl Pts',(95.3429282397361,0.372331024498018,-2.60214245785198));
#25285=CARTESIAN_POINT('Ctrl Pts',(95.3545633279369,0.405244217262078,-2.60460638724446));
#25286=CARTESIAN_POINT('Ctrl Pts',(95.3592727510937,0.417872233818749,-2.60554836432131));
#25287=CARTESIAN_POINT('Ctrl Pts',(95.3659375997813,0.434847758131694,-2.6068075016658));
#25288=CARTESIAN_POINT('Ctrl Pts',(95.3677039495857,0.439267740196754,-2.60713468484315));
#25289=CARTESIAN_POINT('Ctrl Pts',(95.3706965497113,0.446626423539653,-2.60767814929998));
#25290=CARTESIAN_POINT('Ctrl Pts',(95.3719079920369,0.449571036920018,-2.6078952826766));
#25291=CARTESIAN_POINT('Ctrl Pts',(95.3742252043801,0.455139125218332,-2.60830518169485));
#25292=CARTESIAN_POINT('Ctrl Pts',(95.375328566857,0.45776355686469,-2.60849809210146));
#25293=CARTESIAN_POINT('Ctrl Pts',(95.3779651962993,0.463971875309042,-2.60895381151797));
#25294=CARTESIAN_POINT('Ctrl Pts',(95.3795067728294,0.467552229648226,-2.60921612950088));
#25295=CARTESIAN_POINT('Ctrl Pts',(95.3849880336732,0.480110584928407,-2.61013470541584));
#25296=CARTESIAN_POINT('Ctrl Pts',(95.3890221500025,0.489047280012529,-2.61078562895274));
#25297=CARTESIAN_POINT('Ctrl Pts',(95.4229388507302,0.561747333333516,-2.61606664403242));
#25298=CARTESIAN_POINT('Ctrl Pts',(95.458377692013,0.622772423237232,-2.62041455649931));
#25299=CARTESIAN_POINT('Ctrl Pts',(95.5333492036738,0.728728680572336,-2.62844347473014));
#25300=CARTESIAN_POINT('Ctrl Pts',(95.5712481517739,0.774521230711589,-2.63211043686631));
#25301=CARTESIAN_POINT('Ctrl Pts',(95.6272298861611,0.832611710990445,-2.63725167452129));
#25302=CARTESIAN_POINT('Ctrl Pts',(95.642437433484,0.847557856606306,-2.6386236303474));
#25303=CARTESIAN_POINT('Ctrl Pts',(95.6695843969974,0.872826661600905,-2.64103934413662));
#25304=CARTESIAN_POINT('Ctrl Pts',(95.6813413797738,0.88333755192203,-2.64207530523385));
#25305=CARTESIAN_POINT('Ctrl Pts',(95.6987734593957,0.898303233211234,-2.64359884681239));
#25306=CARTESIAN_POINT('Ctrl Pts',(95.704284376056,0.902947250802624,-2.6440787306028));
#25307=CARTESIAN_POINT('Ctrl Pts',(95.7140617548011,0.911034302726085,-2.64492725624785));
#25308=CARTESIAN_POINT('Ctrl Pts',(95.7183103254208,0.914498703105236,-2.6452950281109));
#25309=CARTESIAN_POINT('Ctrl Pts',(95.7272190317424,0.921660135802268,-2.64606434506589));
#25310=CARTESIAN_POINT('Ctrl Pts',(95.7318832895431,0.925351767507479,-2.64646608938068));
#25311=CARTESIAN_POINT('Ctrl Pts',(95.7441247993499,0.934890652292875,-2.64751791027447));
#25312=CARTESIAN_POINT('Ctrl Pts',(95.7517455881633,0.940681053183735,-2.64817017366798));
#25313=CARTESIAN_POINT('Ctrl Pts',(95.7841816981849,0.964708639548181,-2.65093646461017));
#25314=CARTESIAN_POINT('Ctrl Pts',(95.8096347580536,0.982060268160886,-2.65308353366401));
#25315=CARTESIAN_POINT('Ctrl Pts',(95.8637460938545,1.01592042387009,-2.65760328689503));
#25316=CARTESIAN_POINT('Ctrl Pts',(95.8924610368534,1.03224854876223,-2.65997758591606));
#25317=CARTESIAN_POINT('Ctrl Pts',(95.9218019448244,1.04733948285108,-2.66237442964626));
#25318=CARTESIAN_POINT('Origin',(96.460480949577,-7.19464945638997E-16,
0.924367114736168));
#25319=CARTESIAN_POINT('',(95.9218016227097,1.04733931717749,-3.26242343814143));
#25320=CARTESIAN_POINT('',(95.9218016730922,1.04733934309078,-3.1639039911222));
#25321=CARTESIAN_POINT('',(95.9218016730721,1.04733934308042,0.924367114736168));
#25322=CARTESIAN_POINT('',(97.6382307847678,0.000623063363894689,-2.92357187405869));
#25323=CARTESIAN_POINT('Ctrl Pts',(95.9218016227097,1.04733931717749,-3.26242343814143));
#25324=CARTESIAN_POINT('Ctrl Pts',(95.9009760917006,1.03662809604634,-3.26076286007084));
#25325=CARTESIAN_POINT('Ctrl Pts',(95.8804699490475,1.02529568575856,-3.25908386593059));
#25326=CARTESIAN_POINT('Ctrl Pts',(95.8190575962219,0.988923619110589,-3.25392504421716));
#25327=CARTESIAN_POINT('Ctrl Pts',(95.7793366824058,0.961995788508946,-3.25040383841714));
#25328=CARTESIAN_POINT('Ctrl Pts',(95.7190393102272,0.915507724612175,-3.24481773703771));
#25329=CARTESIAN_POINT('Ctrl Pts',(95.6973338528679,0.897494680329055,-3.2427526516122));
#25330=CARTESIAN_POINT('Ctrl Pts',(95.6504413182246,0.855646906630459,-3.2381957699274));
#25331=CARTESIAN_POINT('Ctrl Pts',(95.6256154274532,0.831442053819478,-3.23571646123758));
#25332=CARTESIAN_POINT('Ctrl Pts',(95.597740441082,0.80175472839589,-3.23288598710055));
#25333=CARTESIAN_POINT('Ctrl Pts',(95.5936239825375,0.797302221286391,-3.23246673579861));
#25334=CARTESIAN_POINT('Ctrl Pts',(95.5869663858731,0.78998861300894,-3.23178689019993));
#25335=CARTESIAN_POINT('Ctrl Pts',(95.5844045401873,0.787146636680469,-3.23152484589805));
#25336=CARTESIAN_POINT('Ctrl Pts',(95.5798305899478,0.782022545901661,-3.23105627563974));
#25337=CARTESIAN_POINT('Ctrl Pts',(95.5778134428252,0.779745081021927,-3.23084938587444));
#25338=CARTESIAN_POINT('Ctrl Pts',(95.5733876777384,0.774708977634497,-3.23039490982893));
#25339=CARTESIAN_POINT('Ctrl Pts',(95.5709830891129,0.771946908867547,-3.23014761525407));
#25340=CARTESIAN_POINT('Ctrl Pts',(95.5640461349075,0.763903215082586,-3.22943296454969));
#25341=CARTESIAN_POINT('Ctrl Pts',(95.5595475577722,0.758592465210856,-3.22896797122995));
#25342=CARTESIAN_POINT('Ctrl Pts',(95.5216904385475,0.713088816751232,-3.2250384880526));
#25343=CARTESIAN_POINT('Ctrl Pts',(95.4909881354004,0.670752141001989,-3.22174071775077));
#25344=CARTESIAN_POINT('Ctrl Pts',(95.4188978841364,0.555998318018275,-3.21329928564867));
#25345=CARTESIAN_POINT('Ctrl Pts',(95.3822055789524,0.480989855424195,-3.20823192923778));
#25346=CARTESIAN_POINT('Ctrl Pts',(95.3432271524176,0.373874971906024,-3.20096082772322));
#25347=CARTESIAN_POINT('Ctrl Pts',(95.3338575705051,0.344612898304213,-3.19897354107816));
#25348=CARTESIAN_POINT('Ctrl Pts',(95.3230849535697,0.305805270613128,-3.19631922653434));
#25349=CARTESIAN_POINT('Ctrl Pts',(95.3206394455921,0.2965600313548,-3.19568555131755));
#25350=CARTESIAN_POINT('Ctrl Pts',(95.3168562027863,0.28151885953178,-3.19465199077159));
#25351=CARTESIAN_POINT('Ctrl Pts',(95.315449281176,0.275740649721048,-3.19425431490897));
#25352=CARTESIAN_POINT('Ctrl Pts',(95.3128294174555,0.264614980481494,-3.19348729673279));
#25353=CARTESIAN_POINT('Ctrl Pts',(95.3116099371108,0.259269207671798,-3.1931181729186));
#25354=CARTESIAN_POINT('Ctrl Pts',(95.3088730659749,0.246873150826158,-3.19226079534717));
#25355=CARTESIAN_POINT('Ctrl Pts',(95.3073830282832,0.239817117983475,-3.19177169192591));
#25356=CARTESIAN_POINT('Ctrl Pts',(95.302836575262,0.217264893233611,-3.19020478121577));
#25357=CARTESIAN_POINT('Ctrl Pts',(95.3000271514698,0.201721272374442,-3.18911930717782));
#25358=CARTESIAN_POINT('Ctrl Pts',(95.2941550211021,0.16503121145522,-3.18654293645155));
#25359=CARTESIAN_POINT('Ctrl Pts',(95.2913535897483,0.143849193209018,-3.18504451335201));
#25360=CARTESIAN_POINT('Ctrl Pts',(95.2829278751971,0.0633503072499742,
-3.17930799981127));
#25361=CARTESIAN_POINT('Ctrl Pts',(95.2812315076657,0.00371783528771251,
-3.17496672243804));
#25362=CARTESIAN_POINT('Ctrl Pts',(95.2873728046181,-0.125804141840988,
-3.1654540281797));
#25363=CARTESIAN_POINT('Ctrl Pts',(95.2969385670497,-0.195397804555561,
-3.16028863476569));
#25364=CARTESIAN_POINT('Ctrl Pts',(95.3148434238025,-0.273325084522133,
-3.15468427401297));
#25365=CARTESIAN_POINT('Ctrl Pts',(95.3171677595946,-0.28289027499488,-3.15399970271783));
#25366=CARTESIAN_POINT('Ctrl Pts',(95.3205783322454,-0.296196282563135,
-3.15305310770803));
#25367=CARTESIAN_POINT('Ctrl Pts',(95.3215635368278,-0.299962235651212,
-3.15278583758001));
#25368=CARTESIAN_POINT('Ctrl Pts',(95.3233012739676,-0.30647274902815,-3.15232497839477));
#25369=CARTESIAN_POINT('Ctrl Pts',(95.3240451083059,-0.309219565406145,
-3.1521309084276));
#25370=CARTESIAN_POINT('Ctrl Pts',(95.3256428422465,-0.315036004237455,
-3.15172078276427));
#25371=CARTESIAN_POINT('Ctrl Pts',(95.3264992573036,-0.318104913374181,
-3.15150487737429));
#25372=CARTESIAN_POINT('Ctrl Pts',(95.3286685605038,-0.325758376053264,
-3.1509675695998));
#25373=CARTESIAN_POINT('Ctrl Pts',(95.3299968761097,-0.330338561496088,
-3.15064703683849));
#25374=CARTESIAN_POINT('Ctrl Pts',(95.3352037756991,-0.347893261053726,
-3.14942197537411));
#25375=CARTESIAN_POINT('Ctrl Pts',(95.3392783750749,-0.360809180432816,
-3.14852791026801));
#25376=CARTESIAN_POINT('Ctrl Pts',(95.350420467529,-0.394114631164175,-3.146234449888));
#25377=CARTESIAN_POINT('Ctrl Pts',(95.35782732335,-0.414385943885653,-3.14485033243837));
#25378=CARTESIAN_POINT('Ctrl Pts',(95.4031340343663,-0.528548008740717,
-3.13706266846482));
#25379=CARTESIAN_POINT('Ctrl Pts',(95.4524587841208,-0.617445476633413,
-3.13098955491386));
#25380=CARTESIAN_POINT('Ctrl Pts',(95.5323877839963,-0.725848230390683,
-3.12242435708074));
#25381=CARTESIAN_POINT('Ctrl Pts',(95.5533614775886,-0.751895285761422,
-3.12026664759121));
#25382=CARTESIAN_POINT('Ctrl Pts',(95.5819192766561,-0.784424440552622,
-3.11741579950001));
#25383=CARTESIAN_POINT('Ctrl Pts',(95.5885181454773,-0.791753228365624,
-3.11676267125256));
#25384=CARTESIAN_POINT('Ctrl Pts',(95.5992868105714,-0.8034151251432,-3.11570522774752));
#25385=CARTESIAN_POINT('Ctrl Pts',(95.6033992090357,-0.807800777501227,
-3.11530331828718));
#25386=CARTESIAN_POINT('Ctrl Pts',(95.6113131425393,-0.816112099201845,
-3.11453338254936));
#25387=CARTESIAN_POINT('Ctrl Pts',(95.6151087838215,-0.820043183383064,
-3.11416561340655));
#25388=CARTESIAN_POINT('Ctrl Pts',(95.6238808132659,-0.829002606611762,
-3.11331900067909));
#25389=CARTESIAN_POINT('Ctrl Pts',(95.6288753855253,-0.834012764833267,
-3.11283937609178));
#25390=CARTESIAN_POINT('Ctrl Pts',(95.6446331362918,-0.849537405856089,
-3.11133342310889));
#25391=CARTESIAN_POINT('Ctrl Pts',(95.6555524990969,-0.859890464944481,
-3.11030024511203));
#25392=CARTESIAN_POINT('Ctrl Pts',(95.6814839561895,-0.883550260810635,
-3.10786929906239));
#25393=CARTESIAN_POINT('Ctrl Pts',(95.6966432719301,-0.896687960923984,
-3.10646510787272));
#25394=CARTESIAN_POINT('Ctrl Pts',(95.7533991485074,-0.943391113113564,
-3.10126779144723));
#25395=CARTESIAN_POINT('Ctrl Pts',(95.796927756772,-0.974498589916816,-3.09739165977353));
#25396=CARTESIAN_POINT('Ctrl Pts',(95.9099798663846,-1.0441953823916,-3.08766513798926));
#25397=CARTESIAN_POINT('Ctrl Pts',(95.9815890125677,-1.07891606625807,-3.081786070867));
#25398=CARTESIAN_POINT('Ctrl Pts',(96.0651215072671,-1.10944904872095,-3.07555914180613));
#25399=CARTESIAN_POINT('Ctrl Pts',(96.0741317578964,-1.11261880127896,-3.07489552143454));
#25400=CARTESIAN_POINT('Ctrl Pts',(96.0867289098586,-1.11687891514314,-3.07397982125982));
#25401=CARTESIAN_POINT('Ctrl Pts',(96.0902836645051,-1.11806219387595,-3.0737227543308));
#25402=CARTESIAN_POINT('Ctrl Pts',(96.0967809912372,-1.12019058821716,-3.07325539434339));
#25403=CARTESIAN_POINT('Ctrl Pts',(96.0997217515134,-1.12114112203396,-3.07304479484892));
#25404=CARTESIAN_POINT('Ctrl Pts',(96.1058237138427,-1.12308694707486,-3.07260978308047));
#25405=CARTESIAN_POINT('Ctrl Pts',(96.1089854177312,-1.12408048525348,-3.07238547116343));
#25406=CARTESIAN_POINT('Ctrl Pts',(96.1172680474249,-1.12664486721356,-3.07180058536465));
#25407=CARTESIAN_POINT('Ctrl Pts',(96.1223956412252,-1.12819416769388,-3.07144122553461));
#25408=CARTESIAN_POINT('Ctrl Pts',(96.1454333886894,-1.1349838428861,-3.06983812783228));
#25409=CARTESIAN_POINT('Ctrl Pts',(96.1634571135928,-1.13983341984474,-3.06861490562632));
#25410=CARTESIAN_POINT('Ctrl Pts',(96.2151287939989,-1.15242747203118,-3.06517580293584));
#25411=CARTESIAN_POINT('Ctrl Pts',(96.249013689404,-1.15912411313574,-3.06300109130569));
#25412=CARTESIAN_POINT('Ctrl Pts',(96.3603773976328,-1.17608561559311,-3.05597617286261));
#25413=CARTESIAN_POINT('Ctrl Pts',(96.4385848592033,-1.18013496855584,-3.05122035080892));
#25414=CARTESIAN_POINT('Ctrl Pts',(96.5531933428802,-1.17466605076945,-3.04394795409462));
#25415=CARTESIAN_POINT('Ctrl Pts',(96.5896648949994,-1.17121604195322,-3.04159078765786));
#25416=CARTESIAN_POINT('Ctrl Pts',(96.6359807761467,-1.164645118841,-3.03851192044276));
#25417=CARTESIAN_POINT('Ctrl Pts',(96.6460283553419,-1.16308666554623,-3.03783887884745));
#25418=CARTESIAN_POINT('Ctrl Pts',(96.662048706251,-1.16038892380336,-3.0367569719613));
#25419=CARTESIAN_POINT('Ctrl Pts',(96.6680351646755,-1.15933311022793,-3.0363507203432));
#25420=CARTESIAN_POINT('Ctrl Pts',(96.6793723745648,-1.15724297567353,-3.03557749999468));
#25421=CARTESIAN_POINT('Ctrl Pts',(96.6847246602296,-1.15621776374552,-3.03521082649259));
#25422=CARTESIAN_POINT('Ctrl Pts',(96.696886602852,-1.15380056222418,-3.03437381595719));
#25423=CARTESIAN_POINT('Ctrl Pts',(96.703691386933,-1.15238537385207,-3.03390275960276));
#25424=CARTESIAN_POINT('Ctrl Pts',(96.7245445675324,-1.14785561899205,-3.03245057728314));
#25425=CARTESIAN_POINT('Ctrl Pts',(96.7385482870937,-1.14454385692141,-3.03146328342912));
#25426=CARTESIAN_POINT('Ctrl Pts',(96.8065414721501,-1.12714258546035,-3.02660830388785));
#25427=CARTESIAN_POINT('Ctrl Pts',(96.8595364085919,-1.10948701084169,-3.02262946222148));
#25428=CARTESIAN_POINT('Ctrl Pts',(96.9930489986196,-1.0542003806011,-3.01213027339254));
#25429=CARTESIAN_POINT('Ctrl Pts',(97.0709237652827,-1.01110184527003,-3.00551388142081));
#25430=CARTESIAN_POINT('Ctrl Pts',(97.1565820562292,-0.950161672381643,
-2.99805279667147));
#25431=CARTESIAN_POINT('Ctrl Pts',(97.1697444621521,-0.940377206693605,
-2.99690149697072));
#25432=CARTESIAN_POINT('Ctrl Pts',(97.1868891613878,-0.927067586969161,
-2.99539983345348));
#25433=CARTESIAN_POINT('Ctrl Pts',(97.1910573905014,-0.92378637554014,-2.99503458623596));
#25434=CARTESIAN_POINT('Ctrl Pts',(97.1977845902097,-0.918416741647205,
-2.99444503254865));
#25435=CARTESIAN_POINT('Ctrl Pts',(97.2003571375762,-0.916345566335308,
-2.99421956394865));
#25436=CARTESIAN_POINT('Ctrl Pts',(97.2053044524956,-0.912328032690507,
-2.99378598269923));
#25437=CARTESIAN_POINT('Ctrl Pts',(97.2076803594539,-0.910383178598652,
-2.99357777379183));
#25438=CARTESIAN_POINT('Ctrl Pts',(97.2132532037757,-0.905784884220247,
-2.99308937271893));
#25439=CARTESIAN_POINT('Ctrl Pts',(97.2164437983878,-0.903123743288702,
-2.99280972325654));
#25440=CARTESIAN_POINT('Ctrl Pts',(97.2233627712162,-0.897290560427546,
-2.99220305896326));
#25441=CARTESIAN_POINT('Ctrl Pts',(97.2270856090653,-0.894112029701201,
-2.99187648880318));
#25442=CARTESIAN_POINT('Ctrl Pts',(97.2373799774598,-0.88521121153983,-2.99097269429881));
#25443=CARTESIAN_POINT('Ctrl Pts',(97.2439081256502,-0.879438945231865,
-2.9903986787372));
#25444=CARTESIAN_POINT('Ctrl Pts',(97.2651984889004,-0.860188523820308,
-2.98852136051856));
#25445=CARTESIAN_POINT('Ctrl Pts',(97.2796823452108,-0.846406392633618,
-2.98723569488297));
#25446=CARTESIAN_POINT('Ctrl Pts',(97.3518218119252,-0.774174462494765,
-2.98074433415138));
#25447=CARTESIAN_POINT('Ctrl Pts',(97.4036049931769,-0.710178400745265,
-2.97577255524557));
#25448=CARTESIAN_POINT('Ctrl Pts',(97.4769901014258,-0.597141286668738,
-2.96734429994462));
#25449=CARTESIAN_POINT('Ctrl Pts',(97.5026686331844,-0.551101044715363,
-2.96399692254765));
#25450=CARTESIAN_POINT('Ctrl Pts',(97.5298914951449,-0.493535876865327,
-2.95981454271306));
#25451=CARTESIAN_POINT('Ctrl Pts',(97.5344638238239,-0.483505273100771,
-2.95908603617534));
#25452=CARTESIAN_POINT('Ctrl Pts',(97.5414387792638,-0.467616611415199,
-2.95793174257182));
#25453=CARTESIAN_POINT('Ctrl Pts',(97.5439361936714,-0.461800667217046,
-2.95750915460304));
#25454=CARTESIAN_POINT('Ctrl Pts',(97.548465233225,-0.451014510774662,-2.95672516987478));
#25455=CARTESIAN_POINT('Ctrl Pts',(97.5505099929958,-0.44604996722813,-2.95636422460229));
#25456=CARTESIAN_POINT('Ctrl Pts',(97.5549800576062,-0.434982631839735,
-2.95555926652657));
#25457=CARTESIAN_POINT('Ctrl Pts',(97.5573883940214,-0.428873224604644,
-2.95511470289317));
#25458=CARTESIAN_POINT('Ctrl Pts',(97.5642177120164,-0.411114900009522,
-2.95382169775168));
#25459=CARTESIAN_POINT('Ctrl Pts',(97.568504977346,-0.399415867230539,-2.9529688965145));
#25460=CARTESIAN_POINT('Ctrl Pts',(97.5777891446315,-0.372780719729976,
-2.95102443631894));
#25461=CARTESIAN_POINT('Ctrl Pts',(97.5826735839436,-0.357808214621021,
-2.94992934910239));
#25462=CARTESIAN_POINT('Ctrl Pts',(97.5978663382881,-0.307861679145551,
-2.94626871955088));
#25463=CARTESIAN_POINT('Ctrl Pts',(97.6068501517927,-0.272509735916407,
-2.94366483576044));
#25464=CARTESIAN_POINT('Ctrl Pts',(97.6302157724857,-0.15867197365401,-2.93525594847338));
#25465=CARTESIAN_POINT('Ctrl Pts',(97.6382729731053,-0.07912373339909,-2.92932917990252));
#25466=CARTESIAN_POINT('Ctrl Pts',(97.6382307847678,0.000623063363894689,
-2.92357187405869));
#25467=CARTESIAN_POINT('Ctrl Pts',(97.6382307838965,0.000624708245411292,
-2.92357175530679));
#25468=CARTESIAN_POINT('Ctrl Pts',(97.6382200576542,0.0208466762333824,
-2.92211183462094));
#25469=CARTESIAN_POINT('Ctrl Pts',(97.6376885142611,0.0410664476087709,
-2.92066502402141));
#25470=CARTESIAN_POINT('Ctrl Pts',(97.6360622140238,0.0722884927679515,
-2.91846009423071));
#25471=CARTESIAN_POINT('Ctrl Pts',(97.6353329528843,0.083305023328173,-2.91768773127109));
#25472=CARTESIAN_POINT('Ctrl Pts',(97.6341135960156,0.0984835176264949,
-2.91663277603021));
#25473=CARTESIAN_POINT('Ctrl Pts',(97.6337560713312,0.102655160580913,-2.91634379392765));
#25474=CARTESIAN_POINT('Ctrl Pts',(97.6330962775147,0.109899438030602,-2.9158437317152));
#25475=CARTESIAN_POINT('Ctrl Pts',(97.6328041614323,0.112972922786058,-2.91563212772087));
#25476=CARTESIAN_POINT('Ctrl Pts',(97.6322144695702,0.118928616547422,-2.91522320904985));
#25477=CARTESIAN_POINT('Ctrl Pts',(97.6319183355781,0.121810956513514,-2.91502581734544));
#25478=CARTESIAN_POINT('Ctrl Pts',(97.6312597418791,0.127996579577273,-2.91460333773178));
#25479=CARTESIAN_POINT('Ctrl Pts',(97.6308939354182,0.131299459838404,-2.91437843690302));
#25480=CARTESIAN_POINT('Ctrl Pts',(97.6298973709302,0.139962213275983,-2.91379026823759));
#25481=CARTESIAN_POINT('Ctrl Pts',(97.6292437343871,0.145319452578551,-2.91342823956589));
#25482=CARTESIAN_POINT('Ctrl Pts',(97.6263575133559,0.167694624255707,-2.91192261479255));
#25483=CARTESIAN_POINT('Ctrl Pts',(97.6237897611973,0.184668168497702,-2.91079603636991));
#25484=CARTESIAN_POINT('Ctrl Pts',(97.616442722953,0.226960383239004,-2.90801441228442));
#25485=CARTESIAN_POINT('Ctrl Pts',(97.6112019519173,0.252190361787846,-2.90637791061506));
#25486=CARTESIAN_POINT('Ctrl Pts',(97.5838509200275,0.365120356223873,-2.89907646267668));
#25487=CARTESIAN_POINT('Ctrl Pts',(97.552513132994,0.450265876192737,-2.89361209556491));
#25488=CARTESIAN_POINT('Ctrl Pts',(97.4957586195887,0.562629324071688,-2.88561860773344));
#25489=CARTESIAN_POINT('Ctrl Pts',(97.4783580454184,0.593529653678918,-2.88333272300151));
#25490=CARTESIAN_POINT('Ctrl Pts',(97.4544641065259,0.63181194817932,-2.88035945550087));
#25491=CARTESIAN_POINT('Ctrl Pts',(97.4492352792564,0.639963843119852,-2.87971786345913));
#25492=CARTESIAN_POINT('Ctrl Pts',(97.4406197495736,0.653038037246644,-2.8786745859055));
#25493=CARTESIAN_POINT('Ctrl Pts',(97.4372950110972,0.658000784454563,-2.87827518896341));
#25494=CARTESIAN_POINT('Ctrl Pts',(97.4308509248713,0.667463219249453,-2.87750702246368));
#25495=CARTESIAN_POINT('Ctrl Pts',(97.4277376632707,0.671966878708811,-2.87713848731499));
#25496=CARTESIAN_POINT('Ctrl Pts',(97.4205532148742,0.682206554536134,-2.87629376446147));
#25497=CARTESIAN_POINT('Ctrl Pts',(97.4164618486732,0.687928088170462,-2.87581682266126));
#25498=CARTESIAN_POINT('Ctrl Pts',(97.4036685150321,0.705484271766663,-2.8743377671868));
#25499=CARTESIAN_POINT('Ctrl Pts',(97.3947964865978,0.717192641375545,-2.8733291948492));
#25500=CARTESIAN_POINT('Ctrl Pts',(97.3292443300348,0.800420320291184,-2.86599454841086));
#25501=CARTESIAN_POINT('Ctrl Pts',(97.2646501074495,0.865290863763662,-2.85934395187622));
#25502=CARTESIAN_POINT('Ctrl Pts',(97.1776881841854,0.93439989836288,-2.85119204829202));
#25503=CARTESIAN_POINT('Ctrl Pts',(97.1618317391493,0.946359591977941,-2.84973551157088));
#25504=CARTESIAN_POINT('Ctrl Pts',(97.1371256381188,0.964031978173706,-2.84751731717873));
#25505=CARTESIAN_POINT('Ctrl Pts',(97.1284892358031,0.970036404582205,-2.8467511548269));
#25506=CARTESIAN_POINT('Ctrl Pts',(97.0994809187217,0.989633173165769,-2.84421059883275));
#25507=CARTESIAN_POINT('Ctrl Pts',(97.0787644262287,1.00270657414317,-2.8424491806011));
#25508=CARTESIAN_POINT('Ctrl Pts',(97.049034194821,1.02019613648238,-2.84000879795541));
#25509=CARTESIAN_POINT('Ctrl Pts',(97.0403497088137,1.02515721546501,-2.8393061133871));
#25510=CARTESIAN_POINT('Ctrl Pts',(97.0250094818353,1.03366311509145,-2.83808393997327));
#25511=CARTESIAN_POINT('Ctrl Pts',(97.0183810320589,1.03725570837788,-2.83756197053904));
#25512=CARTESIAN_POINT('Ctrl Pts',(97.0084126612964,1.04253532052752,-2.8367866141955));
#25513=CARTESIAN_POINT('Ctrl Pts',(97.0050986125118,1.04427039479552,-2.83653041698755));
#25514=CARTESIAN_POINT('Ctrl Pts',(97.0017635779524,1.04599626142931,-2.83627421643074));
#25515=CARTESIAN_POINT('Ctrl Pts',(97.0017508597257,1.04600284276509,-2.83627323942793));
#25516=CARTESIAN_POINT('Ctrl Pts',(97.001725305159,1.04601606596627,-2.83627127639633));
#25517=CARTESIAN_POINT('Ctrl Pts',(97.0017124688816,1.04602270779372,-2.83627029037278));
#25518=CARTESIAN_POINT('Ctrl Pts',(97.0016866770629,1.04603605255711,-2.83626830921265));
#25519=CARTESIAN_POINT('Ctrl Pts',(97.0016737211745,1.04604275566701,-2.83626731404985));
#25520=CARTESIAN_POINT('Ctrl Pts',(97.0016476881485,1.04605622400551,-2.83626531446008));
#25521=CARTESIAN_POINT('Ctrl Pts',(97.0016346116658,1.04606298888959,-2.83626431008386));
#25522=CARTESIAN_POINT('Ctrl Pts',(97.0016083361947,1.04607658140938,-2.83626229197212));
#25523=CARTESIAN_POINT('Ctrl Pts',(97.0015951370314,1.04608340912971,-2.83626127822362));
#25524=CARTESIAN_POINT('Ctrl Pts',(97.0015686146738,1.04609712809335,-2.8362592412516));
#25525=CARTESIAN_POINT('Ctrl Pts',(97.0015552917613,1.0461040191849,-2.8362582180502));
#25526=CARTESIAN_POINT('Ctrl Pts',(97.0015285204552,1.0461178656232,-2.83625616206242));
#25527=CARTESIAN_POINT('Ctrl Pts',(97.0015150720133,1.04612482098877,-2.83625512927283));
#25528=CARTESIAN_POINT('Ctrl Pts',(97.0014880481205,1.04613879674694,-2.83625305399283));
#25529=CARTESIAN_POINT('Ctrl Pts',(97.0014744727672,1.04614581708281,-2.83625201151041));
#25530=CARTESIAN_POINT('Ctrl Pts',(97.0014471937013,1.04615992346106,-2.83624991674257));
#25531=CARTESIAN_POINT('Ctrl Pts',(97.0014334896944,1.04616700964929,-2.83624886443505));
#25532=CARTESIAN_POINT('Ctrl Pts',(97.0014059515975,1.04618124860451,-2.83624674988619));
#25533=CARTESIAN_POINT('Ctrl Pts',(97.0013921176172,1.04618840130826,-2.83624568765379));
#25534=CARTESIAN_POINT('Ctrl Pts',(97.0013643179878,1.04620277409486,-2.83624355313497));
#25535=CARTESIAN_POINT('Ctrl Pts',(97.0013503522125,1.0462099942363,-2.8362424808394));
#25536=CARTESIAN_POINT('Ctrl Pts',(97.0013222872284,1.04622450279055,-2.83624032606036));
#25537=CARTESIAN_POINT('Ctrl Pts',(97.0013081882112,1.04623179109754,-2.83623924359214));
#25538=CARTESIAN_POINT('Ctrl Pts',(97.0012798552718,1.04624643672321,-2.83623706835648));
#25539=CARTESIAN_POINT('Ctrl Pts',(97.0012656211068,1.04625379416046,-2.83623597557095));
#25540=CARTESIAN_POINT('Ctrl Pts',(97.001237016241,1.04626857886861,-2.83623377957715));
#25541=CARTESIAN_POINT('Ctrl Pts',(97.0012226454426,1.04627600618291,-2.83623267636196));
#25542=CARTESIAN_POINT('Ctrl Pts',(97.0011937652452,1.04629093169102,-2.83623045935203));
#25543=CARTESIAN_POINT('Ctrl Pts',(97.0011792562182,1.04629842968538,-2.83622934558644));
#25544=CARTESIAN_POINT('Ctrl Pts',(97.0011500977151,1.04631349748702,-2.83622710733557));
#25545=CARTESIAN_POINT('Ctrl Pts',(97.0011354485582,1.046321067122,-2.83622598287539));
#25546=CARTESIAN_POINT('Ctrl Pts',(97.001106008481,1.04633627886172,-2.8362237231363));
#25547=CARTESIAN_POINT('Ctrl Pts',(97.0010912172478,1.04634392112063,-2.83622258783395));
#25548=CARTESIAN_POINT('Ctrl Pts',(97.0010614914671,1.04635927888675,-2.8362203062933));
#25549=CARTESIAN_POINT('Ctrl Pts',(97.0010465565831,1.04636699456006,-2.8362191600298));
#25550=CARTESIAN_POINT('Ctrl Pts',(97.0010165410557,1.04638250039499,-2.83621685638103));
#25551=CARTESIAN_POINT('Ctrl Pts',(97.0010014610511,1.04639029021867,-2.83621569904543));
#25552=CARTESIAN_POINT('Ctrl Pts',(97.0009711537988,1.04640594509682,-2.83621337314054));
#25553=CARTESIAN_POINT('Ctrl Pts',(97.0009559261828,1.04641381033351,-2.83621220454363));
#25554=CARTESIAN_POINT('Ctrl Pts',(97.0009253219372,1.04642961692784,-2.83620985598222));
#25555=CARTESIAN_POINT('Ctrl Pts',(97.0009099453165,1.0464375582726,-2.83620867601905));
#25556=CARTESIAN_POINT('Ctrl Pts',(97.0008790411323,1.04645351805459,-2.83620630457909));
#25557=CARTESIAN_POINT('Ctrl Pts',(97.0008635134599,1.04646153653954,-2.83620511309462));
#25558=CARTESIAN_POINT('Ctrl Pts',(97.0008323050362,1.04647765167958,-2.83620271845018));
#25559=CARTESIAN_POINT('Ctrl Pts',(97.0008166245765,1.04648574817543,-2.83620151531328));
#25560=CARTESIAN_POINT('Ctrl Pts',(97.0007851088386,1.04650202020935,-2.83619909723262));
#25561=CARTESIAN_POINT('Ctrl Pts',(97.0007692733564,1.04651019584392,-2.83619788227392));
#25562=CARTESIAN_POINT('Ctrl Pts',(97.0007374458956,1.04652662699495,-2.83619544042305));
#25563=CARTESIAN_POINT('Ctrl Pts',(97.0007214535335,1.0465348827004,-2.8361942135022));
#25564=CARTESIAN_POINT('Ctrl Pts',(97.0006893100342,1.04655147514231,-2.83619174755441));
#25565=CARTESIAN_POINT('Ctrl Pts',(97.0006731590339,1.04655981179885,-2.83619050853873));
#25566=CARTESIAN_POINT('Ctrl Pts',(97.00064069607,1.04657656724463,-2.83618801823566));
#25567=CARTESIAN_POINT('Ctrl Pts',(97.000624384237,1.04658498595701,-2.83618676695905));
#25568=CARTESIAN_POINT('Ctrl Pts',(97.00059159798,1.04660190632608,-2.83618425201158));
#25569=CARTESIAN_POINT('Ctrl Pts',(97.0005751230591,1.04661040822953,-2.83618298830338));
#25570=CARTESIAN_POINT('Ctrl Pts',(97.0005420083843,1.04662749610861,-2.8361804483231));
#25571=CARTESIAN_POINT('Ctrl Pts',(97.0005253686955,1.04663608204071,-2.83617917205681));
#25572=CARTESIAN_POINT('Ctrl Pts',(97.0004919221036,1.04665333917613,-2.8361766067801));
#25573=CARTESIAN_POINT('Ctrl Pts',(97.0004751153979,1.04666201026745,-2.83617531778564));
#25574=CARTESIAN_POINT('Ctrl Pts',(97.0004413326219,1.04667943880009,-2.83617272689014));
#25575=CARTESIAN_POINT('Ctrl Pts',(97.0004243567054,1.04668819615178,-2.83617142500173));
#25576=CARTESIAN_POINT('Ctrl Pts',(97.0003927143127,1.04670451851149,-2.83616899841504));
#25577=CARTESIAN_POINT('Ctrl Pts',(97.0003780476421,1.04671208375238,-2.83616787369118));
#25578=CARTESIAN_POINT('Ctrl Pts',(97.0003480451391,1.04672755859734,-2.83616557299255));
#25579=CARTESIAN_POINT('Ctrl Pts',(97.0003327096747,1.04673546797514,-2.83616439704895));
#25580=CARTESIAN_POINT('Ctrl Pts',(97.0003013385469,1.04675164699076,-2.83616199153978));
#25581=CARTESIAN_POINT('Ctrl Pts',(97.0002853025206,1.04675991677591,-2.8361607619496));
#25582=CARTESIAN_POINT('Ctrl Pts',(97.0002524970752,1.04677683360273,-2.8361582466119));
#25583=CARTESIAN_POINT('Ctrl Pts',(97.0002357281957,1.04678548032261,-2.83615696090925));
#25584=CARTESIAN_POINT('Ctrl Pts',(97.0002014228425,1.04680316852185,-2.83615433073501));
#25585=CARTESIAN_POINT('Ctrl Pts',(97.000183886109,1.0468122100874,-2.83615298624734));
#25586=CARTESIAN_POINT('Ctrl Pts',(97.0001480088512,1.04683070649464,-2.8361502357397));
#25587=CARTESIAN_POINT('Ctrl Pts',(97.0001296685942,1.04684016114631,-2.83614882974443));
#25588=CARTESIAN_POINT('Ctrl Pts',(97.0000921464834,1.04685950305613,-2.83614595333614));
#25589=CARTESIAN_POINT('Ctrl Pts',(97.0000729645317,1.04686939030753,-2.83614448292022));
#25590=CARTESIAN_POINT('Ctrl Pts',(97.0000337193397,1.04688961770136,-2.83614147464208));
#25591=CARTESIAN_POINT('Ctrl Pts',(97.000013656137,1.04689995776169,-2.83613993678779));
#25592=CARTESIAN_POINT('Ctrl Pts',(96.9999726070225,1.04692111192968,-2.83613679047338));
#25593=CARTESIAN_POINT('Ctrl Pts',(96.9999516207137,1.04693192617316,-2.83613518198837));
#25594=CARTESIAN_POINT('Ctrl Pts',(96.9999086816822,1.04695405101928,-2.83613189107966));
#25595=CARTESIAN_POINT('Ctrl Pts',(96.9998867287839,1.04696536163717,-2.83613020864857));
#25596=CARTESIAN_POINT('Ctrl Pts',(96.9998418103219,1.04698850283274,-2.83612676632155));
#25597=CARTESIAN_POINT('Ctrl Pts',(96.9998188450897,1.04700033315721,-2.83612500645767));
#25598=CARTESIAN_POINT('Ctrl Pts',(96.9997718541473,1.04702453814519,-2.83612140562136));
#25599=CARTESIAN_POINT('Ctrl Pts',(96.9997478281137,1.04703691288499,-2.83611956463143));
#25600=CARTESIAN_POINT('Ctrl Pts',(96.9996986651567,1.04706223239331,-2.83611579770245));
#25601=CARTESIAN_POINT('Ctrl Pts',(96.9996735282113,1.0470751770743,-2.83611387176967));
#25602=CARTESIAN_POINT('Ctrl Pts',(96.9996220903764,1.04710166348479,-2.83610993091443));
#25603=CARTESIAN_POINT('Ctrl Pts',(96.9995957895622,1.04711520506718,-2.83610791600646));
#25604=CARTESIAN_POINT('Ctrl Pts',(96.9995419683922,1.04714291357581,-2.83610379296818));
#25605=CARTESIAN_POINT('Ctrl Pts',(96.9995144482628,1.04715708026666,-2.83610168486479));
#25606=CARTESIAN_POINT('Ctrl Pts',(96.9994581305478,1.04718606844328,-2.8360973710285));
#25607=CARTESIAN_POINT('Ctrl Pts',(96.9994293327486,1.04720088990876,-2.83609516528974));
#25608=CARTESIAN_POINT('Ctrl Pts',(96.9993703988724,1.04723121854093,-2.83609065155623));
#25609=CARTESIAN_POINT('Ctrl Pts',(96.9993402625758,1.04724672567792,-2.83608834355616));
#25610=CARTESIAN_POINT('Ctrl Pts',(96.9992785876637,1.04727845817155,-2.83608362043057));
#25611=CARTESIAN_POINT('Ctrl Pts',(96.9992470490281,1.04729468338197,-2.83608120531614));
#25612=CARTESIAN_POINT('Ctrl Pts',(96.9991825024183,1.04732788602431,-2.83607626286822));
#25613=CARTESIAN_POINT('Ctrl Pts',(96.9991494943946,1.04734486331,-2.8360737355448));
#25614=CARTESIAN_POINT('Ctrl Pts',(96.9990837284374,1.04737868531904,-2.83606870036398));
#25615=CARTESIAN_POINT('Ctrl Pts',(96.9990509705815,1.04739553003247,-2.83606619251011));
#25616=CARTESIAN_POINT('Ctrl Pts',(96.9989780966347,1.04743299888128,-2.83606061382459));
#25617=CARTESIAN_POINT('Ctrl Pts',(96.9989379800671,1.04745362229097,-2.83605754303485));
#25618=CARTESIAN_POINT('Ctrl Pts',(96.998848745859,1.04749948996466,-2.8360507129767));
#25619=CARTESIAN_POINT('Ctrl Pts',(96.9987996275969,1.04752473309453,-2.83604695377813));
#25620=CARTESIAN_POINT('Ctrl Pts',(96.9986903874506,1.04758086468419,-2.83603859401873));
#25621=CARTESIAN_POINT('Ctrl Pts',(96.9986302647637,1.04761175138158,-2.83603399357222));
#25622=CARTESIAN_POINT('Ctrl Pts',(96.9984497307201,1.04770447710142,-2.83602018112));
#25623=CARTESIAN_POINT('Ctrl Pts',(96.9983293112801,1.04776630058248,-2.83601097008789));
#25624=CARTESIAN_POINT('Ctrl Pts',(96.9954582575898,1.04923967752026,-2.83579141023946));
#25625=CARTESIAN_POINT('Ctrl Pts',(96.9927020756964,1.05064042095293,-2.8355817477836));
#25626=CARTESIAN_POINT('Ctrl Pts',(96.9865897183398,1.05371661110011,-2.83511917414598));
#25627=CARTESIAN_POINT('Ctrl Pts',(96.9832309584351,1.05538692538626,-2.83486657542912));
#25628=CARTESIAN_POINT('Ctrl Pts',(96.9712658332756,1.06126605844432,-2.83397215020811));
#25629=CARTESIAN_POINT('Ctrl Pts',(96.9626158788199,1.06538601994717,-2.83333547250403));
#25630=CARTESIAN_POINT('Ctrl Pts',(96.8831011816924,1.10207515009635,-2.82756433798437));
#25631=CARTESIAN_POINT('Ctrl Pts',(96.8092048344613,1.12764033084855,-2.82278019432459));
#25632=CARTESIAN_POINT('Ctrl Pts',(96.6804084361057,1.15831114223334,-2.81458872521298));
#25633=CARTESIAN_POINT('Ctrl Pts',(96.6266964660867,1.16722944498864,-2.81121475584011));
#25634=CARTESIAN_POINT('Ctrl Pts',(96.5523893872103,1.1743332720838,-2.80644895866472));
#25635=CARTESIAN_POINT('Ctrl Pts',(96.532169359578,1.17574082844781,-2.80514273902991));
#25636=CARTESIAN_POINT('Ctrl Pts',(96.4967712652627,1.17728845969005,-2.80283254760023));
#25637=CARTESIAN_POINT('Ctrl Pts',(96.4816078220439,1.17765815305746,-2.80183544577691));
#25638=CARTESIAN_POINT('Ctrl Pts',(96.4593452629466,1.17777083418023,-2.80035860838719));
#25639=CARTESIAN_POINT('Ctrl Pts',(96.4522484681269,1.17774260778417,-2.79988590429107));
#25640=CARTESIAN_POINT('Ctrl Pts',(96.4396855788131,1.177579087464,-2.79904551672093));
#25641=CARTESIAN_POINT('Ctrl Pts',(96.4342193099253,1.17746986341124,-2.79867864784263));
#25642=CARTESIAN_POINT('Ctrl Pts',(96.4227553374457,1.1771609285487,-2.79790662175393));
#25643=CARTESIAN_POINT('Ctrl Pts',(96.4167580185672,1.17695343005497,-2.79750123441681));
#25644=CARTESIAN_POINT('Ctrl Pts',(96.4009611125814,1.17628597415192,-2.79642934713953));
#25645=CARTESIAN_POINT('Ctrl Pts',(96.3911654068634,1.1757493990743,-2.79576050420177));
#25646=CARTESIAN_POINT('Ctrl Pts',(96.3484684016645,1.17287517996881,-2.79282628438202));
#25647=CARTESIAN_POINT('Ctrl Pts',(96.3156696802063,1.16927854971727,-2.79052267527381));
#25648=CARTESIAN_POINT('Ctrl Pts',(96.1824756344831,1.1489829470998,-2.78095891734609));
#25649=CARTESIAN_POINT('Ctrl Pts',(96.0842986985664,1.12068314393935,-2.77337181593966));
#25650=CARTESIAN_POINT('Ctrl Pts',(95.9711832733422,1.07151753323898,-2.7644518492937));
#25651=CARTESIAN_POINT('Ctrl Pts',(95.9516043251507,1.06235904226172,-2.76290315540541));
#25652=CARTESIAN_POINT('Ctrl Pts',(95.9287833015,1.0509081993579,-2.76110075900233));
#25653=CARTESIAN_POINT('Ctrl Pts',(95.9252880219267,1.04913248098871,-2.76082478278657));
#25654=CARTESIAN_POINT('Ctrl Pts',(95.9218016730066,1.04733934304671,-2.76054963702842));
#25655=CARTESIAN_POINT('Ctrl Pts',(95.9218019448244,1.04733948285108,-2.66237442964626));
#25656=CARTESIAN_POINT('Ctrl Pts',(95.9663540586353,1.07025400934438,-2.66601386898332));
#25657=CARTESIAN_POINT('Ctrl Pts',(96.0123492927123,1.09031600146745,-2.66970698864775));
#25658=CARTESIAN_POINT('Ctrl Pts',(96.1086000098264,1.12516685586158,-2.67720048344083));
#25659=CARTESIAN_POINT('Ctrl Pts',(96.1588220835574,1.13965954581114,-2.68098827651821));
#25660=CARTESIAN_POINT('Ctrl Pts',(96.2166448882217,1.15225321068321,-2.68510428922803));
#25661=CARTESIAN_POINT('Ctrl Pts',(96.223457413953,1.15367384288636,-2.68558540435396));
#25662=CARTESIAN_POINT('Ctrl Pts',(96.2338733587941,1.1557497436619,-2.68631477400422));
#25663=CARTESIAN_POINT('Ctrl Pts',(96.2374677634198,1.15644869747496,-2.68656534224159));
#25664=CARTESIAN_POINT('Ctrl Pts',(96.2440542443618,1.15769762804151,-2.68702235583915));
#25665=CARTESIAN_POINT('Ctrl Pts',(96.2470452029915,1.15825277864105,-2.6872290772222));
#25666=CARTESIAN_POINT('Ctrl Pts',(96.253802636675,1.15947995857396,-2.68769430912778));
#25667=CARTESIAN_POINT('Ctrl Pts',(96.257570257238,1.16014522854953,-2.68795244151098));
#25668=CARTESIAN_POINT('Ctrl Pts',(96.2673169651254,1.16181732615593,-2.68861712787747));
#25669=CARTESIAN_POINT('Ctrl Pts',(96.2733007940795,1.16279637832727,-2.6890221979335));
#25670=CARTESIAN_POINT('Ctrl Pts',(96.3135293102752,1.16905982837264,-2.69172691573369));
#25671=CARTESIAN_POINT('Ctrl Pts',(96.3479888329969,1.17287752801496,-2.69395399200171));
#25672=CARTESIAN_POINT('Ctrl Pts',(96.4107084007409,1.17703568710873,-2.69792577585794));
#25673=CARTESIAN_POINT('Ctrl Pts',(96.438905886038,1.17789004272111,-2.69968171942755));
#25674=CARTESIAN_POINT('Ctrl Pts',(96.515053759483,1.17746157386284,-2.70440312758135));
#25675=CARTESIAN_POINT('Ctrl Pts',(96.5629376360678,1.1742642312032,-2.70735163659253));
#25676=CARTESIAN_POINT('Ctrl Pts',(96.6634207426539,1.16136043503585,-2.71368682288293));
#25677=CARTESIAN_POINT('Ctrl Pts',(96.7158191573994,1.15097520984258,-2.71707895268986));
#25678=CARTESIAN_POINT('Ctrl Pts',(96.7777881101862,1.13425243655716,-2.72129748198627));
#25679=CARTESIAN_POINT('Ctrl Pts',(96.7882075808831,1.13128584644294,-2.72201383644248));
#25680=CARTESIAN_POINT('Ctrl Pts',(96.8045454837078,1.12638953532181,-2.72314892785088));
#25681=CARTESIAN_POINT('Ctrl Pts',(96.8104922467831,1.12455585821711,-2.72356457428885));
#25682=CARTESIAN_POINT('Ctrl Pts',(96.8215985279412,1.12103462174659,-2.72434564677691));
#25683=CARTESIAN_POINT('Ctrl Pts',(96.8267614726324,1.11935834534743,-2.72471069873768));
#25684=CARTESIAN_POINT('Ctrl Pts',(96.8382943024762,1.11552559693821,-2.72553062316257));
#25685=CARTESIAN_POINT('Ctrl Pts',(96.8446576338129,1.11335015116531,-2.72598610340758));
#25686=CARTESIAN_POINT('Ctrl Pts',(96.8608022575925,1.10767586638347,-2.72714974533548));
#25687=CARTESIAN_POINT('Ctrl Pts',(96.8705563584975,1.10410195255554,-2.72786033717157));
#25688=CARTESIAN_POINT('Ctrl Pts',(96.9507797487173,1.07349831447265,-2.73376886507221));
#25689=CARTESIAN_POINT('Ctrl Pts',(97.0185355208864,1.03988593423637,-2.73918851583574));
#25690=CARTESIAN_POINT('Ctrl Pts',(97.1317055887668,0.969482927792906,-2.7489383901991));
#25691=CARTESIAN_POINT('Ctrl Pts',(97.1784951794666,0.935358477456175,-2.75320978194467));
#25692=CARTESIAN_POINT('Ctrl Pts',(97.2382010136099,0.884684046383803,-2.75886465845143));
#25693=CARTESIAN_POINT('Ctrl Pts',(97.2534655393762,0.87102807056017,-2.76032991818037));
#25694=CARTESIAN_POINT('Ctrl Pts',(97.2778572319971,0.848033713443923,-2.76269399060493));
#25695=CARTESIAN_POINT('Ctrl Pts',(97.2871986512601,0.838929701006134,-2.76360511507559));
#25696=CARTESIAN_POINT('Ctrl Pts',(97.2996988533462,0.826335567239342,-2.76482995312867));
#25697=CARTESIAN_POINT('Ctrl Pts',(97.3029903976098,0.822979338471609,-2.76515302114701));
#25698=CARTESIAN_POINT('Ctrl Pts',(97.3084690829008,0.817325668490033,-2.76569153884634));
#25699=CARTESIAN_POINT('Ctrl Pts',(97.3106671692767,0.815038965475175,-2.7659078089783));
#25700=CARTESIAN_POINT('Ctrl Pts',(97.3148277645409,0.810675487541049,-2.76631752985166));
#25701=CARTESIAN_POINT('Ctrl Pts',(97.3167919900742,0.808600413495037,-2.76651111606723));
#25702=CARTESIAN_POINT('Ctrl Pts',(97.3214462009582,0.803647569217087,-2.76697024957072));
#25703=CARTESIAN_POINT('Ctrl Pts',(97.3241293599648,0.800763388232761,-2.7672352880574));
#25704=CARTESIAN_POINT('Ctrl Pts',(97.3335871098416,0.790494229011149,-2.76817098365678));
#25705=CARTESIAN_POINT('Ctrl Pts',(97.3402820881501,0.78303605670343,-2.76883605134641));
#25706=CARTESIAN_POINT('Ctrl Pts',(97.3865749324673,0.730122629399314,-2.77346160040564));
#25707=CARTESIAN_POINT('Ctrl Pts',(97.4227319137921,0.681765414417662,-2.77721774770458));
#25708=CARTESIAN_POINT('Ctrl Pts',(97.4907129690381,0.574591118580488,-2.78508024869095));
#25709=CARTESIAN_POINT('Ctrl Pts',(97.521556597827,0.515413263641715,-2.78917140781017));
#25710=CARTESIAN_POINT('Ctrl Pts',(97.5604357680378,0.42233640917668,-2.79558464550255));
#25711=CARTESIAN_POINT('Ctrl Pts',(97.5722532905243,0.390167351712429,-2.79779597112176));
#25712=CARTESIAN_POINT('Ctrl Pts',(97.5855595177424,0.348403572046824,-2.80068461261046));
#25713=CARTESIAN_POINT('Ctrl Pts',(97.5883561006421,0.339241017950264,-2.80131937103951));
#25714=CARTESIAN_POINT('Ctrl Pts',(97.5927080155404,0.324333686034414,-2.80235423823862));
#25715=CARTESIAN_POINT('Ctrl Pts',(97.5943321596776,0.31860932182205,-2.80275212662732));
#25716=CARTESIAN_POINT('Ctrl Pts',(97.5973689863232,0.307588524332501,-2.80351923880726));
#25717=CARTESIAN_POINT('Ctrl Pts',(97.5987882099123,0.302294041824895,-2.80388824183233));
#25718=CARTESIAN_POINT('Ctrl Pts',(97.6019559624507,0.290137891386286,-2.80473665691486));
#25719=CARTESIAN_POINT('Ctrl Pts',(97.6036796578444,0.283270031346951,-2.80521684625146));
#25720=CARTESIAN_POINT('Ctrl Pts',(97.6089788784832,0.261319419631843,-2.80675456967465));
#25721=CARTESIAN_POINT('Ctrl Pts',(97.6123184926412,0.246181978433166,-2.8078194878866));
#25722=CARTESIAN_POINT('Ctrl Pts',(97.630640734358,0.154574014095299,-2.81429402187953));
#25723=CARTESIAN_POINT('Ctrl Pts',(97.6382997778215,0.0768496093721461,
-2.81993130167333));
#25724=CARTESIAN_POINT('Ctrl Pts',(97.6381647893319,-0.0748980491663311,
-2.83105779166144));
#25725=CARTESIAN_POINT('Ctrl Pts',(97.631153159679,-0.148584594388026,-2.83651100063276));
#25726=CARTESIAN_POINT('Ctrl Pts',(97.6154736991933,-0.230607544573968,
-2.84236197868445));
#25727=CARTESIAN_POINT('Ctrl Pts',(97.6135463496234,-0.240058928974523,
-2.84303263086583));
#25728=CARTESIAN_POINT('Ctrl Pts',(97.6106820058404,-0.253273793745423,
-2.84396437021411));
#25729=CARTESIAN_POINT('Ctrl Pts',(97.6098422743851,-0.257057640475069,
-2.84423046884668));
#25730=CARTESIAN_POINT('Ctrl Pts',(97.6082920835984,-0.263883345113966,
-2.84470915722954));
#25731=CARTESIAN_POINT('Ctrl Pts',(97.6075881745252,-0.266926646243,-2.84492210611287));
#25732=CARTESIAN_POINT('Ctrl Pts',(97.6061251057949,-0.273139435339931,
-2.84535580638582));
#25733=CARTESIAN_POINT('Ctrl Pts',(97.6053648848538,-0.27630863036546,-2.8455764964868));
#25734=CARTESIAN_POINT('Ctrl Pts',(97.603379534233,-0.28443623828964,-2.84614116915173));
#25735=CARTESIAN_POINT('Ctrl Pts',(97.6021352724631,-0.289389975409617,
-2.84648408801441));
#25736=CARTESIAN_POINT('Ctrl Pts',(97.5967844263749,-0.310121368041253,
-2.84791457639331));
#25737=CARTESIAN_POINT('Ctrl Pts',(97.5923824693897,-0.325821836037436,
-2.84898666491449));
#25738=CARTESIAN_POINT('Ctrl Pts',(97.5794935326046,-0.368372932170697,
-2.8518740967461));
#25739=CARTESIAN_POINT('Ctrl Pts',(97.5703671887484,-0.395019662268076,
-2.85366244816334));
#25740=CARTESIAN_POINT('Ctrl Pts',(97.5299106068564,-0.500628611504686,
-2.86076312922837));
#25741=CARTESIAN_POINT('Ctrl Pts',(97.4910376196131,-0.576422005274534,
-2.8659071441088));
#25742=CARTESIAN_POINT('Ctrl Pts',(97.4230655427561,-0.679724476674423,
-2.87372873608515));
#25743=CARTESIAN_POINT('Ctrl Pts',(97.4002007336604,-0.710999799204278,
-2.87621708737866));
#25744=CARTESIAN_POINT('Ctrl Pts',(97.369332635706,-0.749126552268779,-2.8794445748785));
#25745=CARTESIAN_POINT('Ctrl Pts',(97.3627208775857,-0.757076667090176,
-2.88012884050519));
#25746=CARTESIAN_POINT('Ctrl Pts',(97.3520331234067,-0.769588974931314,
-2.88122451552935));
#25747=CARTESIAN_POINT('Ctrl Pts',(97.3480246786715,-0.774208367016738,
-2.88163319082155));
#25748=CARTESIAN_POINT('Ctrl Pts',(97.3407416566589,-0.782470536509436,
-2.88237181146634));
#25749=CARTESIAN_POINT('Ctrl Pts',(97.3374799675646,-0.786124528395592,
-2.88270122121272));
#25750=CARTESIAN_POINT('Ctrl Pts',(97.3297562787912,-0.794669297837173,
-2.88347811188416));
#25751=CARTESIAN_POINT('Ctrl Pts',(97.3252756838025,-0.79954296661796,-2.88392636270999));
#25752=CARTESIAN_POINT('Ctrl Pts',(97.3120658345516,-0.813670745079915,
-2.88524105728996));
#25753=CARTESIAN_POINT('Ctrl Pts',(97.3032276780343,-0.822821260908672,
-2.88611208946013));
#25754=CARTESIAN_POINT('Ctrl Pts',(97.2352688202048,-0.890938275222554,
-2.89274833266928));
#25755=CARTESIAN_POINT('Ctrl Pts',(97.1701865235266,-0.943599604013672,
-2.8987854688735));
#25756=CARTESIAN_POINT('Ctrl Pts',(97.039194677788,-1.02832218890769,-2.9102263522282));
#25757=CARTESIAN_POINT('Ctrl Pts',(96.9747764345198,-1.0620066336921,-2.91557835557593));
#25758=CARTESIAN_POINT('Ctrl Pts',(96.8986688311447,-1.0932433286244,-2.92134350565761));
#25759=CARTESIAN_POINT('Ctrl Pts',(96.889628416951,-1.09682362374725,-2.92201964738021));
#25760=CARTESIAN_POINT('Ctrl Pts',(96.876911070954,-1.10167878313548,-2.92295771333596));
#25761=CARTESIAN_POINT('Ctrl Pts',(96.8732708842239,-1.1030478947576,-2.92322473600786));
#25762=CARTESIAN_POINT('Ctrl Pts',(96.8669564293806,-1.10538718957934,-2.92368527581429));
#25763=CARTESIAN_POINT('Ctrl Pts',(96.8642853325616,-1.10636575113703,-2.92387927242119));
#25764=CARTESIAN_POINT('Ctrl Pts',(96.858614393183,-1.10842003744551,-2.9242893711362));
#25765=CARTESIAN_POINT('Ctrl Pts',(96.8556136754024,-1.10949328426272,-2.92450532228908));
#25766=CARTESIAN_POINT('Ctrl Pts',(96.8481078693628,-1.11214352293168,-2.925042961671));
#25767=CARTESIAN_POINT('Ctrl Pts',(96.8435974232867,-1.11370535334296,-2.9253637777945));
#25768=CARTESIAN_POINT('Ctrl Pts',(96.826222354679,-1.11960376326395,-2.92659138036781));
#25769=CARTESIAN_POINT('Ctrl Pts',(96.8132920225567,-1.12374541057853,-2.92748764698077));
#25770=CARTESIAN_POINT('Ctrl Pts',(96.7795599872562,-1.13391026548408,-2.92978816111361));
#25771=CARTESIAN_POINT('Ctrl Pts',(96.7586580314389,-1.13958521618735,-2.93117701218273));
#25772=CARTESIAN_POINT('Ctrl Pts',(96.6380778980831,-1.16877788413901,-2.93904225063871));
#25773=CARTESIAN_POINT('Ctrl Pts',(96.5358270161162,-1.17979130246164,-2.94518206607897));
#25774=CARTESIAN_POINT('Ctrl Pts',(96.4010626873588,-1.17669584278995,-2.95376466696525));
#25775=CARTESIAN_POINT('Ctrl Pts',(96.368736550134,-1.17461751554145,-2.95585668776548));
#25776=CARTESIAN_POINT('Ctrl Pts',(96.3268506949603,-1.17018500050912,-2.95863144908712));
#25777=CARTESIAN_POINT('Ctrl Pts',(96.3171755553971,-1.16903957803086,-2.95927681726107));
#25778=CARTESIAN_POINT('Ctrl Pts',(96.3015808585473,-1.16699685241761,-2.96032470843447));
#25779=CARTESIAN_POINT('Ctrl Pts',(96.2956518520169,-1.1661741974691,-2.96072490459219));
#25780=CARTESIAN_POINT('Ctrl Pts',(96.2843164256689,-1.16451322582957,-2.96149357907426));
#25781=CARTESIAN_POINT('Ctrl Pts',(96.2789090581526,-1.16368236178441,-2.96186181542352));
#25782=CARTESIAN_POINT('Ctrl Pts',(96.2664720770932,-1.16168257301862,-2.96271243653817));
#25783=CARTESIAN_POINT('Ctrl Pts',(96.2594469508878,-1.16048747109417,-2.96319562825402));
#25784=CARTESIAN_POINT('Ctrl Pts',(96.2373469939121,-1.15652117392608,-2.96472446950394));
#25785=CARTESIAN_POINT('Ctrl Pts',(96.2223156952353,-1.1535195105332,-2.96577727045876));
#25786=CARTESIAN_POINT('Ctrl Pts',(96.187282775681,-1.14580972518998,-2.9682625765319));
#25787=CARTESIAN_POINT('Ctrl Pts',(96.1673378046631,-1.14086992127229,-2.96970190607677));
#25788=CARTESIAN_POINT('Ctrl Pts',(96.0938667562285,-1.12061946410546,-2.97509554490433));
#25789=CARTESIAN_POINT('Ctrl Pts',(96.0413222022353,-1.10204294839336,-2.97913992276067));
#25790=CARTESIAN_POINT('Ctrl Pts',(95.9206239553812,-1.04948729889846,-2.98878857495109));
#25791=CARTESIAN_POINT('Ctrl Pts',(95.8540485676708,-1.01247757070838,-2.99440618208594));
#25792=CARTESIAN_POINT('Ctrl Pts',(95.7836770678246,-0.963909694778292,
-3.00039506305378));
#25793=CARTESIAN_POINT('Ctrl Pts',(95.7759201972558,-0.958416394212479,
-3.00105575947556));
#25794=CARTESIAN_POINT('Ctrl Pts',(95.7651143461908,-0.950565717938824,
-3.00197600774841));
#25795=CARTESIAN_POINT('Ctrl Pts',(95.7620093833136,-0.948286543926136,
-3.00224041512364));
#25796=CARTESIAN_POINT('Ctrl Pts',(95.7564118710914,-0.944135324862518,
-3.00271696503446));
#25797=CARTESIAN_POINT('Ctrl Pts',(95.7539154708188,-0.942268541325628,
-3.00292945688122));
#25798=CARTESIAN_POINT('Ctrl Pts',(95.7488167377208,-0.938424101695163,
-3.00336332418986));
#25799=CARTESIAN_POINT('Ctrl Pts',(95.7462151804926,-0.936445490594071,
-3.00358463140933));
#25800=CARTESIAN_POINT('Ctrl Pts',(95.739535550762,-0.931321275969118,-3.00415277204559));
#25801=CARTESIAN_POINT('Ctrl Pts',(95.7354697603805,-0.928159665744005,
-3.00449851642664));
#25802=CARTESIAN_POINT('Ctrl Pts',(95.7183195759232,-0.914642006552505,
-3.00595723620951));
#25803=CARTESIAN_POINT('Ctrl Pts',(95.7054345827661,-0.90403460007461,-3.00705395875899));
#25804=CARTESIAN_POINT('Ctrl Pts',(95.6706800978347,-0.874161776889747,
-3.01002809155301));
#25805=CARTESIAN_POINT('Ctrl Pts',(95.6492925576752,-0.854352285993023,
-3.01187649409323));
#25806=CARTESIAN_POINT('Ctrl Pts',(95.5621362240676,-0.767399590029131,
-3.0195969995126));
#25807=CARTESIAN_POINT('Ctrl Pts',(95.5037956008233,-0.693310107047775,
-3.02527350649935));
#25808=CARTESIAN_POINT('Ctrl Pts',(95.4393059161946,-0.587530097487091,
-3.0331834717284));
#25809=CARTESIAN_POINT('Ctrl Pts',(95.4247130109355,-0.561404137414405,
-3.03512036203158));
#25810=CARTESIAN_POINT('Ctrl Pts',(95.4068270695234,-0.526306401932507,
-3.03771699555707));
#25811=CARTESIAN_POINT('Ctrl Pts',(95.4026250787456,-0.517808724892698,
-3.03834523807455));
#25812=CARTESIAN_POINT('Ctrl Pts',(95.3959627046806,-0.50391578320374,-3.03937211072911));
#25813=CARTESIAN_POINT('Ctrl Pts',(95.3934396257025,-0.498550921419669,
-3.03976858489841));
#25814=CARTESIAN_POINT('Ctrl Pts',(95.3886589138722,-0.488183071325856,
-3.04053478908916));
#25815=CARTESIAN_POINT('Ctrl Pts',(95.3863955340879,-0.483182890668872,
-3.04090431161191));
#25816=CARTESIAN_POINT('Ctrl Pts',(95.3812228525201,-0.471539622694852,
-3.04176486484143));
#25817=CARTESIAN_POINT('Ctrl Pts',(95.3783398211502,-0.464885179296589,
-3.04225676575113));
#25818=CARTESIAN_POINT('Ctrl Pts',(95.3692851437974,-0.443445010976813,
-3.04384211959519));
#25819=CARTESIAN_POINT('Ctrl Pts',(95.3633539141323,-0.428560367553834,
-3.04494349646848));
#25820=CARTESIAN_POINT('Ctrl Pts',(95.350085191382,-0.393179483143595,-3.04756452643043));
#25821=CARTESIAN_POINT('Ctrl Pts',(95.3430088981202,-0.372592211810573,
-3.04909206523416));
#25822=CARTESIAN_POINT('Ctrl Pts',(95.3052665895603,-0.252015951827739,
-3.05805299057977));
#25823=CARTESIAN_POINT('Ctrl Pts',(95.2874611621814,-0.148497143163256,
-3.06586033474288));
#25824=CARTESIAN_POINT('Ctrl Pts',(95.2824332096335,-0.0140539367339928,
-3.07557432519419));
#25825=CARTESIAN_POINT('Ctrl Pts',(95.2824571030796,0.0159420902453292,
-3.07771027253911));
#25826=CARTESIAN_POINT('Ctrl Pts',(95.2838752319896,0.0522966082595831,
-3.08023711188907));
#25827=CARTESIAN_POINT('Ctrl Pts',(95.2841765124887,0.0586841184268421,
-3.08067874738934));
#25828=CARTESIAN_POINT('Ctrl Pts',(95.2847276222602,0.0686439736991038,
-3.08136341717221));
#25829=CARTESIAN_POINT('Ctrl Pts',(95.284941739024,0.0722180526845859,-3.0816083137778));
#25830=CARTESIAN_POINT('Ctrl Pts',(95.2853683390178,0.0788334248508394,
-3.08206005821494));
#25831=CARTESIAN_POINT('Ctrl Pts',(95.285576330699,0.0818748634086122,-3.0822671373571));
#25832=CARTESIAN_POINT('Ctrl Pts',(95.2860794563372,0.0888348830761416,
-3.0827396462324));
#25833=CARTESIAN_POINT('Ctrl Pts',(95.2863823937992,0.0927528231951996,
-3.08300464433913));
#25834=CARTESIAN_POINT('Ctrl Pts',(95.2873860459821,0.10493935535317,-3.08382603842329));
#25835=CARTESIAN_POINT('Ctrl Pts',(95.2881545597509,0.113202325216241,-3.08437886655753));
#25836=CARTESIAN_POINT('Ctrl Pts',(95.2901651417045,0.13259472029244,-3.08566808898048));
#25837=CARTESIAN_POINT('Ctrl Pts',(95.2914787440969,0.143716086875455,-3.08640107685722));
#25838=CARTESIAN_POINT('Ctrl Pts',(95.2967685301269,0.183608127972321,-3.08901279200894));
#25839=CARTESIAN_POINT('Ctrl Pts',(95.3016501620551,0.212249810345654,-3.0908552693653));
#25840=CARTESIAN_POINT('Ctrl Pts',(95.3264880732794,0.331225529647054,-3.09847801851818));
#25841=CARTESIAN_POINT('Ctrl Pts',(95.3559890002146,0.419223261554849,-3.10406770305709));
#25842=CARTESIAN_POINT('Ctrl Pts',(95.4088258103388,0.531124483469788,-3.11195668464847));
#25843=CARTESIAN_POINT('Ctrl Pts',(95.4232879883082,0.558840087648294,-3.11397770336914));
#25844=CARTESIAN_POINT('Ctrl Pts',(95.4436203206812,0.594291235280489,-3.116670740302));
#25845=CARTESIAN_POINT('Ctrl Pts',(95.4485084488211,0.602577181464901,-3.11730813667241));
#25846=CARTESIAN_POINT('Ctrl Pts',(95.4565879329454,0.615897219502984,-3.1183462413799));
#25847=CARTESIAN_POINT('Ctrl Pts',(95.4597170247295,0.620968709638013,-3.11874470304889));
#25848=CARTESIAN_POINT('Ctrl Pts',(95.4657965225961,0.630656775828993,-3.1195121943089));
#25849=CARTESIAN_POINT('Ctrl Pts',(95.4687409263771,0.635276949700458,-3.11988099781594));
#25850=CARTESIAN_POINT('Ctrl Pts',(95.4756199466394,0.645906697813495,-3.1207360888178));
#25851=CARTESIAN_POINT('Ctrl Pts',(95.4795774860086,0.65190110338251,-3.12122321175409));
#25852=CARTESIAN_POINT('Ctrl Pts',(95.4923246992689,0.670830154424144,-3.12277739129527));
#25853=CARTESIAN_POINT('Ctrl Pts',(95.5013169650072,0.683625651273023,-3.12385194063286));
#25854=CARTESIAN_POINT('Ctrl Pts',(95.5230280506598,0.713247418574105,-3.12639779494679));
#25855=CARTESIAN_POINT('Ctrl Pts',(95.5359490471729,0.729918135479005,-3.12787638707241));
#25856=CARTESIAN_POINT('Ctrl Pts',(95.5862113649606,0.79128987719799,-3.13349598633765));
#25857=CARTESIAN_POINT('Ctrl Pts',(95.6264002402084,0.833543628443717,-3.13773559407867));
#25858=CARTESIAN_POINT('Ctrl Pts',(95.722952260825,0.921054912916952,-3.14729289549292));
#25859=CARTESIAN_POINT('Ctrl Pts',(95.7806959365638,0.964460927588447,-3.15261008441173));
#25860=CARTESIAN_POINT('Ctrl Pts',(95.8503237999271,1.00742136910774,-3.15834341172623));
#25861=CARTESIAN_POINT('Ctrl Pts',(95.8586600977274,1.01242344881201,-3.15901943370131));
#25862=CARTESIAN_POINT('Ctrl Pts',(95.8704167543442,1.01928133038278,-3.15995736172232));
#25863=CARTESIAN_POINT('Ctrl Pts',(95.873785548795,1.02122411484335,-3.16022436430213));
#25864=CARTESIAN_POINT('Ctrl Pts',(95.8796351478772,1.02455908019468,-3.16068487908988));
#25865=CARTESIAN_POINT('Ctrl Pts',(95.8821114619338,1.02595901007983,-3.16087887064855));
#25866=CARTESIAN_POINT('Ctrl Pts',(95.8873727962883,1.02890828723372,-3.16128897029248));
#25867=CARTESIAN_POINT('Ctrl Pts',(95.8901590838189,1.03045533084014,-3.16150492736123));
#25868=CARTESIAN_POINT('Ctrl Pts',(95.8971343673452,1.0342912921111,-3.16204260135164));
#25869=CARTESIAN_POINT('Ctrl Pts',(95.9013311178489,1.0365661176592,-3.16236344592702));
#25870=CARTESIAN_POINT('Ctrl Pts',(95.910939416062,1.04169890833297,-3.1630922433017));
#25871=CARTESIAN_POINT('Ctrl Pts',(95.9163595808209,1.04454030537047,-3.16349922992478));
#25872=CARTESIAN_POINT('Ctrl Pts',(95.9218016730922,1.04733934309078,-3.1639039911222));
#25873=CARTESIAN_POINT('Origin',(96.460480949577,-7.19464945638997E-16,
0.924367114736168));
#25874=CARTESIAN_POINT('',(95.921801595944,1.04733930341107,-3.76190742309816));
#25875=CARTESIAN_POINT('',(95.9218017102038,1.04733936217843,-3.66210953954391));
#25876=CARTESIAN_POINT('',(95.9218016730721,1.04733934308042,0.924367114736168));
#25877=CARTESIAN_POINT('Ctrl Pts',(95.921801595944,1.04733930341107,-3.76190742309816));
#25878=CARTESIAN_POINT('Ctrl Pts',(95.8962264988879,1.03418523127187,-3.76011579365399));
#25879=CARTESIAN_POINT('Ctrl Pts',(95.8711315530826,1.02009353307782,-3.75831047647257));
#25880=CARTESIAN_POINT('Ctrl Pts',(95.8274863741028,0.993434893227348,-3.75505698510355));
#25881=CARTESIAN_POINT('Ctrl Pts',(95.8087413652297,0.981239237558241,-3.75362027545444));
#25882=CARTESIAN_POINT('Ctrl Pts',(95.7769064042041,0.959212374883115,-3.75110111045232));
#25883=CARTESIAN_POINT('Ctrl Pts',(95.7636530284024,0.949628003487759,-3.75002742763029));
#25884=CARTESIAN_POINT('Ctrl Pts',(95.7447697826221,0.935364125973282,-3.74845863469301));
#25885=CARTESIAN_POINT('Ctrl Pts',(95.738976823307,0.930902956494515,-3.74797189496362));
#25886=CARTESIAN_POINT('Ctrl Pts',(95.7289013511859,0.922993272446278,-3.74711546572422));
#25887=CARTESIAN_POINT('Ctrl Pts',(95.7246007061124,0.919568135210955,-3.7467466991317));
#25888=CARTESIAN_POINT('Ctrl Pts',(95.7162901545888,0.912853778048933,-3.74602774492841));
#25889=CARTESIAN_POINT('Ctrl Pts',(95.712277676495,0.909567930454248,-3.74567769681928));
#25890=CARTESIAN_POINT('Ctrl Pts',(95.7015897637707,0.900696943966807,-3.74473732240066));
#25891=CARTESIAN_POINT('Ctrl Pts',(95.6949544280044,0.895064218078987,-3.74414509196726));
#25892=CARTESIAN_POINT('Ctrl Pts',(95.6704592311989,0.873798657840505,-3.74192665430579));
#25893=CARTESIAN_POINT('Ctrl Pts',(95.6530118441587,0.857701529376837,-3.74028160503915));
#25894=CARTESIAN_POINT('Ctrl Pts',(95.5640698078699,0.77052249533053,-3.73153996219475));
#25895=CARTESIAN_POINT('Ctrl Pts',(95.5014426631754,0.691011472349212,-3.72407534013313));
#25896=CARTESIAN_POINT('Ctrl Pts',(95.4344131552923,0.578937511781002,-3.71455120705597));
#25897=CARTESIAN_POINT('Ctrl Pts',(95.4200874088515,0.552779594576922,-3.71239441864231));
#25898=CARTESIAN_POINT('Ctrl Pts',(95.3991999679067,0.510945047567632,-3.70907446133398));
#25899=CARTESIAN_POINT('Ctrl Pts',(95.3919585338193,0.49562292557937,-3.70788471077241));
#25900=CARTESIAN_POINT('Ctrl Pts',(95.3829385801679,0.475420154483092,-3.70635466661999));
#25901=CARTESIAN_POINT('Ctrl Pts',(95.3808584845957,0.470677402008181,-3.70599821894912));
#25902=CARTESIAN_POINT('Ctrl Pts',(95.3775141468252,0.462913265513497,-3.70541933722816));
#25903=CARTESIAN_POINT('Ctrl Pts',(95.3762311314206,0.459900119314074,-3.7051958156858));
#25904=CARTESIAN_POINT('Ctrl Pts',(95.3737529118436,0.454012034748813,-3.70476128791256));
#25905=CARTESIAN_POINT('Ctrl Pts',(95.3725565172301,0.451137656956187,-3.70455021577775));
#25906=CARTESIAN_POINT('Ctrl Pts',(95.3699113050293,0.444710728563006,-3.70408054294366));
#25907=CARTESIAN_POINT('Ctrl Pts',(95.3684684060854,0.441155740741356,-3.70382229017021));
#25908=CARTESIAN_POINT('Ctrl Pts',(95.363544123011,0.428851179380597,-3.70293352696014));
#25909=CARTESIAN_POINT('Ctrl Pts',(95.3601502074514,0.42006666988485,-3.70230790123492));
#25910=CARTESIAN_POINT('Ctrl Pts',(95.3296010061518,0.338084100915692,-3.6965429068482));
#25911=CARTESIAN_POINT('Ctrl Pts',(95.3096779079478,0.262385658831466,-3.69175436383144));
#25912=CARTESIAN_POINT('Ctrl Pts',(95.2888559946576,0.131664971017972,-3.68356457278708));
#25913=CARTESIAN_POINT('Ctrl Pts',(95.2840341658322,0.0775437903394788,
-3.68019718458866));
#25914=CARTESIAN_POINT('Ctrl Pts',(95.2825609572128,0.0030483911169273,
-3.67543985621155));
#25915=CARTESIAN_POINT('Ctrl Pts',(95.2826825629583,-0.017195661879143,
-3.67413516945524));
#25916=CARTESIAN_POINT('Ctrl Pts',(95.283807263385,-0.0525710119043245,
-3.67182744559456));
#25917=CARTESIAN_POINT('Ctrl Pts',(95.2845810093655,-0.067705034108542,
-3.67083125761951));
#25918=CARTESIAN_POINT('Ctrl Pts',(95.2861453524805,-0.0898960275837626,
-3.66935552085773));
#25919=CARTESIAN_POINT('Ctrl Pts',(95.286708137701,-0.0969678957148688,
-3.66888298825782));
#25920=CARTESIAN_POINT('Ctrl Pts',(95.287817686569,-0.109479781345357,-3.66804279454567));
#25921=CARTESIAN_POINT('Ctrl Pts',(95.2883385101261,-0.11492193372713,-3.66767594671396));
#25922=CARTESIAN_POINT('Ctrl Pts',(95.2895105943463,-0.126330979195489,
-3.66690385215306));
#25923=CARTESIAN_POINT('Ctrl Pts',(95.2901696160824,-0.13229689916204,-3.6664983745375));
#25924=CARTESIAN_POINT('Ctrl Pts',(95.2920265406785,-0.14800579512436,-3.66542598756796));
#25925=CARTESIAN_POINT('Ctrl Pts',(95.2933006790065,-0.157739110368548,
-3.66475673126597));
#25926=CARTESIAN_POINT('Ctrl Pts',(95.2993932951894,-0.200154527426412,
-3.66181855588219));
#25927=CARTESIAN_POINT('Ctrl Pts',(95.3054635441935,-0.232638774721101,
-3.65951127919769));
#25928=CARTESIAN_POINT('Ctrl Pts',(95.3311628016828,-0.344004827360322,
-3.65139786216768));
#25929=CARTESIAN_POINT('Ctrl Pts',(95.3575799294867,-0.421076181429397,
-3.64540523707158));
#25930=CARTESIAN_POINT('Ctrl Pts',(95.4065519807671,-0.52685511090678,-3.63687455410522));
#25931=CARTESIAN_POINT('Ctrl Pts',(95.4228262813435,-0.558225495885777,
-3.6343060402724));
#25932=CARTESIAN_POINT('Ctrl Pts',(95.449954883054,-0.605219594611901,-3.63044159753571));
#25933=CARTESIAN_POINT('Ctrl Pts',(95.4598175707864,-0.621390852404269,
-3.62910871906064));
#25934=CARTESIAN_POINT('Ctrl Pts',(95.4729797914285,-0.641845391255723,
-3.62742538307828));
#25935=CARTESIAN_POINT('Ctrl Pts',(95.4759240040404,-0.646352587528858,
-3.62705462421256));
#25936=CARTESIAN_POINT('Ctrl Pts',(95.4807337916269,-0.653606603193718,
-3.62645838484702));
#25937=CARTESIAN_POINT('Ctrl Pts',(95.4825802158884,-0.656365935278397,
-3.62623169457153));
#25938=CARTESIAN_POINT('Ctrl Pts',(95.4861661811299,-0.661676149546743,
-3.62579571092749));
#25939=CARTESIAN_POINT('Ctrl Pts',(95.487904109929,-0.664228037739306,-3.62558632161974));
#25940=CARTESIAN_POINT('Ctrl Pts',(95.4917659109567,-0.669850862114665,
-3.62512517314593));
#25941=CARTESIAN_POINT('Ctrl Pts',(95.4938944118356,-0.672918620287419,
-3.62487371930569));
#25942=CARTESIAN_POINT('Ctrl Pts',(95.5014732419932,-0.683731652578977,
-3.62398772343226));
#25943=CARTESIAN_POINT('Ctrl Pts',(95.5070025420534,-0.691421504081438,
-3.62335820345055));
#25944=CARTESIAN_POINT('Ctrl Pts',(95.5603202558847,-0.763716732617802,
-3.6174365589991));
#25945=CARTESIAN_POINT('Ctrl Pts',(95.6145173496878,-0.823348013849373,
-3.61251740585219));
#25946=CARTESIAN_POINT('Ctrl Pts',(95.7137126148767,-0.912262644176052,
-3.60427325709178));
#25947=CARTESIAN_POINT('Ctrl Pts',(95.7553778495771,-0.944836011124048,
-3.60099125938578));
#25948=CARTESIAN_POINT('Ctrl Pts',(95.8155685444667,-0.985687509875306,
-3.59634396703402));
#25949=CARTESIAN_POINT('Ctrl Pts',(95.8323314437918,-0.996453715932912,
-3.59505939547738));
#25950=CARTESIAN_POINT('Ctrl Pts',(95.8621527900226,-1.01455531102816,-3.59278408031653));
#25951=CARTESIAN_POINT('Ctrl Pts',(95.8750933488403,-1.02207650874092,-3.59179991554965));
#25952=CARTESIAN_POINT('Ctrl Pts',(95.8943432725977,-1.03277927477638,-3.59033866677666));
#25953=CARTESIAN_POINT('Ctrl Pts',(95.9005438922124,-1.03615413325488,-3.58986839939262));
#25954=CARTESIAN_POINT('Ctrl Pts',(95.9115956012941,-1.04204115886769,-3.58903076081365));
#25955=CARTESIAN_POINT('Ctrl Pts',(95.9164345745886,-1.04457572367029,-3.58866418554441));
#25956=CARTESIAN_POINT('Ctrl Pts',(95.9266427573101,-1.04983240757999,-3.5878911598405));
#25957=CARTESIAN_POINT('Ctrl Pts',(95.9320155411572,-1.05254720051486,-3.58748446836076));
#25958=CARTESIAN_POINT('Ctrl Pts',(95.9462756734567,-1.05961593810717,-3.58640536236708));
#25959=CARTESIAN_POINT('Ctrl Pts',(95.9551973350177,-1.06389917791706,-3.58573054753544));
#25960=CARTESIAN_POINT('Ctrl Pts',(95.9948540124099,-1.08232679792293,-3.5827316185277));
#25961=CARTESIAN_POINT('Ctrl Pts',(96.0261334911932,-1.09525413997415,-3.58036715298766));
#25962=CARTESIAN_POINT('Ctrl Pts',(96.1422458488791,-1.13748508981621,-3.57158860392831));
#25963=CARTESIAN_POINT('Ctrl Pts',(96.2297909045413,-1.15841458722514,-3.56493905067645));
#25964=CARTESIAN_POINT('Ctrl Pts',(96.3474409737906,-1.17266649041917,-3.55630281782057));
#25965=CARTESIAN_POINT('Ctrl Pts',(96.3761553931163,-1.17508048918689,-3.55422103812789));
#25966=CARTESIAN_POINT('Ctrl Pts',(96.4214695994568,-1.17722016024378,-3.55100208231746));
#25967=CARTESIAN_POINT('Ctrl Pts',(96.4380236986057,-1.17765229675402,-3.54984007601831));
#25968=CARTESIAN_POINT('Ctrl Pts',(96.4597184651846,-1.17776095235082,-3.54833999634666));
#25969=CARTESIAN_POINT('Ctrl Pts',(96.4648547568724,-1.17775307875157,-3.54798652206235));
#25970=CARTESIAN_POINT('Ctrl Pts',(96.473256358879,-1.17768523596426,-3.54741124523273));
#25971=CARTESIAN_POINT('Ctrl Pts',(96.4765216948585,-1.17764528668139,-3.54718838002288));
#25972=CARTESIAN_POINT('Ctrl Pts',(96.4829060535945,-1.17754061888076,-3.5467540977208));
#25973=CARTESIAN_POINT('Ctrl Pts',(96.4860250441665,-1.17747708852005,-3.54654262118865));
#25974=CARTESIAN_POINT('Ctrl Pts',(96.4930027468704,-1.17730722229821,-3.5460709765356));
#25975=CARTESIAN_POINT('Ctrl Pts',(96.4968612991698,-1.17719430604323,-3.5458111661792));
#25976=CARTESIAN_POINT('Ctrl Pts',(96.5102662788259,-1.17673605151267,-3.54491182273778));
#25977=CARTESIAN_POINT('Ctrl Pts',(96.5198093137165,-1.17629353198926,-3.54427732868217));
#25978=CARTESIAN_POINT('Ctrl Pts',(96.6044455846745,-1.17133620334127,-3.53869274241208));
#25979=CARTESIAN_POINT('Ctrl Pts',(96.6789619343092,-1.15975153802912,-3.53406714360415));
#25980=CARTESIAN_POINT('Ctrl Pts',(96.8062777120929,-1.12724116350638,-3.52593891566542));
#25981=CARTESIAN_POINT('Ctrl Pts',(96.8596163749504,-1.10947659329195,-3.5224607679926));
#25982=CARTESIAN_POINT('Ctrl Pts',(96.930558248863,-1.08006889329543,-3.51756105189604));
#25983=CARTESIAN_POINT('Ctrl Pts',(96.9494219607149,-1.07166137117709,-3.51623088690277));
#25984=CARTESIAN_POINT('Ctrl Pts',(96.9819394448575,-1.05613109045067,-3.51388218815197));
#25985=CARTESIAN_POINT('Ctrl Pts',(96.9956929073246,-1.04922827221261,-3.51287085445709));
#25986=CARTESIAN_POINT('Ctrl Pts',(97.0156218807661,-1.03873218555018,-3.51137688655667));
#25987=CARTESIAN_POINT('Ctrl Pts',(97.0219065880417,-1.03534885690895,-3.51090152394723));
#25988=CARTESIAN_POINT('Ctrl Pts',(97.0329551301552,-1.02927077412618,-3.51005812405196));
#25989=CARTESIAN_POINT('Ctrl Pts',(97.0377317041404,-1.02659952198082,-3.50969092177131));
#25990=CARTESIAN_POINT('Ctrl Pts',(97.047689226528,-1.02093940866751,-3.50891992192117));
#25991=CARTESIAN_POINT('Ctrl Pts',(97.0528663584122,-1.0179441840367,-3.5085159058378));
#25992=CARTESIAN_POINT('Ctrl Pts',(97.0663961499154,-1.00997836820594,-3.50745160869495));
#25993=CARTESIAN_POINT('Ctrl Pts',(97.0747103381124,-1.0049436713989,-3.50678904432556));
#25994=CARTESIAN_POINT('Ctrl Pts',(97.110266067293,-0.982806660159659,-3.50391778512569));
#25995=CARTESIAN_POINT('Ctrl Pts',(97.1368607178075,-0.964696686773595,
-3.50167284305935));
#25996=CARTESIAN_POINT('Ctrl Pts',(97.2285274714655,-0.896619826873043,
-3.49357537072678));
#25997=CARTESIAN_POINT('Ctrl Pts',(97.289080930863,-0.840976518992091,-3.48752804788429));
#25998=CARTESIAN_POINT('Ctrl Pts',(97.377603802382,-0.740714807832277,-3.47773879451204));
#25999=CARTESIAN_POINT('Ctrl Pts',(97.4092632435488,-0.699704359762225,
-3.47398576019866));
#26000=CARTESIAN_POINT('Ctrl Pts',(97.4420009167106,-0.650969990066961,
-3.46990245875859));
#26001=CARTESIAN_POINT('Ctrl Pts',(97.4458257131345,-0.645165929519488,
-3.46942191133067));
#26002=CARTESIAN_POINT('Ctrl Pts',(97.4515858863273,-0.636254244431529,
-3.46869320772909));
#26003=CARTESIAN_POINT('Ctrl Pts',(97.4535584515858,-0.63317101570372,-3.46844274435539));
#26004=CARTESIAN_POINT('Ctrl Pts',(97.4571443017282,-0.627508152449101,
-3.46798581185558));
#26005=CARTESIAN_POINT('Ctrl Pts',(97.4587619710553,-0.624931453451115,
-3.46777906765202));
#26006=CARTESIAN_POINT('Ctrl Pts',(97.4623926647974,-0.619098242158763,
-3.46731364558971));
#26007=CARTESIAN_POINT('Ctrl Pts',(97.4643998082453,-0.615838164443482,
-3.46705534705968));
#26008=CARTESIAN_POINT('Ctrl Pts',(97.4695486247545,-0.607383194516477,
-3.46638998155709));
#26009=CARTESIAN_POINT('Ctrl Pts',(97.4726661385212,-0.602173617142791,
-3.46598440338801));
#26010=CARTESIAN_POINT('Ctrl Pts',(97.4933986779388,-0.566912174135319,
-3.46326702613465));
#26011=CARTESIAN_POINT('Ctrl Pts',(97.5097150960555,-0.536112548932825,
-3.46102857825812));
#26012=CARTESIAN_POINT('Ctrl Pts',(97.563716282685,-0.422235373459249,-3.45306653781826));
#26013=CARTESIAN_POINT('Ctrl Pts',(97.5930880658869,-0.335579168232345,
-3.44756652821645));
#26014=CARTESIAN_POINT('Ctrl Pts',(97.6204722495787,-0.207583335840273,
-3.43929000611338));
#26015=CARTESIAN_POINT('Ctrl Pts',(97.6268082783092,-0.168376682339155,
-3.43673920724081));
#26016=CARTESIAN_POINT('Ctrl Pts',(97.6322501521289,-0.118964187548293,
-3.43346637123012));
#26017=CARTESIAN_POINT('Ctrl Pts',(97.633220193476,-0.108987144238704,-3.4328026795988));
#26018=CARTESIAN_POINT('Ctrl Pts',(97.6345710856818,-0.092973047211535,
-3.43173226013924));
#26019=CARTESIAN_POINT('Ctrl Pts',(97.6350329985036,-0.0869431841124467,
-3.43132804750004));
#26020=CARTESIAN_POINT('Ctrl Pts',(97.6358232727898,-0.075466912115708,
-3.43055640275571));
#26021=CARTESIAN_POINT('Ctrl Pts',(97.6361602662685,-0.0700212406777715,
-3.43018924815991));
#26022=CARTESIAN_POINT('Ctrl Pts',(97.6368435681495,-0.0575773083010886,
-3.42934789167097));
#26023=CARTESIAN_POINT('Ctrl Pts',(97.6371652840934,-0.0505779600130338,
-3.42887294246872));
#26024=CARTESIAN_POINT('Ctrl Pts',(97.637967888394,-0.028900574278145,-3.4273964788855));
#26025=CARTESIAN_POINT('Ctrl Pts',(97.6382366922115,-0.014216586273703,
-3.42638849319511));
#26026=CARTESIAN_POINT('Ctrl Pts',(97.638207738034,0.0586443039133953,-3.42134582836754));
#26027=CARTESIAN_POINT('Ctrl Pts',(97.6338742324366,0.116730217766737,-3.41718986520103));
#26028=CARTESIAN_POINT('Ctrl Pts',(97.6162402326283,0.234605498196122,-3.40851686435091));
#26029=CARTESIAN_POINT('Ctrl Pts',(97.602534286478,0.294165280185552,-3.40400491838927));
#26030=CARTESIAN_POINT('Ctrl Pts',(97.5793544758938,0.368086347227076,-3.39837246677786));
#26031=CARTESIAN_POINT('Ctrl Pts',(97.5741054044671,0.383674523097038,-3.3971832509645));
#26032=CARTESIAN_POINT('Ctrl Pts',(97.5606007426072,0.421163975046063,-3.39432680599592));
#26033=CARTESIAN_POINT('Ctrl Pts',(97.5520150376988,0.442940362539929,-3.39267059675925));
#26034=CARTESIAN_POINT('Ctrl Pts',(97.5404126312541,0.46997747793587,-3.39063008814944));
#26035=CARTESIAN_POINT('Ctrl Pts',(97.5379974106486,0.475488745211111,-3.3902149957794));
#26036=CARTESIAN_POINT('Ctrl Pts',(97.5341270008379,0.484139639058019,-3.38956504402371));
#26037=CARTESIAN_POINT('Ctrl Pts',(97.5327000735977,0.487291683038719,-3.38932856603096));
#26038=CARTESIAN_POINT('Ctrl Pts',(97.5299807007787,0.493228924272358,-3.38888383528646));
#26039=CARTESIAN_POINT('Ctrl Pts',(97.5286912643782,0.496015335597813,-3.38867542018727));
#26040=CARTESIAN_POINT('Ctrl Pts',(97.5256437404625,0.502533889484588,-3.38818851158696));
#26041=CARTESIAN_POINT('Ctrl Pts',(97.5238769217997,0.50626187759933,-3.38791054987453));
#26042=CARTESIAN_POINT('Ctrl Pts',(97.5180369140199,0.518418827179166,-3.38700551875452));
#26043=CARTESIAN_POINT('Ctrl Pts',(97.5138826896912,0.526808775313851,-3.38638313543998));
#26044=CARTESIAN_POINT('Ctrl Pts',(97.4903554219877,0.572933495398094,-3.38296889380943));
#26045=CARTESIAN_POINT('Ctrl Pts',(97.469052749589,0.609653949941007,-3.38027783432291));
#26046=CARTESIAN_POINT('Ctrl Pts',(97.4338745102181,0.663381494102728,-3.3762617896122));
#26047=CARTESIAN_POINT('Ctrl Pts',(97.4214322754108,0.681280131640827,-3.37490981259047));
#26048=CARTESIAN_POINT('Ctrl Pts',(97.3557183708018,0.770427180692221,-3.36805311642911));
#26049=CARTESIAN_POINT('Ctrl Pts',(97.2950011783242,0.83581214368228,-3.36258621162187));
#26050=CARTESIAN_POINT('Ctrl Pts',(97.2160848308699,0.903539914513462,-3.35580436483116));
#26051=CARTESIAN_POINT('Ctrl Pts',(97.204476755838,0.913122012347313,-3.35481474361452));
#26052=CARTESIAN_POINT('Ctrl Pts',(97.1872063250918,0.926830234182048,-3.35335195268731));
#26053=CARTESIAN_POINT('Ctrl Pts',(97.1816854104147,0.931132738410469,-3.35288573057784));
#26054=CARTESIAN_POINT('Ctrl Pts',(97.1717820923058,0.938709576764417,-3.35205170886831));
#26055=CARTESIAN_POINT('Ctrl Pts',(97.1674145728991,0.942003097474619,-3.3516846685469));
#26056=CARTESIAN_POINT('Ctrl Pts',(97.1582162864729,0.948839474814292,-3.35091318344318));
#26057=CARTESIAN_POINT('Ctrl Pts',(97.1533811266725,0.952376129275639,-3.35050851460131));
#26058=CARTESIAN_POINT('Ctrl Pts',(97.1405956728279,0.961579085619236,-3.34944060422895));
#26059=CARTESIAN_POINT('Ctrl Pts',(97.1326016777581,0.967183587268537,-3.34877505104877));
#26060=CARTESIAN_POINT('Ctrl Pts',(97.0944990655968,0.993196402963338,-3.34561203107023));
#26061=CARTESIAN_POINT('Ctrl Pts',(97.063528181944,1.01230015869973,-3.34306716432496));
#26062=CARTESIAN_POINT('Ctrl Pts',(96.9749446917226,1.06143207068858,-3.33585510726276));
#26063=CARTESIAN_POINT('Ctrl Pts',(96.9156616083976,1.0881727534905,-3.33109677911087));
#26064=CARTESIAN_POINT('Ctrl Pts',(96.7984090821579,1.12979658947852,-3.32196642117665));
#26065=CARTESIAN_POINT('Ctrl Pts',(96.740900057033,1.14542669015451,-3.31761019633741));
#26066=CARTESIAN_POINT('Ctrl Pts',(96.6726127546298,1.15853162007676,-3.31273421598941));
#26067=CARTESIAN_POINT('Ctrl Pts',(96.6627504502367,1.16029413646768,-3.31203721367748));
#26068=CARTESIAN_POINT('Ctrl Pts',(96.6489806169948,1.16257406284862,-3.31107515432437));
#26069=CARTESIAN_POINT('Ctrl Pts',(96.6450915017148,1.1631979717049,-3.31080466205198));
#26070=CARTESIAN_POINT('Ctrl Pts',(96.6383758007135,1.16424080352314,-3.31033978055128));
#26071=CARTESIAN_POINT('Ctrl Pts',(96.6355507163483,1.16466896749941,-3.31014489083879));
#26072=CARTESIAN_POINT('Ctrl Pts',(96.6295858599768,1.1655507948362,-3.30973485786621));
#26073=CARTESIAN_POINT('Ctrl Pts',(96.6264457620266,1.16600206154691,-3.30951985524483));
#26074=CARTESIAN_POINT('Ctrl Pts',(96.6186466716879,1.16709073285635,-3.3089878808779));
#26075=CARTESIAN_POINT('Ctrl Pts',(96.6139855497869,1.16771294158852,-3.30867174182828));
#26076=CARTESIAN_POINT('Ctrl Pts',(96.5963734615488,1.16995668300139,-3.30748355424475));
#26077=CARTESIAN_POINT('Ctrl Pts',(96.5833990054547,1.17139088320151,-3.30662117896036));
#26078=CARTESIAN_POINT('Ctrl Pts',(96.5499951971362,1.17452219619262,-3.30442793140284));
#26079=CARTESIAN_POINT('Ctrl Pts',(96.52953995878,1.17590226754377,-3.30311071553934));
#26080=CARTESIAN_POINT('Ctrl Pts',(96.4512988131533,1.17913211951348,-3.29813602601166));
#26081=CARTESIAN_POINT('Ctrl Pts',(96.3934390981789,1.17726082863896,-3.29458641741194));
#26082=CARTESIAN_POINT('Ctrl Pts',(96.2609143845635,1.16316892189656,-3.28633432851085));
#26083=CARTESIAN_POINT('Ctrl Pts',(96.1868318697482,1.14799944623993,-3.28162174921314));
#26084=CARTESIAN_POINT('Ctrl Pts',(96.1047829235298,1.12280092345165,-3.27598861093874));
#26085=CARTESIAN_POINT('Ctrl Pts',(96.0948925300866,1.11961962102213,-3.27530278492724));
#26086=CARTESIAN_POINT('Ctrl Pts',(96.0786710410923,1.11416403186653,-3.27416605014586));
#26087=CARTESIAN_POINT('Ctrl Pts',(96.0723149093042,1.1119655651825,-3.27371760087763));
#26088=CARTESIAN_POINT('Ctrl Pts',(96.0608629271379,1.1078943857459,-3.27290394844389));
#26089=CARTESIAN_POINT('Ctrl Pts',(96.05576049814,1.10604063593009,-3.27253937488855));
#26090=CARTESIAN_POINT('Ctrl Pts',(96.0448364989843,1.10198615500307,-3.27175434162039));
#26091=CARTESIAN_POINT('Ctrl Pts',(96.0390192139224,1.09977443048098,-3.27133352856879));
#26092=CARTESIAN_POINT('Ctrl Pts',(96.0231237928433,1.09358637410383,-3.27017593173458));
#26093=CARTESIAN_POINT('Ctrl Pts',(96.0130827768813,1.0895170038342,-3.26943608845137));
#26094=CARTESIAN_POINT('Ctrl Pts',(95.975517817703,1.07368602990993,-3.2666348868698));
#26095=CARTESIAN_POINT('Ctrl Pts',(95.9483992295894,1.0610192972329,-3.26454426774695));
#26096=CARTESIAN_POINT('Ctrl Pts',(95.9218016227097,1.04733931717749,-3.26242343814143));
#26097=CARTESIAN_POINT('',(97.6382307499679,0.00068569618098675,-3.32647283958636));
#26098=CARTESIAN_POINT('Ctrl Pts',(95.9218016730922,1.04733934309078,-3.1639039911222));
#26099=CARTESIAN_POINT('Ctrl Pts',(95.9284350625409,1.05075110208983,-3.1643973562697));
#26100=CARTESIAN_POINT('Ctrl Pts',(95.9351010302927,1.05409992667817,-3.16488741516598));
#26101=CARTESIAN_POINT('Ctrl Pts',(95.9612454033876,1.06692460104026,-3.16678894697688));
#26102=CARTESIAN_POINT('Ctrl Pts',(95.9809527995633,1.07592616055621,-3.16817824435421));
#26103=CARTESIAN_POINT('Ctrl Pts',(96.0952895725782,1.1243844560262,-3.17605087310667));
#26104=CARTESIAN_POINT('Ctrl Pts',(96.1945005918812,1.1518948418863,-3.18219704691524));
#26105=CARTESIAN_POINT('Ctrl Pts',(96.32799003106,1.17071913262763,-3.19078126878048));
#26106=CARTESIAN_POINT('Ctrl Pts',(96.3601241296241,1.1739102812802,-3.19286697222096));
#26107=CARTESIAN_POINT('Ctrl Pts',(96.4020620541466,1.17634051244649,-3.19563445854756));
#26108=CARTESIAN_POINT('Ctrl Pts',(96.4117838164527,1.1767830507194,-3.19627911828201));
#26109=CARTESIAN_POINT('Ctrl Pts',(96.4274898788756,1.17730304227345,-3.19732613959883));
#26110=CARTESIAN_POINT('Ctrl Pts',(96.4334713720535,1.17745545333156,-3.19772618150922));
#26111=CARTESIAN_POINT('Ctrl Pts',(96.4449243089704,1.17765996400205,-3.19849474863586));
#26112=CARTESIAN_POINT('Ctrl Pts',(96.4503954766207,1.17771952577118,-3.19886303327881));
#26113=CARTESIAN_POINT('Ctrl Pts',(96.4629977142343,1.17776889896263,-3.19971404136749));
#26114=CARTESIAN_POINT('Ctrl Pts',(96.4701286133761,1.17773207147511,-3.20019757423244));
#26115=CARTESIAN_POINT('Ctrl Pts',(96.4926111628343,1.17741176347643,-3.20172860340908));
#26116=CARTESIAN_POINT('Ctrl Pts',(96.5079573128253,1.17689284463589,-3.2027832802902));
#26117=CARTESIAN_POINT('Ctrl Pts',(96.5438509897074,1.17497596908158,-3.20527379517967));
#26118=CARTESIAN_POINT('Ctrl Pts',(96.5643801686324,1.17333880670873,-3.20671649674668));
#26119=CARTESIAN_POINT('Ctrl Pts',(96.6404270569036,1.16526287136231,-3.21212925456227));
#26120=CARTESIAN_POINT('Ctrl Pts',(96.6955028727292,1.15541404314257,-3.21619008429051));
#26121=CARTESIAN_POINT('Ctrl Pts',(96.8230009295493,1.12311949178227,-3.22583061178204));
#26122=CARTESIAN_POINT('Ctrl Pts',(96.8943813540385,1.09752014226995,-3.23142230417399));
#26123=CARTESIAN_POINT('Ctrl Pts',(96.971433199885,1.06118499951821,-3.23738942722104));
#26124=CARTESIAN_POINT('Ctrl Pts',(96.9799998951076,1.05701744777285,-3.23805165093634));
#26125=CARTESIAN_POINT('Ctrl Pts',(96.9919615396042,1.05101774886761,-3.23897366347195));
#26126=CARTESIAN_POINT('Ctrl Pts',(96.9953992196052,1.04927230567082,-3.23923833158901));
#26127=CARTESIAN_POINT('Ctrl Pts',(97.0016016228565,1.04608470118273,-3.23971521078501));
#26128=CARTESIAN_POINT('Ctrl Pts',(97.0043693027853,1.04464838350147,-3.23992777268958));
#26129=CARTESIAN_POINT('Ctrl Pts',(97.009966939946,1.04171515186747,-3.24035715609558));
#26130=CARTESIAN_POINT('Ctrl Pts',(97.0127965466701,1.04021766619817,-3.24057394072053));
#26131=CARTESIAN_POINT('Ctrl Pts',(97.0199897449005,1.03637325258533,-3.24112443758274));
#26132=CARTESIAN_POINT('Ctrl Pts',(97.0243447509081,1.03401026418261,-3.2414571659441));
#26133=CARTESIAN_POINT('Ctrl Pts',(97.0338576271679,1.02877068564333,-3.24218301782307));
#26134=CARTESIAN_POINT('Ctrl Pts',(97.0390090663219,1.02588262464877,-3.24257546876886));
#26135=CARTESIAN_POINT('Ctrl Pts',(97.0540581627215,1.01729621164579,-3.24372079561052));
#26136=CARTESIAN_POINT('Ctrl Pts',(97.0638951966319,1.01149234193363,-3.24446797570809));
#26137=CARTESIAN_POINT('Ctrl Pts',(97.0992031296901,0.989962136732548,-3.24715023311478));
#26138=CARTESIAN_POINT('Ctrl Pts',(97.1241580883341,0.973408426531692,-3.24904692946635));
#26139=CARTESIAN_POINT('Ctrl Pts',(97.2305040515468,0.896871270219678,-3.25725587227644));
#26140=CARTESIAN_POINT('Ctrl Pts',(97.3046040967562,0.827508243602876,-3.26335290274558));
#26141=CARTESIAN_POINT('Ctrl Pts',(97.3838153983031,0.731501932619335,-3.27136494343075));
#26142=CARTESIAN_POINT('Ctrl Pts',(97.3981522053595,0.713031611950603,-3.27288758850829));
#26143=CARTESIAN_POINT('Ctrl Pts',(97.4170290756989,0.687157636279639,-3.27500296491219));
#26144=CARTESIAN_POINT('Ctrl Pts',(97.4220516396637,0.680111561468263,-3.27557728960866));
#26145=CARTESIAN_POINT('Ctrl Pts',(97.4299539266813,0.668763039589785,-3.27649988508025));
#26146=CARTESIAN_POINT('Ctrl Pts',(97.4328837759791,0.664495747324605,-3.27684626245233));
#26147=CARTESIAN_POINT('Ctrl Pts',(97.4388698753604,0.655652689820493,-3.27756303066356));
#26148=CARTESIAN_POINT('Ctrl Pts',(97.4419223733568,0.65107455002475,-3.27793354967336));
#26149=CARTESIAN_POINT('Ctrl Pts',(97.4489736001787,0.640336841822631,-3.2788013736127));
#26150=CARTESIAN_POINT('Ctrl Pts',(97.4529469845707,0.634160986220808,-3.27929959498285));
#26151=CARTESIAN_POINT('Ctrl Pts',(97.4656803733759,0.613956604907375,-3.28092684771773));
#26152=CARTESIAN_POINT('Ctrl Pts',(97.4742023553827,0.599781174775953,-3.28206440231029));
#26153=CARTESIAN_POINT('Ctrl Pts',(97.4937019069202,0.565742347608503,-3.28478767209151));
#26154=CARTESIAN_POINT('Ctrl Pts',(97.504409081684,0.545732433353623,-3.28638213037285));
#26155=CARTESIAN_POINT('Ctrl Pts',(97.5575232445258,0.43918098927892,-3.29483928527847));
#26156=CARTESIAN_POINT('Ctrl Pts',(97.5897643793363,0.347989026783004,-3.30200586241499));
#26157=CARTESIAN_POINT('Ctrl Pts',(97.6159473589241,0.229396241711363,-3.31082030717976));
#26158=CARTESIAN_POINT('Ctrl Pts',(97.6205746673701,0.204714412379462,-3.31262571697676));
#26159=CARTESIAN_POINT('Ctrl Pts',(97.6265695890689,0.165928512977467,-3.31540044245408));
#26160=CARTESIAN_POINT('Ctrl Pts',(97.6284777067806,0.151916443611184,-3.31639024236712));
#26161=CARTESIAN_POINT('Ctrl Pts',(97.6307193117883,0.132899634094702,-3.31771359933256));
#26162=CARTESIAN_POINT('Ctrl Pts',(97.6312737985954,0.127922805171892,-3.31805808442022));
#26163=CARTESIAN_POINT('Ctrl Pts',(97.6321008893281,0.120042825293883,-3.31860044242035));
#26164=CARTESIAN_POINT('Ctrl Pts',(97.6323944758455,0.117142010167833,-3.31879943904172));
#26165=CARTESIAN_POINT('Ctrl Pts',(97.6329584392618,0.111355286562692,-3.31919505698834));
#26166=CARTESIAN_POINT('Ctrl Pts',(97.6332289376657,0.108469444035727,-3.31939167667239));
#26167=CARTESIAN_POINT('Ctrl Pts',(97.6337653850194,0.102509589717689,-3.31979639132501));
#26168=CARTESIAN_POINT('Ctrl Pts',(97.634029914557,0.0994354552902017,-3.32000440895853));
#26169=CARTESIAN_POINT('Ctrl Pts',(97.634624539983,0.0921920951228765,-3.3204928854576));
#26170=CARTESIAN_POINT('Ctrl Pts',(97.6349445180288,0.0880220480615195,
-3.32077280977784));
#26171=CARTESIAN_POINT('Ctrl Pts',(97.6359645372441,0.0737313538625278,
-3.3217279452586));
#26172=CARTESIAN_POINT('Ctrl Pts',(97.6365560495189,0.0636030888188594,
-3.32239773610283));
#26173=CARTESIAN_POINT('Ctrl Pts',(97.6378156614166,0.0358860074512165,
-3.32421425643881));
#26174=CARTESIAN_POINT('Ctrl Pts',(97.6382205020686,0.0182874587000585,
-3.32534956677183));
#26175=CARTESIAN_POINT('Ctrl Pts',(97.6382307499679,0.00068569618098675,
-3.32647283958636));
#26176=CARTESIAN_POINT('Ctrl Pts',(97.6382307490143,0.00068733208902312,
-3.32647273518933));
#26177=CARTESIAN_POINT('Ctrl Pts',(97.6382770658552,-0.0786769969879645,
-3.33153744694585));
#26178=CARTESIAN_POINT('Ctrl Pts',(97.6303013137131,-0.157851648856124,
-3.33635344872659));
#26179=CARTESIAN_POINT('Ctrl Pts',(97.606625994462,-0.273795366228378,-3.34372958097377));
#26180=CARTESIAN_POINT('Ctrl Pts',(97.5969448075925,-0.311547596326401,
-3.34618219489677));
#26181=CARTESIAN_POINT('Ctrl Pts',(97.5805410616979,-0.364459829034245,
-3.34974490195577));
#26182=CARTESIAN_POINT('Ctrl Pts',(97.5753419607074,-0.380066451572931,
-3.35081150537214));
#26183=CARTESIAN_POINT('Ctrl Pts',(97.5654877568798,-0.407702394250402,
-3.35273215743632));
#26184=CARTESIAN_POINT('Ctrl Pts',(97.5609586217089,-0.419773937184554,
-3.35358218025397));
#26185=CARTESIAN_POINT('Ctrl Pts',(97.5537925641819,-0.437960120215368,
-3.35488083065936));
#26186=CARTESIAN_POINT('Ctrl Pts',(97.551300361422,-0.444131018076531,-3.35532467823532));
#26187=CARTESIAN_POINT('Ctrl Pts',(97.546682404585,-0.455292080922485,-3.35613342188149));
#26188=CARTESIAN_POINT('Ctrl Pts',(97.5445742090377,-0.46028934695762,-3.3564977232528));
#26189=CARTESIAN_POINT('Ctrl Pts',(97.5399524088277,-0.471036956683567,
-3.35728606074298));
#26190=CARTESIAN_POINT('Ctrl Pts',(97.5374272192485,-0.476782104852329,
-3.35771047782267));
#26191=CARTESIAN_POINT('Ctrl Pts',(97.5304372174622,-0.492346418079202,
-3.35886863859466));
#26192=CARTESIAN_POINT('Ctrl Pts',(97.5258833229054,-0.502124665865675,
-3.35960537554341));
#26193=CARTESIAN_POINT('Ctrl Pts',(97.5004951274383,-0.554738189931191,
-3.3636203822063));
#26194=CARTESIAN_POINT('Ctrl Pts',(97.4772136943327,-0.596336660290867,
-3.36698186067454));
#26195=CARTESIAN_POINT('Ctrl Pts',(97.4069844483931,-0.705696171288772,
-3.37633821556428));
#26196=CARTESIAN_POINT('Ctrl Pts',(97.3553484068043,-0.770121171285593,
-3.3824550675494));
#26197=CARTESIAN_POINT('Ctrl Pts',(97.2810301096322,-0.845184429744388,
-3.39011039238728));
#26198=CARTESIAN_POINT('Ctrl Pts',(97.2641530093495,-0.861248512835887,
-3.39178336260563));
#26199=CARTESIAN_POINT('Ctrl Pts',(97.239610992501,-0.883258136035274,-3.39411358256002));
#26200=CARTESIAN_POINT('Ctrl Pts',(97.2323329381092,-0.889625247004127,
-3.39479245762194));
#26201=CARTESIAN_POINT('Ctrl Pts',(97.2209760490338,-0.899316368382955,
-3.3958321568395));
#26202=CARTESIAN_POINT('Ctrl Pts',(97.2169521487075,-0.902703746584086,
-3.39619681288014));
#26203=CARTESIAN_POINT('Ctrl Pts',(97.2095173989548,-0.908877800736754,
-3.39686355685727));
#26204=CARTESIAN_POINT('Ctrl Pts',(97.2061133722229,-0.911672502063806,
-3.3971661672936));
#26205=CARTESIAN_POINT('Ctrl Pts',(97.2002682834563,-0.916416674323551,
-3.3976811399251));
#26206=CARTESIAN_POINT('Ctrl Pts',(97.1978350218529,-0.918375627463482,
-3.39789415855569));
#26207=CARTESIAN_POINT('Ctrl Pts',(97.193171651942,-0.922099498401751,-3.39829977418749));
#26208=CARTESIAN_POINT('Ctrl Pts',(97.1909429006942,-0.923866055601311,
-3.3984924898816));
#26209=CARTESIAN_POINT('Ctrl Pts',(97.1856536255042,-0.928027345319967,
-3.39894721421844));
#26210=CARTESIAN_POINT('Ctrl Pts',(97.1825875814772,-0.930415056198753,
-3.39920873700817));
#26211=CARTESIAN_POINT('Ctrl Pts',(97.1717394396161,-0.938777223758773,
-3.40012700831896));
#26212=CARTESIAN_POINT('Ctrl Pts',(97.1638943071926,-0.944669772577159,
-3.40077840549285));
#26213=CARTESIAN_POINT('Ctrl Pts',(97.0986505312648,-0.992411444864561,
-3.40610068574788));
#26214=CARTESIAN_POINT('Ctrl Pts',(97.0376390741064,-1.02909290466519,-3.41048425996234));
#26215=CARTESIAN_POINT('Ctrl Pts',(96.9206428502157,-1.08573435739123,-3.41852464525718));
#26216=CARTESIAN_POINT('Ctrl Pts',(96.8657508961875,-1.10739499830961,-3.42216643877416));
#26217=CARTESIAN_POINT('Ctrl Pts',(96.7891920199696,-1.13114760442962,-3.42727555534493));
#26218=CARTESIAN_POINT('Ctrl Pts',(96.7687478935929,-1.136889300453,-3.42864205328648));
#26219=CARTESIAN_POINT('Ctrl Pts',(96.7329170324958,-1.14591481097142,-3.43104902526543));
#26220=CARTESIAN_POINT('Ctrl Pts',(96.7175987105506,-1.14944882113353,-3.43208178182147));
#26221=CARTESIAN_POINT('Ctrl Pts',(96.695170325036,-1.15415240193836,-3.43360147526847));
#26222=CARTESIAN_POINT('Ctrl Pts',(96.6881125754422,-1.15556510371089,-3.43408077142885));
#26223=CARTESIAN_POINT('Ctrl Pts',(96.6756586733308,-1.15793939747957,-3.43492862538003));
#26224=CARTESIAN_POINT('Ctrl Pts',(96.6702678776649,-1.15892818764057,-3.43529631771252));
#26225=CARTESIAN_POINT('Ctrl Pts',(96.6590083321617,-1.16091230177867,-3.43606583260128));
#26226=CARTESIAN_POINT('Ctrl Pts',(96.6531385585539,-1.16190082946785,-3.43646785681354));
#26227=CARTESIAN_POINT('Ctrl Pts',(96.6377935259728,-1.16436560868705,-3.43752122804168));
#26228=CARTESIAN_POINT('Ctrl Pts',(96.6283074470817,-1.16577067974211,-3.43817477381897));
#26229=CARTESIAN_POINT('Ctrl Pts',(96.5881153794085,-1.17122317816419,-3.44095448130407));
#26230=CARTESIAN_POINT('Ctrl Pts',(96.5572756728521,-1.17417407394072,-3.44311408813969));
#26231=CARTESIAN_POINT('Ctrl Pts',(96.4434276068684,-1.18055209797416,-3.45118957647388));
#26232=CARTESIAN_POINT('Ctrl Pts',(96.3602467950593,-1.1764114227093,-3.45731174126188));
#26233=CARTESIAN_POINT('Ctrl Pts',(96.226687130472,-1.15548905986495,-3.46720774948426));
#26234=CARTESIAN_POINT('Ctrl Pts',(96.1757534784659,-1.14400440733427,-3.47099110822223));
#26235=CARTESIAN_POINT('Ctrl Pts',(96.1190730342821,-1.12720189264742,-3.47510294566811));
#26236=CARTESIAN_POINT('Ctrl Pts',(96.112419768381,-1.12516527293042,-3.47558398547491));
#26237=CARTESIAN_POINT('Ctrl Pts',(96.1022933105377,-1.12196706002121,-3.47631326501021));
#26238=CARTESIAN_POINT('Ctrl Pts',(96.0988069783108,-1.12084807532427,-3.47656381759944));
#26239=CARTESIAN_POINT('Ctrl Pts',(96.0924336865831,-1.11876964964784,-3.47702081619737));
#26240=CARTESIAN_POINT('Ctrl Pts',(96.0895452148008,-1.117815278963,-3.47722753810698));
#26241=CARTESIAN_POINT('Ctrl Pts',(96.083032130833,-1.11563528565298,-3.47769278803118));
#26242=CARTESIAN_POINT('Ctrl Pts',(96.0794097718269,-1.11440318551529,-3.47795093777042));
#26243=CARTESIAN_POINT('Ctrl Pts',(96.0700619978902,-1.11117274847258,-3.47861569915611));
#26244=CARTESIAN_POINT('Ctrl Pts',(96.0643458118303,-1.10914777700991,-3.47902082631766));
#26245=CARTESIAN_POINT('Ctrl Pts',(96.0260545216806,-1.09524921430965,-3.48172702739036));
#26246=CARTESIAN_POINT('Ctrl Pts',(95.9939983918163,-1.08198507025018,-3.4839554384391));
#26247=CARTESIAN_POINT('Ctrl Pts',(95.9369542069627,-1.05537379973302,-3.48793273566414));
#26248=CARTESIAN_POINT('Ctrl Pts',(95.9117747074287,-1.04250452690599,-3.48969277121955));
#26249=CARTESIAN_POINT('Ctrl Pts',(95.8450410465118,-1.00530856258729,-3.49442958033675));
#26250=CARTESIAN_POINT('Ctrl Pts',(95.8044769525897,-0.979321316211375,
-3.49738935153617));
#26251=CARTESIAN_POINT('Ctrl Pts',(95.7227357275263,-0.919591048871131,
-3.50372128862714));
#26252=CARTESIAN_POINT('Ctrl Pts',(95.6820281079373,-0.885395849201364,
-3.5070980240436));
#26253=CARTESIAN_POINT('Ctrl Pts',(95.6359725484629,-0.841069596787787,
-3.51129927786758));
#26254=CARTESIAN_POINT('Ctrl Pts',(95.6282795382827,-0.833458438344985,
-3.51201487009788));
#26255=CARTESIAN_POINT('Ctrl Pts',(95.6163313781962,-0.821307042810172,
-3.51314902557432));
#26256=CARTESIAN_POINT('Ctrl Pts',(95.6120053329248,-0.816837121386389,
-3.51356450698912));
#26257=CARTESIAN_POINT('Ctrl Pts',(95.603970740741,-0.808402618418435,-3.51434543318382));
#26258=CARTESIAN_POINT('Ctrl Pts',(95.6002537870404,-0.804446243356598,
-3.5147105052207));
#26259=CARTESIAN_POINT('Ctrl Pts',(95.5919913610126,-0.79552886101755,-3.51553068990995));
#26260=CARTESIAN_POINT('Ctrl Pts',(95.587460814149,-0.790554346041938,-3.51598641207894));
#26261=CARTESIAN_POINT('Ctrl Pts',(95.5760368381114,-0.777792921079663,
-3.51715109092701));
#26262=CARTESIAN_POINT('Ctrl Pts',(95.5692035893285,-0.769953160572135,
-3.51786248522407));
#26263=CARTESIAN_POINT('Ctrl Pts',(95.5139475611787,-0.704836813987481,
-3.52373941571972));
#26264=CARTESIAN_POINT('Ctrl Pts',(95.4710025016443,-0.64315548341963,-3.52912368160108));
#26265=CARTESIAN_POINT('Ctrl Pts',(95.4063689084888,-0.528360586635435,
-3.53875927167759));
#26266=CARTESIAN_POINT('Ctrl Pts',(95.3821320477432,-0.476949636307013,
-3.5429510902622));
#26267=CARTESIAN_POINT('Ctrl Pts',(95.3539815457502,-0.403996798857289,
-3.54860495379084));
#26268=CARTESIAN_POINT('Ctrl Pts',(95.3468131063683,-0.383794724334684,
-3.55014046823892));
#26269=CARTESIAN_POINT('Ctrl Pts',(95.3360414552827,-0.350588771039507,
-3.55260440821723));
#26270=CARTESIAN_POINT('Ctrl Pts',(95.3321034046053,-0.337699300320329,
-3.55354638854198));
#26271=CARTESIAN_POINT('Ctrl Pts',(95.3270748461233,-0.320169208460801,
-3.55480552949018));
#26272=CARTESIAN_POINT('Ctrl Pts',(95.3257901546734,-0.315585993521177,
-3.55513271309447));
#26273=CARTESIAN_POINT('Ctrl Pts',(95.3236924921297,-0.307924022149816,
-3.55567617806474));
#26274=CARTESIAN_POINT('Ctrl Pts',(95.3228641695256,-0.304849574181654,
-3.55589331153192));
#26275=CARTESIAN_POINT('Ctrl Pts',(95.3213188598415,-0.299019899975307,
-3.55630321057245));
#26276=CARTESIAN_POINT('Ctrl Pts',(95.3205993795728,-0.29626537778691,-3.55649612091172));
#26277=CARTESIAN_POINT('Ctrl Pts',(95.3189184526351,-0.289733192291764,
-3.55695183998417));
#26278=CARTESIAN_POINT('Ctrl Pts',(95.3179657510791,-0.285953281871582,
-3.55721415769265));
#26279=CARTESIAN_POINT('Ctrl Pts',(95.3146828833548,-0.272649917649177,
-3.55813273414725));
#26280=CARTESIAN_POINT('Ctrl Pts',(95.3124528061022,-0.263101849663352,
-3.55878365847946));
#26281=CARTESIAN_POINT('Ctrl Pts',(95.2951838363263,-0.184760141228891,
-3.56406467365795));
#26282=CARTESIAN_POINT('Ctrl Pts',(95.2862212028043,-0.114762692647277,
-3.56841258552827));
#26283=CARTESIAN_POINT('Ctrl Pts',(95.2813306304502,0.0149428872917502,
-3.57644150355668));
#26284=CARTESIAN_POINT('Ctrl Pts',(95.2835818817306,0.0743417140062381,
-3.58010846610203));
#26285=CARTESIAN_POINT('Ctrl Pts',(95.2927138946204,0.154498224522783,-3.58524970427908));
#26286=CARTESIAN_POINT('Ctrl Pts',(95.29570180392,0.175610524798074,-3.58662166019366));
#26287=CARTESIAN_POINT('Ctrl Pts',(95.3018936552606,0.212177330451747,-3.58903737412449));
#26288=CARTESIAN_POINT('Ctrl Pts',(95.3048383146312,0.22767037617934,-3.59007333527359));
#26289=CARTESIAN_POINT('Ctrl Pts',(95.3095805711071,0.250150591116389,-3.59159687691451));
#26290=CARTESIAN_POINT('Ctrl Pts',(95.3111327728463,0.257188188268535,-3.59207676071437));
#26291=CARTESIAN_POINT('Ctrl Pts',(95.3139792477609,0.269553265249039,-3.59292528637033));
#26292=CARTESIAN_POINT('Ctrl Pts',(95.3152463260638,0.274886832075314,-3.59329305823462));
#26293=CARTESIAN_POINT('Ctrl Pts',(95.3179658266052,0.285988880647027,-3.59406237518671));
#26294=CARTESIAN_POINT('Ctrl Pts',(95.3194248049891,0.29175558046656,-3.59446411949715));
#26295=CARTESIAN_POINT('Ctrl Pts',(95.3233450973738,0.306771444794223,-3.59551594036567));
#26296=CARTESIAN_POINT('Ctrl Pts',(95.3258755418078,0.316001938273036,-3.59616820373848));
#26297=CARTESIAN_POINT('Ctrl Pts',(95.3370214427277,0.354798778111042,-3.59893449446566));
#26298=CARTESIAN_POINT('Ctrl Pts',(95.3466816220361,0.384049727401228,-3.60108156331856));
#26299=CARTESIAN_POINT('Ctrl Pts',(95.3866479761879,0.490817801548664,-3.60915376741557));
#26300=CARTESIAN_POINT('Ctrl Pts',(95.4239942613389,0.565430217690965,-3.61528688016901));
#26301=CARTESIAN_POINT('Ctrl Pts',(95.4970510205316,0.679428746232457,-3.62519851346871));
#26302=CARTESIAN_POINT('Ctrl Pts',(95.5281152794503,0.721468092900924,-3.62898630661707));
#26303=CARTESIAN_POINT('Ctrl Pts',(95.5663688436828,0.766620524406078,-3.63310231939359));
#26304=CARTESIAN_POINT('Ctrl Pts',(95.5709141479166,0.771890146059535,-3.63358343452079));
#26305=CARTESIAN_POINT('Ctrl Pts',(95.5779221076076,0.779870733286376,-3.63431280417285));
#26306=CARTESIAN_POINT('Ctrl Pts',(95.5803510473422,0.782610903504199,-3.63456337241033));
#26307=CARTESIAN_POINT('Ctrl Pts',(95.5848212635766,0.787606774359508,-3.63502038600803));
#26308=CARTESIAN_POINT('Ctrl Pts',(95.5868585072208,0.789865903405021,-3.63522710739106));
#26309=CARTESIAN_POINT('Ctrl Pts',(95.591477679009,0.794948435498007,-3.63569233929621));
#26310=CARTESIAN_POINT('Ctrl Pts',(95.5940646260103,0.797767168194389,-3.635950471679));
#26311=CARTESIAN_POINT('Ctrl Pts',(95.6007867201475,0.805020283055485,-3.63661515804458));
#26312=CARTESIAN_POINT('Ctrl Pts',(95.6049425181058,0.809435494859631,-3.63702022809975));
#26313=CARTESIAN_POINT('Ctrl Pts',(95.6330751039406,0.838865444032705,-3.63972494587747));
#26314=CARTESIAN_POINT('Ctrl Pts',(95.6581141449915,0.862846268399949,-3.64195202212529));
#26315=CARTESIAN_POINT('Ctrl Pts',(95.7053846884277,0.904278720673471,-3.64592386524868));
#26316=CARTESIAN_POINT('Ctrl Pts',(95.727254140592,0.922100285014337,-3.64767986637031));
#26317=CARTESIAN_POINT('Ctrl Pts',(95.7879764152464,0.968055663958696,-3.65240143967931));
#26318=CARTESIAN_POINT('Ctrl Pts',(95.8279404400586,0.994628839711344,-3.65535005607151));
#26319=CARTESIAN_POINT('Ctrl Pts',(95.8866360330971,1.02868537170764,-3.65959362283606));
#26320=CARTESIAN_POINT('Ctrl Pts',(95.9041048308538,1.03823730619562,-3.66084605093489));
#26321=CARTESIAN_POINT('Ctrl Pts',(95.9218017102038,1.04733936217842,-3.66210953954391));
#26322=CARTESIAN_POINT('Origin',(96.460480949577,-7.19464945638997E-16,
0.924367114736168));
#26323=CARTESIAN_POINT('',(95.9218016729659,1.04733934302581,-4.26051510683823));
#26324=CARTESIAN_POINT('',(95.9218017335164,1.04733937416884,-4.16230107423304));
#26325=CARTESIAN_POINT('',(95.9218016730721,1.04733934308042,0.924367114736168));
#26326=CARTESIAN_POINT('',(97.6382304695238,-0.00104852062301618,-3.92438110998958));
#26327=CARTESIAN_POINT('Ctrl Pts',(95.9218016729659,1.04733934302581,-4.26051510683823));
#26328=CARTESIAN_POINT('Ctrl Pts',(95.9188215355377,1.04580656543591,-4.26028177707212));
#26329=CARTESIAN_POINT('Ctrl Pts',(95.9158478598941,1.04426102683307,-4.26004910401954));
#26330=CARTESIAN_POINT('Ctrl Pts',(95.9080700984155,1.04017634993692,-4.25944101180714));
#26331=CARTESIAN_POINT('Ctrl Pts',(95.9032768919896,1.037616609602,-4.25906673765364));
#26332=CARTESIAN_POINT('Ctrl Pts',(95.8955739714834,1.03343420948893,-4.25846623425049));
#26333=CARTESIAN_POINT('Ctrl Pts',(95.8926531955007,1.03183225460391,-4.25823876447539));
#26334=CARTESIAN_POINT('Ctrl Pts',(95.8870124124072,1.02870725518024,-4.25779995986589));
#26335=CARTESIAN_POINT('Ctrl Pts',(95.8842916159851,1.02718578265178,-4.2575885377243));
#26336=CARTESIAN_POINT('Ctrl Pts',(95.8777283936761,1.02348133845189,-4.25707902852195));
#26337=CARTESIAN_POINT('Ctrl Pts',(95.8738921009329,1.02128747949717,-4.25678162146082));
#26338=CARTESIAN_POINT('Ctrl Pts',(95.8604422314703,1.01349512083887,-4.25574003595753));
#26339=CARTESIAN_POINT('Ctrl Pts',(95.8508953607436,1.00778184901058,-4.25500271280772));
#26340=CARTESIAN_POINT('Ctrl Pts',(95.8274118415054,0.993272424760727,-4.25319035488317));
#26341=CARTESIAN_POINT('Ctrl Pts',(95.8135758092324,0.984317225977614,-4.25212371861783));
#26342=CARTESIAN_POINT('Ctrl Pts',(95.7544233807811,0.944245299800212,-4.24754799908496));
#26343=CARTESIAN_POINT('Ctrl Pts',(95.7111257036779,0.910265957092341,-4.24415579942139));
#26344=CARTESIAN_POINT('Ctrl Pts',(95.6121084665285,0.820688116726456,-4.23589674640043));
#26345=CARTESIAN_POINT('Ctrl Pts',(95.5592843367647,0.762304109621516,-4.23103137637637));
#26346=CARTESIAN_POINT('Ctrl Pts',(95.503472015115,0.686635918194949,-4.22490415859336));
#26347=CARTESIAN_POINT('Ctrl Pts',(95.4945248122245,0.673990867318193,-4.22388625902733));
#26348=CARTESIAN_POINT('Ctrl Pts',(95.4818557318674,0.655315085264326,-4.2223894992221));
#26349=CARTESIAN_POINT('Ctrl Pts',(95.4779345315283,0.649421057891322,-4.22191806447771));
#26350=CARTESIAN_POINT('Ctrl Pts',(95.4710717917935,0.638901110122984,-4.22107808566589));
#26351=CARTESIAN_POINT('Ctrl Pts',(95.4681089404117,0.634289290242098,-4.22071034006781));
#26352=CARTESIAN_POINT('Ctrl Pts',(95.4619963827024,0.624627134709062,-4.2199408091851));
#26353=CARTESIAN_POINT('Ctrl Pts',(95.4588525578356,0.619573280829297,-4.21953882284913));
#26354=CARTESIAN_POINT('Ctrl Pts',(95.4507459676092,0.606318571260493,-4.21848576426071));
#26355=CARTESIAN_POINT('Ctrl Pts',(95.445844860502,0.598080714446914,-4.21783249599246));
#26356=CARTESIAN_POINT('Ctrl Pts',(95.4238603149811,0.56008064903702,-4.21482384246334));
#26357=CARTESIAN_POINT('Ctrl Pts',(95.4079837456875,0.529643177178622,-4.21242654021555));
#26358=CARTESIAN_POINT('Ctrl Pts',(95.3651696292797,0.438011884448065,-4.20524130982053));
#26359=CARTESIAN_POINT('Ctrl Pts',(95.3420871710673,0.375173065989842,-4.20034631197919));
#26360=CARTESIAN_POINT('Ctrl Pts',(95.3086347324428,0.252869407464614,-4.19104137635901));
#26361=CARTESIAN_POINT('Ctrl Pts',(95.2972514231438,0.193884379330255,-4.18664885652213));
#26362=CARTESIAN_POINT('Ctrl Pts',(95.2892665473949,0.124308871235898,-4.18173764880226));
#26363=CARTESIAN_POINT('Ctrl Pts',(95.2882493267785,0.114319335857526,-4.18103904539758));
#26364=CARTESIAN_POINT('Ctrl Pts',(95.2870107407519,0.100390610904378,-4.18007514959461));
#26365=CARTESIAN_POINT('Ctrl Pts',(95.2866812539225,0.0964618129432036,
-4.17980439568779));
#26366=CARTESIAN_POINT('Ctrl Pts',(95.2861469340296,0.0896819492625977,
-4.17933918684036));
#26367=CARTESIAN_POINT('Ctrl Pts',(95.2859327425362,0.0868316870583113,
-4.17914422981957));
#26368=CARTESIAN_POINT('Ctrl Pts',(95.2855027979959,0.0808174646131285,
-4.17873420021916));
#26369=CARTESIAN_POINT('Ctrl Pts',(95.2852894438399,0.0776533615249369,
-4.17851926750525));
#26370=CARTESIAN_POINT('Ctrl Pts',(95.2847917942317,0.0698006836629429,
-4.17798771022529));
#26371=CARTESIAN_POINT('Ctrl Pts',(95.2845227583069,0.0651111333339425,
-4.17767191548024));
#26372=CARTESIAN_POINT('Ctrl Pts',(95.2836141369934,0.0474229567656407,
-4.17648657481495));
#26373=CARTESIAN_POINT('Ctrl Pts',(95.2831619322355,0.0344150738771813,
-4.17562664249958));
#26374=CARTESIAN_POINT('Ctrl Pts',(95.2825544460545,0.000990245263173205,
-4.1734410560954));
#26375=CARTESIAN_POINT('Ctrl Pts',(95.2827142263405,-0.019428654245409,
-4.17212893859638));
#26376=CARTESIAN_POINT('Ctrl Pts',(95.2853629410118,-0.0976964847208325,
-4.16715319170785));
#26377=CARTESIAN_POINT('Ctrl Pts',(95.2915850881283,-0.15533901963567,-4.16359823879228));
#26378=CARTESIAN_POINT('Ctrl Pts',(95.3156314500694,-0.286557312319542,
-4.1553380793406));
#26379=CARTESIAN_POINT('Ctrl Pts',(95.3363480036909,-0.359330461262717,
-4.15062288797782));
#26380=CARTESIAN_POINT('Ctrl Pts',(95.367673455852,-0.439288951056962,-4.14498682695457));
#26381=CARTESIAN_POINT('Ctrl Pts',(95.3715909734151,-0.448911583144755,
-4.14430099649661));
#26382=CARTESIAN_POINT('Ctrl Pts',(95.3782533655663,-0.464675965387144,
-4.1431642558651));
#26383=CARTESIAN_POINT('Ctrl Pts',(95.3809245207711,-0.47084839415314,-4.14271580523754));
#26384=CARTESIAN_POINT('Ctrl Pts',(95.3858470347871,-0.481961080404928,
-4.14190215135114));
#26385=CARTESIAN_POINT('Ctrl Pts',(95.3880799799546,-0.486909326783869,
-4.14153757771319));
#26386=CARTESIAN_POINT('Ctrl Pts',(95.3929460450998,-0.497496756433642,
-4.14075254539853));
#26387=CARTESIAN_POINT('Ctrl Pts',(95.3955898041255,-0.503130838562036,
-4.14033173339041));
#26388=CARTESIAN_POINT('Ctrl Pts',(95.4029579410932,-0.518514729960688,
-4.13917414239387));
#26389=CARTESIAN_POINT('Ctrl Pts',(95.4077722944733,-0.528220515062181,
-4.13843430395658));
#26390=CARTESIAN_POINT('Ctrl Pts',(95.4370906488992,-0.585333399808519,
-4.13402279789795));
#26391=CARTESIAN_POINT('Ctrl Pts',(95.4646564533333,-0.631090322572359,
-4.13024508643766));
#26392=CARTESIAN_POINT('Ctrl Pts',(95.5226971689602,-0.714111703771539,
-4.12292352043515));
#26393=CARTESIAN_POINT('Ctrl Pts',(95.5525419545015,-0.751691620923437,
-4.11940223740577));
#26394=CARTESIAN_POINT('Ctrl Pts',(95.6034423108333,-0.808316094063832,
-4.11381600843628));
#26395=CARTESIAN_POINT('Ctrl Pts',(95.6230400956137,-0.82860306926117,-4.11175087348832));
#26396=CARTESIAN_POINT('Ctrl Pts',(95.6683026593464,-0.872209483707722,
-4.10719394997566));
#26397=CARTESIAN_POINT('Ctrl Pts',(95.6943092548852,-0.895140914568747,
-4.10471464788955));
#26398=CARTESIAN_POINT('Ctrl Pts',(95.7260124771976,-0.920699675540471,
-4.10188418026188));
#26399=CARTESIAN_POINT('Ctrl Pts',(95.7307624967136,-0.9244689355949,-4.10146492921322));
#26400=CARTESIAN_POINT('Ctrl Pts',(95.7385569562706,-0.930556526798279,
-4.10078508394169));
#26401=CARTESIAN_POINT('Ctrl Pts',(95.7415838861753,-0.932896947658568,
-4.10052303971565));
#26402=CARTESIAN_POINT('Ctrl Pts',(95.7470380538224,-0.937071796988144,
-4.10005446953611));
#26403=CARTESIAN_POINT('Ctrl Pts',(95.7494610351639,-0.938911604018742,
-4.09984757977509));
#26404=CARTESIAN_POINT('Ctrl Pts',(95.7548163014806,-0.942945320473388,
-4.09939310367173));
#26405=CARTESIAN_POINT('Ctrl Pts',(95.7577517033606,-0.945134953538001,
-4.09914580903525));
#26406=CARTESIAN_POINT('Ctrl Pts',(95.7662952303945,-0.951446102682716,
-4.09843115797298));
#26407=CARTESIAN_POINT('Ctrl Pts',(95.7719298517088,-0.955531731775664,
-4.09796616436047));
#26408=CARTESIAN_POINT('Ctrl Pts',(95.8201568581022,-0.989852699961186,
-4.0940366646929));
#26409=CARTESIAN_POINT('Ctrl Pts',(95.8646867980555,-1.0172777919514,-4.09073887976694));
#26410=CARTESIAN_POINT('Ctrl Pts',(95.9845471750855,-1.08051680214726,-4.08229739415115));
#26411=CARTESIAN_POINT('Ctrl Pts',(96.0621077855663,-1.11145307757198,-4.07722999925039));
#26412=CARTESIAN_POINT('Ctrl Pts',(96.1718551393677,-1.14224937672569,-4.06995889791469));
#26413=CARTESIAN_POINT('Ctrl Pts',(96.201739316398,-1.14938723252431,-4.06797165734062));
#26414=CARTESIAN_POINT('Ctrl Pts',(96.2412475420255,-1.15720491997214,-4.06531739560646));
#26415=CARTESIAN_POINT('Ctrl Pts',(96.2506506911962,-1.15894683553549,-4.064683725411));
#26416=CARTESIAN_POINT('Ctrl Pts',(96.2659340770745,-1.16158596063495,-4.0636501710267));
#26417=CARTESIAN_POINT('Ctrl Pts',(96.271801854891,-1.16255349407184,-4.0632524962546));
#26418=CARTESIAN_POINT('Ctrl Pts',(96.2830932902497,-1.16432759370111,-4.06248547878851));
#26419=CARTESIAN_POINT('Ctrl Pts',(96.2885157586713,-1.16514080630106,-4.06211635458374));
#26420=CARTESIAN_POINT('Ctrl Pts',(96.3010828405792,-1.16693586523239,-4.06125897403396));
#26421=CARTESIAN_POINT('Ctrl Pts',(96.308231125564,-1.16789000244121,-4.06076986800623));
#26422=CARTESIAN_POINT('Ctrl Pts',(96.3310620567884,-1.17072425788644,-4.05920294031248));
#26423=CARTESIAN_POINT('Ctrl Pts',(96.3467733872825,-1.17235450532021,-4.05811745166285));
#26424=CARTESIAN_POINT('Ctrl Pts',(96.3838021849195,-1.1754453857943,-4.05554104002007));
#26425=CARTESIAN_POINT('Ctrl Pts',(96.4051354426366,-1.17664279392305,-4.05404259029126));
#26426=CARTESIAN_POINT('Ctrl Pts',(96.4860425467768,-1.17897893349908,-4.04830591819803));
#26427=CARTESIAN_POINT('Ctrl Pts',(96.5456351264127,-1.17617687917045,-4.04396450259567));
#26428=CARTESIAN_POINT('Ctrl Pts',(96.6743251813363,-1.16029292362267,-4.03445186984287));
#26429=CARTESIAN_POINT('Ctrl Pts',(96.7429975345149,-1.14551088136044,-4.02928668292465));
#26430=CARTESIAN_POINT('Ctrl Pts',(96.8193217277633,-1.12179526804257,-4.02368470184939));
#26431=CARTESIAN_POINT('Ctrl Pts',(96.8286549516762,-1.11876684224169,-4.02300228900284));
#26432=CARTESIAN_POINT('Ctrl Pts',(96.8416479119142,-1.11437069799516,-4.02205699039771));
#26433=CARTESIAN_POINT('Ctrl Pts',(96.8453400355421,-1.11310097958984,-4.02178890610049));
#26434=CARTESIAN_POINT('Ctrl Pts',(96.8517149674126,-1.11087313422676,-4.02132703220032));
#26435=CARTESIAN_POINT('Ctrl Pts',(96.8544007110296,-1.10992360054031,-4.02113275675411));
#26436=CARTESIAN_POINT('Ctrl Pts',(96.8600796601408,-1.1078926217854,-4.02072266368408));
#26437=CARTESIAN_POINT('Ctrl Pts',(96.8630719802415,-1.10680877002707,-4.02050699389728));
#26438=CARTESIAN_POINT('Ctrl Pts',(96.8702961370049,-1.10415892641754,-4.01998723567396));
#26439=CARTESIAN_POINT('Ctrl Pts',(96.8745234882347,-1.10258070020744,-4.01968385423754));
#26440=CARTESIAN_POINT('Ctrl Pts',(96.8902420487293,-1.09660923066956,-4.01855827583403));
#26441=CARTESIAN_POINT('Ctrl Pts',(96.9016737482242,-1.0920601407146,-4.01774463809231));
#26442=CARTESIAN_POINT('Ctrl Pts',(96.9306303894835,-1.08000828382375,-4.01569128438336));
#26443=CARTESIAN_POINT('Ctrl Pts',(96.9480487847208,-1.07225746806751,-4.01446331133274));
#26444=CARTESIAN_POINT('Ctrl Pts',(97.0191164037625,-1.03854375300482,-4.00945272827282));
#26445=CARTESIAN_POINT('Ctrl Pts',(97.0709476135287,-1.00894900412825,-4.00579388535072));
#26446=CARTESIAN_POINT('Ctrl Pts',(97.1832585635141,-0.932985160593492,
-3.99739924829797));
#26447=CARTESIAN_POINT('Ctrl Pts',(97.2419224049484,-0.884429652000915,
-3.99265566083505));
#26448=CARTESIAN_POINT('Ctrl Pts',(97.3028258754823,-0.82319989374108,-3.98698773984564));
#26449=CARTESIAN_POINT('Ctrl Pts',(97.3100558781428,-0.815736151464084,
-3.98630178955589));
#26450=CARTESIAN_POINT('Ctrl Pts',(97.321801527665,-0.803285233095336,-3.9851648912569));
#26451=CARTESIAN_POINT('Ctrl Pts',(97.3263749828294,-0.798353195004882,
-3.98471640399275));
#26452=CARTESIAN_POINT('Ctrl Pts',(97.3345629269142,-0.789370148393381,
-3.98390271096816));
#26453=CARTESIAN_POINT('Ctrl Pts',(97.3381921531583,-0.785332780229276,
-3.98353813510746));
#26454=CARTESIAN_POINT('Ctrl Pts',(97.3459214540308,-0.776613741159297,
-3.98275312846434));
#26455=CARTESIAN_POINT('Ctrl Pts',(97.3500125786478,-0.771924392801422,
-3.98233234456633));
#26456=CARTESIAN_POINT('Ctrl Pts',(97.3605333015955,-0.759670576410502,
-3.98123629301274));
#26457=CARTESIAN_POINT('Ctrl Pts',(97.3669046470154,-0.752056973437907,
-3.98055870029925));
#26458=CARTESIAN_POINT('Ctrl Pts',(97.4010022670002,-0.710248358526442,
-3.97685525506667));
#26459=CARTESIAN_POINT('Ctrl Pts',(97.4268876166717,-0.674603870452686,
-3.97375827903032));
#26460=CARTESIAN_POINT('Ctrl Pts',(97.4820555408387,-0.588924269737015,
-3.96644873121523));
#26461=CARTESIAN_POINT('Ctrl Pts',(97.5097624452733,-0.538009126532806,
-3.96219973802592));
#26462=CARTESIAN_POINT('Ctrl Pts',(97.5452613737911,-0.459506128264437,
-3.9558783586982));
#26463=CARTESIAN_POINT('Ctrl Pts',(97.5559797741646,-0.433332285159325,
-3.95380738604897));
#26464=CARTESIAN_POINT('Ctrl Pts',(97.5777892088457,-0.374076231851213,
-3.94922854590822));
#26465=CARTESIAN_POINT('Ctrl Pts',(97.5883746661407,-0.340832863835478,
-3.94673338499372));
#26466=CARTESIAN_POINT('Ctrl Pts',(97.5990537983305,-0.301303505351245,
-3.94388728888438));
#26467=CARTESIAN_POINT('Ctrl Pts',(97.6005921574859,-0.295429131504577,
-3.94346743145868));
#26468=CARTESIAN_POINT('Ctrl Pts',(97.6030263232253,-0.285831752565939,
-3.94278680345621));
#26469=CARTESIAN_POINT('Ctrl Pts',(97.6039495065895,-0.282115901335005,
-3.94252457748723));
#26470=CARTESIAN_POINT('Ctrl Pts',(97.6055737362804,-0.275439337649384,
-3.9420558172051));
#26471=CARTESIAN_POINT('Ctrl Pts',(97.6062814441235,-0.272480359337039,
-3.94184891771273));
#26472=CARTESIAN_POINT('Ctrl Pts',(97.6078152215821,-0.265955870366845,
-3.94139458012618));
#26473=CARTESIAN_POINT('Ctrl Pts',(97.6086361425133,-0.262389234808589,
-3.94114743254129));
#26474=CARTESIAN_POINT('Ctrl Pts',(97.610305694187,-0.254977688742141,-3.94063626921036));
#26475=CARTESIAN_POINT('Ctrl Pts',(97.6111516979197,-0.251132226233793,
-3.9403723982116));
#26476=CARTESIAN_POINT('Ctrl Pts',(97.6133021511285,-0.241118411474756,
-3.93968858455184));
#26477=CARTESIAN_POINT('Ctrl Pts',(97.6145764032244,-0.234943608189631,
-3.93927019642514));
#26478=CARTESIAN_POINT('Ctrl Pts',(97.6306488144902,-0.153771707192968,
-3.93380950112707));
#26479=CARTESIAN_POINT('Ctrl Pts',(97.6381624101106,-0.0775084268869562,
-3.92911084375618));
#26480=CARTESIAN_POINT('Ctrl Pts',(97.6382304828084,-0.00104855774486002,
-3.92438113289323));
#26481=CARTESIAN_POINT('Ctrl Pts',(97.6382304828425,-0.00104851936493903,
-3.92438113051909));
#26482=CARTESIAN_POINT('Ctrl Pts',(97.6383002269576,0.0772915683713354,
-3.91953511170716));
#26483=CARTESIAN_POINT('Ctrl Pts',(97.6305539237946,0.155436028635755,-3.91467389969789));
#26484=CARTESIAN_POINT('Ctrl Pts',(97.6131372675276,0.242029690541228,-3.90890634965245));
#26485=CARTESIAN_POINT('Ctrl Pts',(97.6110418725032,0.251802524473686,-3.90825012618013));
#26486=CARTESIAN_POINT('Ctrl Pts',(97.6073712668865,0.267918573086483,-3.90715853485289));
#26487=CARTESIAN_POINT('Ctrl Pts',(97.6058671594109,0.274277576975191,-3.90672537462082));
#26488=CARTESIAN_POINT('Ctrl Pts',(97.6028218544812,0.28669031982019,-3.90587487533533));
#26489=CARTESIAN_POINT('Ctrl Pts',(97.6012852545469,0.292744970449118,-3.9054576932432));
#26490=CARTESIAN_POINT('Ctrl Pts',(97.5983238954102,0.304036085270877,-3.90467521197181));
#26491=CARTESIAN_POINT('Ctrl Pts',(97.5969109617455,0.30927550223791,-3.90431029913378));
#26492=CARTESIAN_POINT('Ctrl Pts',(97.5936742447718,0.320956122002058,-3.9034926128811));
#26493=CARTESIAN_POINT('Ctrl Pts',(97.5918316618733,0.3273918739262,-3.90303924704889));
#26494=CARTESIAN_POINT('Ctrl Pts',(97.5870188501328,0.343676056174618,-3.90188472558683));
#26495=CARTESIAN_POINT('Ctrl Pts',(97.5839743269869,0.353501757079863,-3.90118120533519));
#26496=CARTESIAN_POINT('Ctrl Pts',(97.5625332826516,0.41962277621498,-3.89639898927226));
#26497=CARTESIAN_POINT('Ctrl Pts',(97.5400445944713,0.474492345754514,-3.89218781070295));
#26498=CARTESIAN_POINT('Ctrl Pts',(97.4910687355275,0.572275608944413,-3.88424865580919));
#26499=CARTESIAN_POINT('Ctrl Pts',(97.4657669042832,0.615638191140721,-3.88055469308813));
#26500=CARTESIAN_POINT('Ctrl Pts',(97.4173021027298,0.687702537750321,-3.87419503402469));
#26501=CARTESIAN_POINT('Ctrl Pts',(97.3954115579605,0.717179626529923,-3.87152354180378));
#26502=CARTESIAN_POINT('Ctrl Pts',(97.3611212399367,0.759109498322487,-3.86766335613339));
#26503=CARTESIAN_POINT('Ctrl Pts',(97.3497633240153,0.772384035688475,-3.86643181847522));
#26504=CARTESIAN_POINT('Ctrl Pts',(97.3338899948569,0.790121393060307,-3.86477858823891));
#26505=CARTESIAN_POINT('Ctrl Pts',(97.3296282548875,0.794806984281414,-3.86434111211018));
#26506=CARTESIAN_POINT('Ctrl Pts',(97.3228819984587,0.802105034608602,-3.86365884752554));
#26507=CARTESIAN_POINT('Ctrl Pts',(97.3204230099361,0.804740771527269,-3.86341226192987));
#26508=CARTESIAN_POINT('Ctrl Pts',(97.3158635732534,0.809583170584965,-3.86295896534749));
#26509=CARTESIAN_POINT('Ctrl Pts',(97.3137666658123,0.811792972271169,-3.86275200975359));
#26510=CARTESIAN_POINT('Ctrl Pts',(97.3089673909662,0.816811491014688,-3.86228176094614));
#26511=CARTESIAN_POINT('Ctrl Pts',(97.3062596375748,0.819614949285999,-3.8620188827926));
#26512=CARTESIAN_POINT('Ctrl Pts',(97.299137653688,0.826915778886499,-3.86133363092183));
#26513=CARTESIAN_POINT('Ctrl Pts',(97.2947010883006,0.831391326112192,-3.86091289739467));
#26514=CARTESIAN_POINT('Ctrl Pts',(97.2609660255036,0.864880855351779,-3.85775756661836));
#26515=CARTESIAN_POINT('Ctrl Pts',(97.2301944185184,0.892377287020628,-3.85512602537788));
#26516=CARTESIAN_POINT('Ctrl Pts',(97.1313703769921,0.971758858477707,-3.84716879529666));
#26517=CARTESIAN_POINT('Ctrl Pts',(97.0590670773619,1.01789150203666,-3.84199035874457));
#26518=CARTESIAN_POINT('Ctrl Pts',(96.9486723009609,1.07246453983375,-3.83419594380122));
#26519=CARTESIAN_POINT('Ctrl Pts',(96.9141634461721,1.08751217833587,-3.83177690051543));
#26520=CARTESIAN_POINT('Ctrl Pts',(96.8694406830457,1.10451414676563,-3.82863012445964));
#26521=CARTESIAN_POINT('Ctrl Pts',(96.8598386509001,1.10802210250701,-3.8279539085823));
#26522=CARTESIAN_POINT('Ctrl Pts',(96.8443193132146,1.11346392284733,-3.82685941839377));
#26523=CARTESIAN_POINT('Ctrl Pts',(96.8384300791682,1.11547669174042,-3.82644372964281));
#26524=CARTESIAN_POINT('Ctrl Pts',(96.8273745084115,1.11915756270456,-3.82566258312755));
#26525=CARTESIAN_POINT('Ctrl Pts',(96.8222120338198,1.12083681001103,-3.82529749956686));
#26526=CARTESIAN_POINT('Ctrl Pts',(96.8106284182255,1.12451635991016,-3.82447751094567));
#26527=CARTESIAN_POINT('Ctrl Pts',(96.8042014244256,1.12649745913283,-3.82402199805452));
#26528=CARTESIAN_POINT('Ctrl Pts',(96.7878043896812,1.13139840544524,-3.82285828461382));
#26529=CARTESIAN_POINT('Ctrl Pts',(96.7778122096802,1.13424152880405,-3.82214765371291));
#26530=CARTESIAN_POINT('Ctrl Pts',(96.6949406321733,1.15664061680823,-3.81624030382034));
#26531=CARTESIAN_POINT('Ctrl Pts',(96.6203874049229,1.16927965196357,-3.81082198307269));
#26532=CARTESIAN_POINT('Ctrl Pts',(96.4875002722337,1.17885787862336,-3.80107581833461));
#26533=CARTESIAN_POINT('Ctrl Pts',(96.4296211536499,1.17876370206417,-3.79680681915103));
#26534=CARTESIAN_POINT('Ctrl Pts',(96.3515331266551,1.17287934927007,-3.79115184810892));
#26535=CARTESIAN_POINT('Ctrl Pts',(96.3311266675664,1.17080449503297,-3.78968436821272));
#26536=CARTESIAN_POINT('Ctrl Pts',(96.2978331152282,1.16653813278344,-3.78731711268388));
#26537=CARTESIAN_POINT('Ctrl Pts',(96.2849103727789,1.16466327375454,-3.78640498723211));
#26538=CARTESIAN_POINT('Ctrl Pts',(96.2673784809264,1.16182124995771,-3.78517901688589));
#26539=CARTESIAN_POINT('Ctrl Pts',(96.2627405802144,1.16104088147806,-3.78485579640214));
#26540=CARTESIAN_POINT('Ctrl Pts',(96.2549821511836,1.15968761766732,-3.78431708253762));
#26541=CARTESIAN_POINT('Ctrl Pts',(96.2518590779142,1.1591298642319,-3.78410076761551));
#26542=CARTESIAN_POINT('Ctrl Pts',(96.2459276071361,1.1580458061945,-3.78369100558806));
#26543=CARTESIAN_POINT('Ctrl Pts',(96.243118819702,1.15752189220615,-3.78349742270611));
#26544=CARTESIAN_POINT('Ctrl Pts',(96.2364430581388,1.15625152795087,-3.78303835076119));
#26545=CARTESIAN_POINT('Ctrl Pts',(96.2325778359534,1.15549588687873,-3.78277337005794));
#26546=CARTESIAN_POINT('Ctrl Pts',(96.2188972106962,1.15275004244836,-3.78183816293063));
#26547=CARTESIAN_POINT('Ctrl Pts',(96.2091031503131,1.15065397996251,-3.7811735180152));
#26548=CARTESIAN_POINT('Ctrl Pts',(96.1380417633,1.1344952006867,-3.77637880967278));
#26549=CARTESIAN_POINT('Ctrl Pts',(96.0779526476298,1.11567045718616,-3.77247141370119));
#26550=CARTESIAN_POINT('Ctrl Pts',(95.9863515882459,1.0786962632783,-3.76635554633995));
#26551=CARTESIAN_POINT('Ctrl Pts',(95.9537030471759,1.06374721732549,-3.76414223687867));
#26552=CARTESIAN_POINT('Ctrl Pts',(95.921801595944,1.04733930341107,-3.76190742309816));
#26553=CARTESIAN_POINT('Ctrl Pts',(95.9218017102038,1.04733936217842,-3.66210953954391));
#26554=CARTESIAN_POINT('Ctrl Pts',(95.9515268869871,1.06262794599194,-3.66423180197923));
#26555=CARTESIAN_POINT('Ctrl Pts',(95.9818955288735,1.07664727186504,-3.66638568234305));
#26556=CARTESIAN_POINT('Ctrl Pts',(96.0228467717177,1.09347553603074,-3.66929554572374));
#26557=CARTESIAN_POINT('Ctrl Pts',(96.0329230079188,1.09745460738624,-3.67001189273349));
#26558=CARTESIAN_POINT('Ctrl Pts',(96.048871483371,1.1034996311513,-3.6711469749985));
#26559=CARTESIAN_POINT('Ctrl Pts',(96.0547078278261,1.10565906127483,-3.67156261982445));
#26560=CARTESIAN_POINT('Ctrl Pts',(96.0656666565797,1.10961533993984,-3.67234369088225));
#26561=CARTESIAN_POINT('Ctrl Pts',(96.070785002189,1.11142322968553,-3.67270874303795));
#26562=CARTESIAN_POINT('Ctrl Pts',(96.0822719393112,1.11539151514891,-3.67352866999955));
#26563=CARTESIAN_POINT('Ctrl Pts',(96.0886468625273,1.11753286125163,-3.67398415260324));
#26564=CARTESIAN_POINT('Ctrl Pts',(96.1049151177559,1.12284278338375,-3.67514780463955));
#26565=CARTESIAN_POINT('Ctrl Pts',(96.1148325027915,1.12593521847783,-3.67585840429814));
#26566=CARTESIAN_POINT('Ctrl Pts',(96.197003849725,1.1503699241136,-3.68175763365032));
#26567=CARTESIAN_POINT('Ctrl Pts',(96.2710987987834,1.16486122859366,-3.68716712787284));
#26568=CARTESIAN_POINT('Ctrl Pts',(96.4040199070875,1.17783656282554,-3.69693638596119));
#26569=CARTESIAN_POINT('Ctrl Pts',(96.4623236931921,1.17918772060614,-3.70123818129027));
#26570=CARTESIAN_POINT('Ctrl Pts',(96.5407701351531,1.17518556088752,-3.7069088198823));
#26571=CARTESIAN_POINT('Ctrl Pts',(96.5610223131808,1.17362642584868,-3.70836162632931));
#26572=CARTESIAN_POINT('Ctrl Pts',(96.5941213928752,1.17021509719897,-3.71070792309368));
#26573=CARTESIAN_POINT('Ctrl Pts',(96.6069954733692,1.16867303846211,-3.71161351018801));
#26574=CARTESIAN_POINT('Ctrl Pts',(96.6244889818733,1.16628402372226,-3.71283217743795));
#26575=CARTESIAN_POINT('Ctrl Pts',(96.6291321218656,1.16562165500001,-3.71315449431352));
#26576=CARTESIAN_POINT('Ctrl Pts',(96.6369063434911,1.16446519441425,-3.71369211061008));
#26577=CARTESIAN_POINT('Ctrl Pts',(96.6400395725906,1.16398617273104,-3.71390822472739));
#26578=CARTESIAN_POINT('Ctrl Pts',(96.6459955072885,1.16305098191484,-3.7143179206363));
#26579=CARTESIAN_POINT('Ctrl Pts',(96.6488185360568,1.16259717512939,-3.71451163617588));
#26580=CARTESIAN_POINT('Ctrl Pts',(96.6555345358518,1.16149246204784,-3.71497141652787));
#26581=CARTESIAN_POINT('Ctrl Pts',(96.6594259737464,1.16083225290393,-3.71523696916608));
#26582=CARTESIAN_POINT('Ctrl Pts',(96.6732313306764,1.15841861855702,-3.71617624146788));
#26583=CARTESIAN_POINT('Ctrl Pts',(96.6831263395424,1.15655759362003,-3.71684431614451));
#26584=CARTESIAN_POINT('Ctrl Pts',(96.7513604548066,1.14281610849804,-3.72142318651043));
#26585=CARTESIAN_POINT('Ctrl Pts',(96.8087568803161,1.12665222691,-3.72513507346931));
#26586=CARTESIAN_POINT('Ctrl Pts',(96.9277443362566,1.08317431244778,-3.73298451711651));
#26587=CARTESIAN_POINT('Ctrl Pts',(96.9887091822793,1.05478718415412,-3.73710555889721));
#26588=CARTESIAN_POINT('Ctrl Pts',(97.0767544313278,1.00423373433936,-3.74355951432544));
#26589=CARTESIAN_POINT('Ctrl Pts',(97.105819040385,0.985807687838174,-3.74577974511669));
#26590=CARTESIAN_POINT('Ctrl Pts',(97.1419026430924,0.960651629002051,-3.74867849749104));
#26591=CARTESIAN_POINT('Ctrl Pts',(97.1497040161767,0.955069961950332,-3.74931408220337));
#26592=CARTESIAN_POINT('Ctrl Pts',(97.1622349803165,0.945870911919544,-3.75034996343363));
#26593=CARTESIAN_POINT('Ctrl Pts',(97.1670069518168,0.942311788970393,-3.75074803134951));
#26594=CARTESIAN_POINT('Ctrl Pts',(97.1761198859155,0.935406869561338,-3.75151526157703));
#26595=CARTESIAN_POINT('Ctrl Pts',(97.1804648885275,0.932066641790059,-3.75188420145349));
#26596=CARTESIAN_POINT('Ctrl Pts',(97.190365185883,0.924345237879084,-3.75273214712997));
#26597=CARTESIAN_POINT('Ctrl Pts',(97.1959045870653,0.919944121586319,-3.75321192730596));
#26598=CARTESIAN_POINT('Ctrl Pts',(97.2134273963945,0.90576264209704,-3.75474698366367));
#26599=CARTESIAN_POINT('Ctrl Pts',(97.225257510117,0.895796343278268,-3.75580960788472));
#26600=CARTESIAN_POINT('Ctrl Pts',(97.2966710054717,0.833188077926024,-3.76239118709433));
#26601=CARTESIAN_POINT('Ctrl Pts',(97.3509833129435,0.774866119990202,-3.76814816727417));
#26602=CARTESIAN_POINT('Ctrl Pts',(97.4270599432811,0.674520055100196,-3.77738369027458));
#26603=CARTESIAN_POINT('Ctrl Pts',(97.4529066846545,0.635880240891937,-3.78080193022208));
#26604=CARTESIAN_POINT('Ctrl Pts',(97.4870930839258,0.577588939991635,-3.78568600736881));
#26605=CARTESIAN_POINT('Ctrl Pts',(97.4972899128815,0.559078473068036,-3.78719921451562));
#26606=CARTESIAN_POINT('Ctrl Pts',(97.5131032635276,0.528449867987034,-3.78963151971322));
#26607=CARTESIAN_POINT('Ctrl Pts',(97.5190212880641,0.516493357386152,-3.79056377237304));
#26608=CARTESIAN_POINT('Ctrl Pts',(97.5267659304711,0.500153858393739,-3.79181211389401));
#26609=CARTESIAN_POINT('Ctrl Pts',(97.5287708202033,0.495857133452275,-3.79213801266752));
#26610=CARTESIAN_POINT('Ctrl Pts',(97.5320770302862,0.488658383488655,-3.79267993169569));
#26611=CARTESIAN_POINT('Ctrl Pts',(97.5333926242884,0.485763023458646,-3.79289679414801));
#26612=CARTESIAN_POINT('Ctrl Pts',(97.5358649758358,0.480262825189689,-3.79330663025232));
#26613=CARTESIAN_POINT('Ctrl Pts',(97.537024029107,0.47765906622593,-3.79349974579894));
#26614=CARTESIAN_POINT('Ctrl Pts',(97.5397510008933,0.471472705207028,-3.79395650784794));
#26615=CARTESIAN_POINT('Ctrl Pts',(97.5413105623929,0.467886422720148,-3.79421965789962));
#26616=CARTESIAN_POINT('Ctrl Pts',(97.5467354837077,0.455239695140926,-3.79514210961642));
#26617=CARTESIAN_POINT('Ctrl Pts',(97.5505051397222,0.44613828955518,-3.7957960258593));
#26618=CARTESIAN_POINT('Ctrl Pts',(97.5798555082221,0.372681527804028,-3.80100264574118));
#26619=CARTESIAN_POINT('Ctrl Pts',(97.5998322490202,0.306222441885801,-3.80528293609165));
#26620=CARTESIAN_POINT('Ctrl Pts',(97.6300381185647,0.160078133085932,-3.81451463964493));
#26621=CARTESIAN_POINT('Ctrl Pts',(97.6382047189824,0.0803358707141346,
-3.81945264061806));
#26622=CARTESIAN_POINT('Ctrl Pts',(97.6382363426027,-0.0162844948558244,
-3.82573338268351));
#26623=CARTESIAN_POINT('Ctrl Pts',(97.637887876712,-0.0329519786022189,
-3.82682672382451));
#26624=CARTESIAN_POINT('Ctrl Pts',(97.6368988735683,-0.0564122383090384,
-3.82838212366944));
#26625=CARTESIAN_POINT('Ctrl Pts',(97.6365528920283,-0.0632159430142647,
-3.82883515389796));
#26626=CARTESIAN_POINT('Ctrl Pts',(97.635846207896,-0.0750821372014775,
-3.82962885086424));
#26627=CARTESIAN_POINT('Ctrl Pts',(97.6355117687516,-0.0801460567420147,
-3.82996870034848));
#26628=CARTESIAN_POINT('Ctrl Pts',(97.6347412397145,-0.0907684961572817,
-3.83068405810339));
#26629=CARTESIAN_POINT('Ctrl Pts',(97.6342983863317,-0.0963263838305222,
-3.83105976722223));
#26630=CARTESIAN_POINT('Ctrl Pts',(97.6331438519652,-0.109622856386331,
-3.83196209773226));
#26631=CARTESIAN_POINT('Ctrl Pts',(97.6323950160105,-0.117357867915084,
-3.83248985639087));
#26632=CARTESIAN_POINT('Ctrl Pts',(97.6295399082135,-0.144088422782283,
-3.83432384392705));
#26633=CARTESIAN_POINT('Ctrl Pts',(97.6270479564917,-0.163038850508583,
-3.83564189020267));
#26634=CARTESIAN_POINT('Ctrl Pts',(97.6198477310537,-0.209093832604273,
-3.83889070061058));
#26635=CARTESIAN_POINT('Ctrl Pts',(97.6146489654909,-0.236109201794215,
-3.84083543160626));
#26636=CARTESIAN_POINT('Ctrl Pts',(97.5851904943787,-0.364740231850199,
-3.85027928674959));
#26637=CARTESIAN_POINT('Ctrl Pts',(97.5484325069005,-0.462995603980884,
-3.8581047594782));
#26638=CARTESIAN_POINT('Ctrl Pts',(97.4892455643655,-0.573746394863369,
-3.86708003621099));
#26639=CARTESIAN_POINT('Ctrl Pts',(97.4787856183896,-0.592112568877566,
-3.86857189979597));
#26640=CARTESIAN_POINT('Ctrl Pts',(97.4648236390865,-0.61516228612518,-3.87043967245905));
#26641=CARTESIAN_POINT('Ctrl Pts',(97.4617740552052,-0.6201136963075,-3.87084061983158));
#26642=CARTESIAN_POINT('Ctrl Pts',(97.456875314224,-0.627937096285412,-3.87147344293429));
#26643=CARTESIAN_POINT('Ctrl Pts',(97.4550501708214,-0.630823899116125,
-3.87170680191852));
#26644=CARTESIAN_POINT('Ctrl Pts',(97.451553757369,-0.636301230139754,-3.87214922306961));
#26645=CARTESIAN_POINT('Ctrl Pts',(97.4498848868775,-0.63889311695495,-3.87235842122598));
#26646=CARTESIAN_POINT('Ctrl Pts',(97.4459108392278,-0.645012208429669,
-3.87285199448922));
#26647=CARTESIAN_POINT('Ctrl Pts',(97.4435968817139,-0.648533639668521,
-3.87313579247093));
#26648=CARTESIAN_POINT('Ctrl Pts',(97.4357999837315,-0.660261500875621,
-3.87408041025011));
#26649=CARTESIAN_POINT('Ctrl Pts',(97.4302326213255,-0.66841168361064,-3.8747359590946));
#26650=CARTESIAN_POINT('Ctrl Pts',(97.4164945853823,-0.687990055566336,
-3.87631103018823));
#26651=CARTESIAN_POINT('Ctrl Pts',(97.4082204708455,-0.699344139352951,
-3.87722472673215));
#26652=CARTESIAN_POINT('Ctrl Pts',(97.3746373162585,-0.743737261580293,
-3.88081002187701));
#26653=CARTESIAN_POINT('Ctrl Pts',(97.3477863046998,-0.775575087314057,
-3.88341080970137));
#26654=CARTESIAN_POINT('Ctrl Pts',(97.2521186001174,-0.877521896547881,
-3.89208627008442));
#26655=CARTESIAN_POINT('Ctrl Pts',(97.1762527327695,-0.940427330348799,
-3.89807945080254));
#26656=CARTESIAN_POINT('Ctrl Pts',(97.081528532809,-1.00079733566589,-3.90541590736069));
#26657=CARTESIAN_POINT('Ctrl Pts',(97.069456530984,-1.00818853447668,-3.90634758187269));
#26658=CARTESIAN_POINT('Ctrl Pts',(97.0513018631366,-1.01885886540171,-3.9077453944503));
#26659=CARTESIAN_POINT('Ctrl Pts',(97.0453185162524,-1.02230511918389,-3.90820555403357));
#26660=CARTESIAN_POINT('Ctrl Pts',(97.0345639164,-1.02837417792903,-3.90903189827456));
#26661=CARTESIAN_POINT('Ctrl Pts',(97.0298040893007,-1.0310169074773,-3.90939736398695));
#26662=CARTESIAN_POINT('Ctrl Pts',(97.0196686280309,-1.03655268493383,-3.9101751149256));
#26663=CARTESIAN_POINT('Ctrl Pts',(97.0142884976244,-1.03943711963902,-3.91058768937873));
#26664=CARTESIAN_POINT('Ctrl Pts',(96.9997823754827,-1.0470696540993,-3.91169949766233));
#26665=CARTESIAN_POINT('Ctrl Pts',(96.9906163697165,-1.05174013577109,-3.91240139870975));
#26666=CARTESIAN_POINT('Ctrl Pts',(96.9423934816961,-1.07552126805308,-3.91609191939869));
#26667=CARTESIAN_POINT('Ctrl Pts',(96.9023660789787,-1.09257603743239,-3.91914953686418));
#26668=CARTESIAN_POINT('Ctrl Pts',(96.8088226234813,-1.12645059794053,-3.92628206706657));
#26669=CARTESIAN_POINT('Ctrl Pts',(96.7548636229608,-1.14174025254999,-3.9303889318132));
#26670=CARTESIAN_POINT('Ctrl Pts',(96.6409953673109,-1.16539462608383,-3.93892369958369));
#26671=CARTESIAN_POINT('Ctrl Pts',(96.5811038662848,-1.17310769041009,-3.94333982433224));
#26672=CARTESIAN_POINT('Ctrl Pts',(96.510870684196,-1.17671423361306,-3.94827141649339));
#26673=CARTESIAN_POINT('Ctrl Pts',(96.5008548027134,-1.17710045515829,-3.94896875577648));
#26674=CARTESIAN_POINT('Ctrl Pts',(96.4868967771687,-1.17746031140682,-3.94993118794331));
#26675=CARTESIAN_POINT('Ctrl Pts',(96.4829581918344,-1.17754208229713,-3.95020172170389));
#26676=CARTESIAN_POINT('Ctrl Pts',(96.4761622693112,-1.17764906605842,-3.95066664405474));
#26677=CARTESIAN_POINT('Ctrl Pts',(96.4733051452017,-1.17768364471443,-3.95086153344227));
#26678=CARTESIAN_POINT('Ctrl Pts',(96.4672762475857,-1.17773466724409,-3.95127152854621));
#26679=CARTESIAN_POINT('Ctrl Pts',(96.4641044818367,-1.17774869685962,-3.95148649384838));
#26680=CARTESIAN_POINT('Ctrl Pts',(96.4562321255529,-1.17775171621336,-3.95201831150723));
#26681=CARTESIAN_POINT('Ctrl Pts',(96.451531520822,-1.17772537849062,-3.95233433207218));
#26682=CARTESIAN_POINT('Ctrl Pts',(96.4337912423027,-1.17751975897642,-3.95352166041228));
#26683=CARTESIAN_POINT('Ctrl Pts',(96.4207541241647,-1.1771520451121,-3.95438331243923));
#26684=CARTESIAN_POINT('Ctrl Pts',(96.3872725585644,-1.17565077445741,-3.95657432247968));
#26685=CARTESIAN_POINT('Ctrl Pts',(96.3668461195623,-1.17420050673262,-3.95789005850836));
#26686=CARTESIAN_POINT('Ctrl Pts',(96.2889044961393,-1.16661962028242,-3.96286507304348));
#26687=CARTESIAN_POINT('Ctrl Pts',(96.2318294492956,-1.15678827488558,-3.96641624874181));
#26688=CARTESIAN_POINT('Ctrl Pts',(96.1024735014979,-1.12455395035829,-3.97467078426801));
#26689=CARTESIAN_POINT('Ctrl Pts',(96.0311759619673,-1.09931157537654,-3.97938421108425));
#26690=CARTESIAN_POINT('Ctrl Pts',(95.9533724197388,-1.0630352425865,-3.98501826155924));
#26691=CARTESIAN_POINT('Ctrl Pts',(95.9440156051416,-1.05852091373772,-3.98570405191449));
#26692=CARTESIAN_POINT('Ctrl Pts',(95.9287021473321,-1.0508813421123,-3.98684071923677));
#26693=CARTESIAN_POINT('Ctrl Pts',(95.9227102560455,-1.0478277376299,-3.98728913689945));
#26694=CARTESIAN_POINT('Ctrl Pts',(95.9119297936061,-1.0422169438252,-3.98810272596984));
#26695=CARTESIAN_POINT('Ctrl Pts',(95.9071320928837,-1.03967762783687,-3.98846726782112));
#26696=CARTESIAN_POINT('Ctrl Pts',(95.8968724016518,-1.03415627051593,-3.98925222574626));
#26697=CARTESIAN_POINT('Ctrl Pts',(95.8914161692256,-1.03116393475531,-3.98967299504892));
#26698=CARTESIAN_POINT('Ctrl Pts',(95.8765274877327,-1.02284444768929,-3.99083045167009));
#26699=CARTESIAN_POINT('Ctrl Pts',(95.8671446173764,-1.01743028904605,-3.99157019762072));
#26700=CARTESIAN_POINT('Ctrl Pts',(95.8120016807602,-0.984589191429312,
-3.99598053235804));
#26701=CARTESIAN_POINT('Ctrl Pts',(95.7680798404003,-0.954211962455254,
-3.99975710092738));
#26702=CARTESIAN_POINT('Ctrl Pts',(95.688870807386,-0.89107398379887,-4.00707829284397));
#26703=CARTESIAN_POINT('Ctrl Pts',(95.6532313882539,-0.858919535469922,
-4.01060041738607));
#26704=CARTESIAN_POINT('Ctrl Pts',(95.5999011707109,-0.804545348895044,
-4.01618833019146));
#26705=CARTESIAN_POINT('Ctrl Pts',(95.5808784047342,-0.783702897460052,
-4.01825429723871));
#26706=CARTESIAN_POINT('Ctrl Pts',(95.540198999677,-0.73578303617225,-4.02281172736505));
#26707=CARTESIAN_POINT('Ctrl Pts',(95.5189501991657,-0.708389642230496,
-4.02529072609573));
#26708=CARTESIAN_POINT('Ctrl Pts',(95.4954373241675,-0.675146372559369,
-4.02812086975255));
#26709=CARTESIAN_POINT('Ctrl Pts',(95.4919743636547,-0.670169247442457,
-4.02854008529184));
#26710=CARTESIAN_POINT('Ctrl Pts',(95.4863891867297,-0.662008260324498,
-4.0292198728282));
#26711=CARTESIAN_POINT('Ctrl Pts',(95.4842438275171,-0.658840482770103,
-4.02948189459992));
#26712=CARTESIAN_POINT('Ctrl Pts',(95.4804203726468,-0.653135194363557,
-4.02995042402147));
#26713=CARTESIAN_POINT('Ctrl Pts',(95.4787366424171,-0.65060159281068,-4.03015729542395));
#26714=CARTESIAN_POINT('Ctrl Pts',(95.475047837898,-0.645003916828311,-4.03061172876866));
#26715=CARTESIAN_POINT('Ctrl Pts',(95.4730472263281,-0.641937001129624,
-4.03085899907545));
#26716=CARTESIAN_POINT('Ctrl Pts',(95.4672861632851,-0.63301469504223,-4.03157357152226));
#26717=CARTESIAN_POINT('Ctrl Pts',(95.4635631838213,-0.627135122405331,
-4.03203851142165));
#26718=CARTESIAN_POINT('Ctrl Pts',(95.4323527311959,-0.576865195737454,
-4.0359665542258));
#26719=CARTESIAN_POINT('Ctrl Pts',(95.4077892952618,-0.530719166968396,
-4.03926307066568));
#26720=CARTESIAN_POINT('Ctrl Pts',(95.3522331404061,-0.407194169962118,
-4.04769989110471));
#26721=CARTESIAN_POINT('Ctrl Pts',(95.3262401268905,-0.327898860002954,
-4.05276392249761));
#26722=CARTESIAN_POINT('Ctrl Pts',(95.3023784675555,-0.216428134594552,
-4.06003510820345));
#26723=CARTESIAN_POINT('Ctrl Pts',(95.2971183977458,-0.186090875366485,
-4.06202644634381));
#26724=CARTESIAN_POINT('Ctrl Pts',(95.2917886172872,-0.146098828993867,
-4.06468537289301));
#26725=CARTESIAN_POINT('Ctrl Pts',(95.290640159318,-0.136598506399567,-4.06531945702201));
#26726=CARTESIAN_POINT('Ctrl Pts',(95.2889657955983,-0.121172133677074,
-4.06635349674472));
#26727=CARTESIAN_POINT('Ctrl Pts',(95.2883687839174,-0.115254114454532,
-4.06675123865691));
#26728=CARTESIAN_POINT('Ctrl Pts',(95.2873077223108,-0.103873457179195,
-4.06751825497637));
#26729=CARTESIAN_POINT('Ctrl Pts',(95.2868369348506,-0.0984115909536513,
-4.0678873099811));
#26730=CARTESIAN_POINT('Ctrl Pts',(95.2858354959576,-0.0857616977923087,
-4.06874433526918));
#26731=CARTESIAN_POINT('Ctrl Pts',(95.2853326669055,-0.0785717522666438,
-4.06923315330876));
#26732=CARTESIAN_POINT('Ctrl Pts',(95.2839399005712,-0.0556330266776116,
-4.07079834455299));
#26733=CARTESIAN_POINT('Ctrl Pts',(95.2833003742687,-0.0398713554988464,
-4.07188236138014));
#26734=CARTESIAN_POINT('Ctrl Pts',(95.2825411383615,-0.00277924115063064,
-4.07445468362038));
#26735=CARTESIAN_POINT('Ctrl Pts',(95.2826839780099,0.0185504439796918,
-4.07595048387227));
#26736=CARTESIAN_POINT('Ctrl Pts',(95.2854163022941,0.0992297589523076,
-4.08167153140116));
#26737=CARTESIAN_POINT('Ctrl Pts',(95.2919149668333,0.158352731941786,-4.08599935465944));
#26738=CARTESIAN_POINT('Ctrl Pts',(95.3157921576293,0.285891698711965,-4.09551816113143));
#26739=CARTESIAN_POINT('Ctrl Pts',(95.3349144130465,0.353762984175862,-4.10070379119663));
#26740=CARTESIAN_POINT('Ctrl Pts',(95.3634864226039,0.428712890323207,-4.10632574896784));
#26741=CARTESIAN_POINT('Ctrl Pts',(95.3671037967118,0.437856314178465,-4.10700956872219));
#26742=CARTESIAN_POINT('Ctrl Pts',(95.3723113352837,0.450551971229827,-4.10795518502667));
#26743=CARTESIAN_POINT('Ctrl Pts',(95.3738051131456,0.454142946483366,-4.10822221711789));
#26744=CARTESIAN_POINT('Ctrl Pts',(95.3764222522237,0.460347581128313,-4.10868276865391));
#26745=CARTESIAN_POINT('Ctrl Pts',(95.3775373338572,0.462964664276499,-4.10887676762747));
#26746=CARTESIAN_POINT('Ctrl Pts',(95.3799216710069,0.468504923724802,-4.10928686590806));
#26747=CARTESIAN_POINT('Ctrl Pts',(95.3811933314758,0.471427042060231,-4.1095028142886));
#26748=CARTESIAN_POINT('Ctrl Pts',(95.3843991402755,0.478712630193634,-4.11004043745148));
#26749=CARTESIAN_POINT('Ctrl Pts',(95.3863480067776,0.483069628273673,-4.11036124024081));
#26750=CARTESIAN_POINT('Ctrl Pts',(95.3939410585981,0.49977192997102,-4.11158872913198));
#26751=CARTESIAN_POINT('Ctrl Pts',(95.3997722821058,0.512031720372891,-4.11248489789159));
#26752=CARTESIAN_POINT('Ctrl Pts',(95.4154502778989,0.543575819331392,-4.11478509982836));
#26753=CARTESIAN_POINT('Ctrl Pts',(95.4256194330087,0.562694883782038,-4.11617374178505));
#26754=CARTESIAN_POINT('Ctrl Pts',(95.4868495938651,0.670532461383294,-4.12403552393305));
#26755=CARTESIAN_POINT('Ctrl Pts',(95.5487760141044,0.752574273259843,-4.13017236595481));
#26756=CARTESIAN_POINT('Ctrl Pts',(95.6432647185861,0.848707438179883,-4.13875420775945));
#26757=CARTESIAN_POINT('Ctrl Pts',(95.6669403009432,0.870884394127228,-4.1408491807657));
#26758=CARTESIAN_POINT('Ctrl Pts',(95.698882231083,0.898419429826612,-4.14362734368396));
#26759=CARTESIAN_POINT('Ctrl Pts',(95.7063438938649,0.904691865624664,-4.14427304451585));
#26760=CARTESIAN_POINT('Ctrl Pts',(95.7185126598875,0.914666039006842,-4.14532134415218));
#26761=CARTESIAN_POINT('Ctrl Pts',(95.7231717429527,0.918425847527388,-4.14572161274511));
#26762=CARTESIAN_POINT('Ctrl Pts',(95.732142513252,0.925552867965071,-4.14649033778117));
#26763=CARTESIAN_POINT('Ctrl Pts',(95.7364494030045,0.928925888896804,-4.1468585515916));
#26764=CARTESIAN_POINT('Ctrl Pts',(95.7464184930705,0.936621918562234,-4.14770899166935));
#26765=CARTESIAN_POINT('Ctrl Pts',(95.7520966820182,0.940923767230999,-4.148192023732));
#26766=CARTESIAN_POINT('Ctrl Pts',(95.7701038910706,0.954310809135408,-4.14971984176694));
#26767=CARTESIAN_POINT('Ctrl Pts',(95.7825708610125,0.963206871293486,-4.15077176554917));
#26768=CARTESIAN_POINT('Ctrl Pts',(95.8121427510015,0.983449974141895,-4.1532546369016));
#26769=CARTESIAN_POINT('Ctrl Pts',(95.8293774407727,0.994597679933277,-4.15469239065058));
#26770=CARTESIAN_POINT('Ctrl Pts',(95.8713523060206,1.02021742212127,-4.15817255954176));
#26771=CARTESIAN_POINT('Ctrl Pts',(95.8963386428299,1.03424291463737,-4.16022718895624));
#26772=CARTESIAN_POINT('Ctrl Pts',(95.9218017335164,1.04733937416884,-4.16230107423304));
#26773=CARTESIAN_POINT('Origin',(96.460480949577,-7.19464945638997E-16,
0.924367114736168));
#26774=CARTESIAN_POINT('',(95.9218016616991,1.04733933723095,-4.76237177033706));
#26775=CARTESIAN_POINT('',(95.9218016730721,1.04733934308042,-4.66392061240651));
#26776=CARTESIAN_POINT('',(95.9218016730721,1.04733934308042,0.924367114736168));
#26777=CARTESIAN_POINT('Ctrl Pts',(95.9218016616992,1.04733933723097,-4.76237177033706));
#26778=CARTESIAN_POINT('Ctrl Pts',(95.8347012246739,1.00254086578743,-4.75539525775616));
#26779=CARTESIAN_POINT('Ctrl Pts',(95.7535208930734,0.947046519428651,-4.74809443105733));
#26780=CARTESIAN_POINT('Ctrl Pts',(95.6639682705235,0.867830384068402,-4.73944764246191));
#26781=CARTESIAN_POINT('Ctrl Pts',(95.6481787712183,0.853069345358054,-4.73789897688971));
#26782=CARTESIAN_POINT('Ctrl Pts',(95.623159246682,0.828354513726947,-4.73541640195253));
#26783=CARTESIAN_POINT('Ctrl Pts',(95.6136796585851,0.818661375359814,-4.73446869999629));
#26784=CARTESIAN_POINT('Ctrl Pts',(95.6010928263053,0.805338361061766,-4.73320319573871));
#26785=CARTESIAN_POINT('Ctrl Pts',(95.5978376230209,0.801850556732903,-4.73287524435591));
#26786=CARTESIAN_POINT('Ctrl Pts',(95.5924436469209,0.796000287382914,-4.73233084194692));
#26787=CARTESIAN_POINT('Ctrl Pts',(95.5902931386447,0.79364878299064,-4.73211353296923));
#26788=CARTESIAN_POINT('Ctrl Pts',(95.5862404547181,0.789181041216751,-4.73170355806071));
#26789=CARTESIAN_POINT('Ctrl Pts',(95.5843363648138,0.787066595463981,-4.731510745704));
#26790=CARTESIAN_POINT('Ctrl Pts',(95.5798464708034,0.782044192749404,-4.73105557329713));
#26791=CARTESIAN_POINT('Ctrl Pts',(95.5772673586259,0.779130257687243,-4.73079370130664));
#26792=CARTESIAN_POINT('Ctrl Pts',(95.5682150608007,0.768800069573509,-4.72987289190035));
#26793=CARTESIAN_POINT('Ctrl Pts',(95.5618202438687,0.761315253233388,-4.729219344919));
#26794=CARTESIAN_POINT('Ctrl Pts',(95.5106391866561,0.699866738242112,-4.72395504992573));
#26795=CARTESIAN_POINT('Ctrl Pts',(95.4706544204621,0.642073980367331,-4.71962399360956));
#26796=CARTESIAN_POINT('Ctrl Pts',(95.4066641675925,0.52925621426904,-4.7116008978476));
#26797=CARTESIAN_POINT('Ctrl Pts',(95.3812550137345,0.475302714960825,-4.70792249209459));
#26798=CARTESIAN_POINT('Ctrl Pts',(95.3524247886639,0.39970344956206,-4.70276663622895));
#26799=CARTESIAN_POINT('Ctrl Pts',(95.3453584807824,0.379543279563745,-4.70139218763886));
#26800=CARTESIAN_POINT('Ctrl Pts',(95.3340279881147,0.344163024903087,-4.69897246612008));
#26801=CARTESIAN_POINT('Ctrl Pts',(95.329514641391,0.329028317124056,-4.69793502616144));
#26802=CARTESIAN_POINT('Ctrl Pts',(95.3233857146382,0.306857444477711,-4.69640968434447));
#26803=CARTESIAN_POINT('Ctrl Pts',(95.321528213299,0.299889521674802,-4.69592950486378));
#26804=CARTESIAN_POINT('Ctrl Pts',(95.3183712201385,0.287594319115543,-4.69508061451651));
#26805=CARTESIAN_POINT('Ctrl Pts',(95.3170447123704,0.282274150739022,-4.69471277575428));
#26806=CARTESIAN_POINT('Ctrl Pts',(95.3143569496039,0.271164541353731,-4.69394347500008));
#26807=CARTESIAN_POINT('Ctrl Pts',(95.3130023044034,0.265373676984706,-4.69354181479479));
#26808=CARTESIAN_POINT('Ctrl Pts',(95.3095837409847,0.250244172384122,-4.69249056270591));
#26809=CARTESIAN_POINT('Ctrl Pts',(95.3075896492725,0.240890371092452,-4.69183878871913));
#26810=CARTESIAN_POINT('Ctrl Pts',(95.299670255675,0.201389065660143,-4.689077943422));
#26811=CARTESIAN_POINT('Ctrl Pts',(95.2948123800131,0.171042420152743,-4.68693599530511));
#26812=CARTESIAN_POINT('Ctrl Pts',(95.2812094443827,0.0578642779716065,
-4.67886519686011));
#26813=CARTESIAN_POINT('Ctrl Pts',(95.2800702457139,-0.0256267804325326,
-4.67272768336147));
#26814=CARTESIAN_POINT('Ctrl Pts',(95.2925546425887,-0.160534256850619,
-4.6628097713229));
#26815=CARTESIAN_POINT('Ctrl Pts',(95.3008225244471,-0.212171503525447,
-4.65902020042589));
#26816=CARTESIAN_POINT('Ctrl Pts',(95.3140476679167,-0.269878174347515,
-4.65490248137147));
#26817=CARTESIAN_POINT('Ctrl Pts',(95.3156624972256,-0.276648179640297,
-4.6544213060363));
#26818=CARTESIAN_POINT('Ctrl Pts',(95.3182184900759,-0.286958091906697,
-4.65369185114534));
#26819=CARTESIAN_POINT('Ctrl Pts',(95.3191162755502,-0.290508441696048,
-4.65344125728871));
#26820=CARTESIAN_POINT('Ctrl Pts',(95.3207902178706,-0.29700059664494,-4.65298419978233));
#26821=CARTESIAN_POINT('Ctrl Pts',(95.3215612159557,-0.299943593296958,
-4.65277746003812));
#26822=CARTESIAN_POINT('Ctrl Pts',(95.323327609944,-0.306581121299168,-4.65231218853159));
#26823=CARTESIAN_POINT('Ctrl Pts',(95.3243296107321,-0.310273811414395,
-4.65205403496205));
#26824=CARTESIAN_POINT('Ctrl Pts',(95.3269660312562,-0.319805815961665,
-4.6513892961044));
#26825=CARTESIAN_POINT('Ctrl Pts',(95.3286276065488,-0.325637595607847,
-4.65098419495902));
#26826=CARTESIAN_POINT('Ctrl Pts',(95.3400866508788,-0.364708799308417,
-4.6482792332123));
#26827=CARTESIAN_POINT('Ctrl Pts',(95.3513030034805,-0.397518153382198,
-4.64605195702448));
#26828=CARTESIAN_POINT('Ctrl Pts',(95.3742389034827,-0.456035101690588,
-4.6420805647027));
#26829=CARTESIAN_POINT('Ctrl Pts',(95.3854659330351,-0.48190521010964,-4.64032519009879));
#26830=CARTESIAN_POINT('Ctrl Pts',(95.4182613070449,-0.550609915934103,
-4.63560491775258));
#26831=CARTESIAN_POINT('Ctrl Pts',(95.441533316629,-0.592569567299774,-4.63265697659181));
#26832=CARTESIAN_POINT('Ctrl Pts',(95.4959840975354,-0.678004239902656,
-4.62632165899971));
#26833=CARTESIAN_POINT('Ctrl Pts',(95.527693938371,-0.721007095967666,-4.62292878703207));
#26834=CARTESIAN_POINT('Ctrl Pts',(95.569214637721,-0.769971954652902,-4.6187093853385));
#26835=CARTESIAN_POINT('Ctrl Pts',(95.5763353552728,-0.77813816568108,-4.61799295403379));
#26836=CARTESIAN_POINT('Ctrl Pts',(95.5877221186251,-0.790838680966592,
-4.61685774570912));
#26837=CARTESIAN_POINT('Ctrl Pts',(95.5919133010307,-0.795439522345213,
-4.61644205991704));
#26838=CARTESIAN_POINT('Ctrl Pts',(95.5998282497927,-0.80399096019547,-4.61566091602712));
#26839=CARTESIAN_POINT('Ctrl Pts',(95.6035432632299,-0.80794946237382,-4.6152958321088));
#26840=CARTESIAN_POINT('Ctrl Pts',(95.6119216571035,-0.81675419895231,-4.614475838832));
#26841=CARTESIAN_POINT('Ctrl Pts',(95.6165994181131,-0.821586423913875,
-4.61402032161194));
#26842=CARTESIAN_POINT('Ctrl Pts',(95.6286076465615,-0.833780425713611,
-4.61285658961946));
#26843=CARTESIAN_POINT('Ctrl Pts',(95.6359944784468,-0.841085630309066,
-4.61214594436212));
#26844=CARTESIAN_POINT('Ctrl Pts',(95.6977145935018,-0.900529304723208,
-4.60624922040344));
#26845=CARTESIAN_POINT('Ctrl Pts',(95.7568270082685,-0.947434860721522,
-4.6008425117736));
#26846=CARTESIAN_POINT('Ctrl Pts',(95.8688255642208,-1.02001177470005,-4.59108030257034));
#26847=CARTESIAN_POINT('Ctrl Pts',(95.9199293773333,-1.04799063362938,-4.58678278428259));
#26848=CARTESIAN_POINT('Ctrl Pts',(95.9914305047523,-1.08050982922471,-4.58111165693349));
#26849=CARTESIAN_POINT('Ctrl Pts',(96.0101853335513,-1.08845935483474,-4.57965459046969));
#26850=CARTESIAN_POINT('Ctrl Pts',(96.0412267064569,-1.10067693675347,-4.57730219417807));
#26851=CARTESIAN_POINT('Ctrl Pts',(96.0533940070274,-1.10523485992692,-4.57639469465947));
#26852=CARTESIAN_POINT('Ctrl Pts',(96.0700571698512,-1.11116441993027,-4.57517387845173));
#26853=CARTESIAN_POINT('Ctrl Pts',(96.0744889555346,-1.11271167797678,-4.57485128466334));
#26854=CARTESIAN_POINT('Ctrl Pts',(96.0819295432561,-1.11525958762172,-4.57431332295994));
#26855=CARTESIAN_POINT('Ctrl Pts',(96.0849333124509,-1.11627464722792,-4.57409713830684));
#26856=CARTESIAN_POINT('Ctrl Pts',(96.0906532448045,-1.11818187437826,-4.5736873975995));
#26857=CARTESIAN_POINT('Ctrl Pts',(96.0933686059131,-1.11907629899786,-4.57349370720699));
#26858=CARTESIAN_POINT('Ctrl Pts',(96.0998384417324,-1.12118134359577,-4.57303409712102));
#26859=CARTESIAN_POINT('Ctrl Pts',(96.103595824904,-1.12238301510144,-4.57276868859318));
#26860=CARTESIAN_POINT('Ctrl Pts',(96.1169505731618,-1.12658023389055,-4.57183047573469));
#26861=CARTESIAN_POINT('Ctrl Pts',(96.1265805030767,-1.12947184614344,-4.57116329968445));
#26862=CARTESIAN_POINT('Ctrl Pts',(96.1936821126324,-1.14868742231013,-4.56657146246185));
#26863=CARTESIAN_POINT('Ctrl Pts',(96.2522935904987,-1.16074298340619,-4.56284722074856));
#26864=CARTESIAN_POINT('Ctrl Pts',(96.3757629681837,-1.1764799858717,-4.55513535410812));
#26865=CARTESIAN_POINT('Ctrl Pts',(96.4405141830677,-1.1793570731058,-4.5511616457911));
#26866=CARTESIAN_POINT('Ctrl Pts',(96.5414528611269,-1.17552404531606,-4.54475317905771));
#26867=CARTESIAN_POINT('Ctrl Pts',(96.5776469915129,-1.17246959302739,-4.54241357809435));
#26868=CARTESIAN_POINT('Ctrl Pts',(96.6233142054462,-1.16648000324601,-4.53937944958983));
#26869=CARTESIAN_POINT('Ctrl Pts',(96.6329722487484,-1.16509098764696,-4.53873312316518));
#26870=CARTESIAN_POINT('Ctrl Pts',(96.6485289970504,-1.16265595374776,-4.5376840328032));
#26871=CARTESIAN_POINT('Ctrl Pts',(96.6544390626157,-1.16168463151129,-4.53728360526223));
#26872=CARTESIAN_POINT('Ctrl Pts',(96.6657325195258,-1.15973996300852,-4.53651472578175));
#26873=CARTESIAN_POINT('Ctrl Pts',(96.6711170547628,-1.15877410146491,-4.53614651764069));
#26874=CARTESIAN_POINT('Ctrl Pts',(96.6833776198437,-1.15648655946073,-4.53530432027431));
#26875=CARTESIAN_POINT('Ctrl Pts',(96.690248930002,-1.15514101275008,-4.5348295926145));
#26876=CARTESIAN_POINT('Ctrl Pts',(96.7118647970285,-1.1507076761245,-4.5333273536103));
#26877=CARTESIAN_POINT('Ctrl Pts',(96.7265618346173,-1.14739832701777,-4.53229293134626));
#26878=CARTESIAN_POINT('Ctrl Pts',(96.8273990957307,-1.12265115980613,-4.52510234999425));
#26879=CARTESIAN_POINT('Ctrl Pts',(96.9109237320985,-1.09181964092174,-4.51864161842532));
#26880=CARTESIAN_POINT('Ctrl Pts',(97.0073579413313,-1.04325962846799,-4.51071740751488));
#26881=CARTESIAN_POINT('Ctrl Pts',(97.0243245022384,-1.03418835750193,-4.50930576916079));
#26882=CARTESIAN_POINT('Ctrl Pts',(97.0702300348611,-1.00817907524102,-4.50544814754966));
#26883=CARTESIAN_POINT('Ctrl Pts',(97.0986817754473,-0.990413552212167,
-4.5030140277712));
#26884=CARTESIAN_POINT('Ctrl Pts',(97.1414414291249,-0.961105172002238,
-4.49932555233204));
#26885=CARTESIAN_POINT('Ctrl Pts',(97.1563020462211,-0.950401714632761,
-4.49803776434283));
#26886=CARTESIAN_POINT('Ctrl Pts',(97.1751522891448,-0.936145425003434,
-4.49640249695755));
#26887=CARTESIAN_POINT('Ctrl Pts',(97.1793748957116,-0.932906681969083,
-4.49603606978881));
#26888=CARTESIAN_POINT('Ctrl Pts',(97.1861853252887,-0.927609375516879,
-4.49544508483991));
#26889=CARTESIAN_POINT('Ctrl Pts',(97.1887866272117,-0.925568384876944,
-4.49521935478727));
#26890=CARTESIAN_POINT('Ctrl Pts',(97.1938059771246,-0.92159592197977,-4.49478385592261));
#26891=CARTESIAN_POINT('Ctrl Pts',(97.1962250459675,-0.919665843841556,
-4.49457400008569));
#26892=CARTESIAN_POINT('Ctrl Pts',(97.201568836087,-0.915367668419748,-4.49411042843509));
#26893=CARTESIAN_POINT('Ctrl Pts',(97.2044898992085,-0.912995020664015,
-4.49385703007945));
#26894=CARTESIAN_POINT('Ctrl Pts',(97.2145693318613,-0.904727453223364,
-4.49298246162963));
#26895=CARTESIAN_POINT('Ctrl Pts',(97.221669642541,-0.898761837050916,-4.49236604818108));
#26896=CARTESIAN_POINT('Ctrl Pts',(97.2902489084566,-0.839746402344359,
-4.48640059101291));
#26897=CARTESIAN_POINT('Ctrl Pts',(97.3461654807295,-0.780548362330831,
-4.48143326757323));
#26898=CARTESIAN_POINT('Ctrl Pts',(97.4273599773606,-0.67452006980631,-4.47316752189625));
#26899=CARTESIAN_POINT('Ctrl Pts',(97.4563644964034,-0.630910246115097,
-4.46991576860415));
#26900=CARTESIAN_POINT('Ctrl Pts',(97.4922181820308,-0.568335790685192,
-4.46530751887286));
#26901=CARTESIAN_POINT('Ctrl Pts',(97.5016286453381,-0.550907157973189,
-4.46403017302286));
#26902=CARTESIAN_POINT('Ctrl Pts',(97.5173409640515,-0.519965355814765,
-4.46176651236397));
#26903=CARTESIAN_POINT('Ctrl Pts',(97.5238341073371,-0.506554134239694,
-4.46078668075241));
#26904=CARTESIAN_POINT('Ctrl Pts',(97.5330208361816,-0.486623996754391,
-4.45933065680798));
#26905=CARTESIAN_POINT('Ctrl Pts',(97.535913258294,-0.480197947027818,-4.4588612098649));
#26906=CARTESIAN_POINT('Ctrl Pts',(97.5409444617384,-0.468746716288336,
-4.45802449417507));
#26907=CARTESIAN_POINT('Ctrl Pts',(97.5431063043181,-0.463731845684422,
-4.45765801507503));
#26908=CARTESIAN_POINT('Ctrl Pts',(97.5475802070877,-0.453151831021365,
-4.45688463958896));
#26909=CARTESIAN_POINT('Ctrl Pts',(97.5498845804596,-0.447583628309523,
-4.45647749841987));
#26910=CARTESIAN_POINT('Ctrl Pts',(97.5558712789293,-0.432797432693821,
-4.45539590302844));
#26911=CARTESIAN_POINT('Ctrl Pts',(97.5594799074409,-0.423550317600299,
-4.45471902859541));
#26912=CARTESIAN_POINT('Ctrl Pts',(97.5749835281572,-0.382289675627383,
-4.45169602282746));
#26913=CARTESIAN_POINT('Ctrl Pts',(97.5855985605515,-0.349816162994044,
-4.44930872869938));
#26914=CARTESIAN_POINT('Ctrl Pts',(97.6236688017928,-0.21356115932731,-4.43925350913957));
#26915=CARTESIAN_POINT('Ctrl Pts',(97.6382813346104,-0.106748830692155,
-4.43122188222926));
#26916=CARTESIAN_POINT('Ctrl Pts',(97.6382188276505,0.0260264136737434,
-4.42168050861395));
#26917=CARTESIAN_POINT('Ctrl Pts',(97.6373804869628,0.0514935380240259,
-4.41987383687667));
#26918=CARTESIAN_POINT('Ctrl Pts',(97.6353178817726,0.0830092683104523,
-4.41768227628789));
#26919=CARTESIAN_POINT('Ctrl Pts',(97.6348716614224,0.0891000326231811,
-4.41726079187598));
#26920=CARTESIAN_POINT('Ctrl Pts',(97.6340939644511,0.0986909873160142,
-4.41660062081228));
#26921=CARTESIAN_POINT('Ctrl Pts',(97.6337941655065,0.102193531104669,-4.41636027383454));
#26922=CARTESIAN_POINT('Ctrl Pts',(97.6332317415458,0.108435299120317,-4.4159333454051));
#26923=CARTESIAN_POINT('Ctrl Pts',(97.6329751998713,0.111174940632863,-4.41574643996885));
#26924=CARTESIAN_POINT('Ctrl Pts',(97.6323360421851,0.117752185414445,-4.41529885623522));
#26925=CARTESIAN_POINT('Ctrl Pts',(97.6319441761344,0.121588836339259,-4.41503869126701));
#26926=CARTESIAN_POINT('Ctrl Pts',(97.6306900550845,0.133298291849693,-4.41424729003307));
#26927=CARTESIAN_POINT('Ctrl Pts',(97.6297672085535,0.14116457830115,-4.41371925800698));
#26928=CARTESIAN_POINT('Ctrl Pts',(97.6274311148989,0.159478890337525,-4.41249709186862));
#26929=CARTESIAN_POINT('Ctrl Pts',(97.6259567737815,0.169918583420597,-4.41180589953393));
#26930=CARTESIAN_POINT('Ctrl Pts',(97.620284302685,0.206527562241394,-4.4093969341489));
#26931=CARTESIAN_POINT('Ctrl Pts',(97.6153430592409,0.23257503949253,-4.40770961720868));
#26932=CARTESIAN_POINT('Ctrl Pts',(97.5923711993018,0.334711730910872,-4.40112232704819));
#26933=CARTESIAN_POINT('Ctrl Pts',(97.5676631781332,0.409091364103382,-4.39637688490095));
#26934=CARTESIAN_POINT('Ctrl Pts',(97.5166152067053,0.523334619492289,-4.38851878235687));
#26935=CARTESIAN_POINT('Ctrl Pts',(97.4949212365808,0.565005487096903,-4.38552174812203));
#26936=CARTESIAN_POINT('Ctrl Pts',(97.4652765133273,0.614488798130523,-4.38173090018636));
#26937=CARTESIAN_POINT('Ctrl Pts',(97.4596264693501,0.623633566928062,-4.38102020894016));
#26938=CARTESIAN_POINT('Ctrl Pts',(97.4504852250847,0.637985798154637,-4.37988797536627));
#26939=CARTESIAN_POINT('Ctrl Pts',(97.4470761666952,0.643245069293355,-4.37946942968615));
#26940=CARTESIAN_POINT('Ctrl Pts',(97.4409370880032,0.65255241979169,-4.37872207873026));
#26941=CARTESIAN_POINT('Ctrl Pts',(97.4382235460922,0.656611234814684,-4.37839388868141));
#26942=CARTESIAN_POINT('Ctrl Pts',(97.4318792876369,0.665974208798717,-4.37763143923391));
#26943=CARTESIAN_POINT('Ctrl Pts',(97.4282302570304,0.671265709734011,-4.37719650234518));
#26944=CARTESIAN_POINT('Ctrl Pts',(97.4177651952761,0.686178519428217,-4.37595906563329));
#26945=CARTESIAN_POINT('Ctrl Pts',(97.4108479010198,0.695727480897372,-4.37515276539066));
#26946=CARTESIAN_POINT('Ctrl Pts',(97.3538195817302,0.772014331851954,-4.36859523000623));
#26947=CARTESIAN_POINT('Ctrl Pts',(97.2968970398898,0.833344500572717,-4.36257031313806));
#26948=CARTESIAN_POINT('Ctrl Pts',(97.1779761153996,0.93691644309143,-4.35100827918186));
#26949=CARTESIAN_POINT('Ctrl Pts',(97.1174728085043,0.980293475811746,-4.34552241967781));
#26950=CARTESIAN_POINT('Ctrl Pts',(97.044956389199,1.02253428325201,-4.33964257189854));
#26951=CARTESIAN_POINT('Ctrl Pts',(97.0365711342112,1.02728185711396,-4.33897262106573));
#26952=CARTESIAN_POINT('Ctrl Pts',(97.0247336215906,1.03379349722139,-4.3380416770788));
#26953=CARTESIAN_POINT('Ctrl Pts',(97.0213297585565,1.03564409296838,-4.33777568363323));
#26954=CARTESIAN_POINT('Ctrl Pts',(97.0151654093495,1.03895619153181,-4.3372971160242));
#26955=CARTESIAN_POINT('Ctrl Pts',(97.0124081295427,1.04042357078429,-4.33708418341315));
#26956=CARTESIAN_POINT('Ctrl Pts',(97.006761035785,1.04340009478161,-4.33665043217467));
#26957=CARTESIAN_POINT('Ctrl Pts',(97.0038707413471,1.04490823770965,-4.33642967537922));
#26958=CARTESIAN_POINT('Ctrl Pts',(96.9964330093848,1.04875000655281,-4.3358646867897));
#26959=CARTESIAN_POINT('Ctrl Pts',(96.9918765168696,1.05106609692002,-4.33552152082154));
#26960=CARTESIAN_POINT('Ctrl Pts',(96.9726963770908,1.06065885780377,-4.33408875104513));
#26961=CARTESIAN_POINT('Ctrl Pts',(96.9579364493386,1.06766097054071,-4.33301468913035));
#26962=CARTESIAN_POINT('Ctrl Pts',(96.9172806444448,1.08592181360353,-4.33012040167329));
#26963=CARTESIAN_POINT('Ctrl Pts',(96.891117083937,1.09656048035367,-4.32832732341106));
#26964=CARTESIAN_POINT('Ctrl Pts',(96.7843827455991,1.13555062878009,-4.32119342848089));
#26965=CARTESIAN_POINT('Ctrl Pts',(96.7012227226418,1.15604133647805,-4.31602210525761));
#26966=CARTESIAN_POINT('Ctrl Pts',(96.5786702770097,1.17242863806958,-4.30819773050146));
#26967=CARTESIAN_POINT('Ctrl Pts',(96.5405432495682,1.17564756446844,-4.30573910599759));
#26968=CARTESIAN_POINT('Ctrl Pts',(96.4920489606173,1.1773717997126,-4.30254619707199));
#26969=CARTESIAN_POINT('Ctrl Pts',(96.4817639383707,1.17760261441919,-4.30186535312159));
#26970=CARTESIAN_POINT('Ctrl Pts',(96.4653727626991,1.1777556637092,-4.30077385968397));
#26971=CARTESIAN_POINT('Ctrl Pts',(96.4592678009129,1.17776519694514,-4.30036590724007));
#26972=CARTESIAN_POINT('Ctrl Pts',(96.4482630094765,1.17769681863065,-4.29962785248133));
#26973=CARTESIAN_POINT('Ctrl Pts',(96.4433631846486,1.17763579070686,-4.29929827959192));
#26974=CARTESIAN_POINT('Ctrl Pts',(96.4318272110866,1.17742009810423,-4.29852001879087));
#26975=CARTESIAN_POINT('Ctrl Pts',(96.4251917640885,1.17723990520999,-4.29807055270068));
#26976=CARTESIAN_POINT('Ctrl Pts',(96.4057603250423,1.17654779417199,-4.29674882408161));
#26977=CARTESIAN_POINT('Ctrl Pts',(96.3929710837099,1.17588326559371,-4.29587189834016));
#26978=CARTESIAN_POINT('Ctrl Pts',(96.3099134757336,1.17020816215441,-4.29012921911651));
#26979=CARTESIAN_POINT('Ctrl Pts',(96.2402162297934,1.15911087088923,-4.28507542885213));
#26980=CARTESIAN_POINT('Ctrl Pts',(96.0989802678761,1.12342118331545,-4.27442998008216));
#26981=CARTESIAN_POINT('Ctrl Pts',(96.027954793011,1.09803455198337,-4.26884939094858));
#26982=CARTESIAN_POINT('Ctrl Pts',(95.9470466697245,1.06003769830293,-4.26249433370216));
#26983=CARTESIAN_POINT('Ctrl Pts',(95.9343667356133,1.05380194648143,-4.26149888802261));
#26984=CARTESIAN_POINT('Ctrl Pts',(95.9218016729659,1.04733934302581,-4.26051510683823));
#26985=CARTESIAN_POINT('',(97.6382304530324,-0.00105496753745055,-4.32555915085301));
#26986=CARTESIAN_POINT('Ctrl Pts',(95.9218017335164,1.04733937416884,-4.16230107423304));
#26987=CARTESIAN_POINT('Ctrl Pts',(95.9457162450475,1.0596393512744,-4.16424883281337));
#26988=CARTESIAN_POINT('Ctrl Pts',(95.9700512852212,1.07111986665047,-4.16621353099733));
#26989=CARTESIAN_POINT('Ctrl Pts',(96.0647000849988,1.11186780571143,-4.17376600339058));
#26990=CARTESIAN_POINT('Ctrl Pts',(96.1373956001256,1.13512566236667,-4.17939543747484));
#26991=CARTESIAN_POINT('Ctrl Pts',(96.221115133895,1.15320824440095,-4.18539442314298));
#26992=CARTESIAN_POINT('Ctrl Pts',(96.2304219996601,1.15510092306814,-4.18605457887953));
#26993=CARTESIAN_POINT('Ctrl Pts',(96.2435331394711,1.15760249426119,-4.18697420245168));
#26994=CARTESIAN_POINT('Ctrl Pts',(96.2473187610821,1.15830555962964,-4.1872385174085));
#26995=CARTESIAN_POINT('Ctrl Pts',(96.2541749520513,1.15954413979634,-4.18771495064252));
#26996=CARTESIAN_POINT('Ctrl Pts',(96.257244323834,1.16008605349809,-4.18792741769356));
#26997=CARTESIAN_POINT('Ctrl Pts',(96.263537265392,1.16117136278808,-4.18836129499613));
#26998=CARTESIAN_POINT('Ctrl Pts',(96.266761001518,1.16171353219465,-4.1885826366211));
#26999=CARTESIAN_POINT('Ctrl Pts',(96.2750717470111,1.16307568080579,-4.18915097039064));
#27000=CARTESIAN_POINT('Ctrl Pts',(96.2801620219128,1.16387572293439,-4.18949687208251));
#27001=CARTESIAN_POINT('Ctrl Pts',(96.3017797399913,1.16712816446043,-4.19095718053255));
#27002=CARTESIAN_POINT('Ctrl Pts',(96.3183540485649,1.16926226311029,-4.1920552904058));
#27003=CARTESIAN_POINT('Ctrl Pts',(96.3639988661453,1.17415445074933,-4.1950343413314));
#27004=CARTESIAN_POINT('Ctrl Pts',(96.3931363272957,1.17618553286863,-4.19688615796863));
#27005=CARTESIAN_POINT('Ctrl Pts',(96.5141901216589,1.1801098179909,-4.20448096090975));
#27006=CARTESIAN_POINT('Ctrl Pts',(96.6060894507238,1.17232351091294,-4.21003735479366));
#27007=CARTESIAN_POINT('Ctrl Pts',(96.727039674914,1.14762166589799,-4.21790456378743));
#27008=CARTESIAN_POINT('Ctrl Pts',(96.757661313432,1.14007569949948,-4.21994287512952));
#27009=CARTESIAN_POINT('Ctrl Pts',(96.7972182407172,1.12862585831167,-4.22265629272679));
#27010=CARTESIAN_POINT('Ctrl Pts',(96.8064614033248,1.12582673968716,-4.22329612357076));
#27011=CARTESIAN_POINT('Ctrl Pts',(96.8213583232834,1.12111470960772,-4.22433721650482));
#27012=CARTESIAN_POINT('Ctrl Pts',(96.8270339204875,1.11927190094823,-4.22473620755997));
#27013=CARTESIAN_POINT('Ctrl Pts',(96.8378906958944,1.11565538340907,-4.22550405427505));
#27014=CARTESIAN_POINT('Ctrl Pts',(96.8430739996599,1.11388850763256,-4.22587267897033));
#27015=CARTESIAN_POINT('Ctrl Pts',(96.8546135731407,1.10986487077006,-4.22669799026334));
#27016=CARTESIAN_POINT('Ctrl Pts',(96.8609631159107,1.10758953927005,-4.2271552746661));
#27017=CARTESIAN_POINT('Ctrl Pts',(96.8807835456759,1.10029425672701,-4.2285928523958));
#27018=CARTESIAN_POINT('Ctrl Pts',(96.8941818494641,1.09508228980156,-4.22957940891503));
#27019=CARTESIAN_POINT('Ctrl Pts',(96.9251704421334,1.08236977009613,-4.23189682790372));
#27020=CARTESIAN_POINT('Ctrl Pts',(96.9426797211388,1.07468363575531,-4.23323351717457));
#27021=CARTESIAN_POINT('Ctrl Pts',(97.0047071395935,1.04563414446829,-4.23806834117014));
#27022=CARTESIAN_POINT('Ctrl Pts',(97.0480552104024,1.02190433296309,-4.24163728652058));
#27023=CARTESIAN_POINT('Ctrl Pts',(97.1499071456353,0.957520783112995,-4.25044523361146));
#27024=CARTESIAN_POINT('Ctrl Pts',(97.2064664820061,0.914144840576898,-4.2557144806438));
#27025=CARTESIAN_POINT('Ctrl Pts',(97.2736535014771,0.852206183019933,-4.26223793033431));
#27026=CARTESIAN_POINT('Ctrl Pts',(97.2881842193577,0.838100467955295,-4.26366596117625));
#27027=CARTESIAN_POINT('Ctrl Pts',(97.3063518759381,0.819530516450613,-4.26546601863086));
#27028=CARTESIAN_POINT('Ctrl Pts',(97.3103289107347,0.815405627716726,-4.26586099621162));
#27029=CARTESIAN_POINT('Ctrl Pts',(97.3166153271874,0.808789543714443,-4.26648658819141));
#27030=CARTESIAN_POINT('Ctrl Pts',(97.3189442459837,0.806317163410141,-4.26671863009636));
#27031=CARTESIAN_POINT('Ctrl Pts',(97.3233708420217,0.801576969850555,-4.26716015123629));
#27032=CARTESIAN_POINT('Ctrl Pts',(97.325470316733,0.799310953258028,-4.26736975891984));
#27033=CARTESIAN_POINT('Ctrl Pts',(97.3304402501196,0.793904264175833,-4.26786648562027));
#27034=CARTESIAN_POINT('Ctrl Pts',(97.3333026826138,0.790756213391443,-4.26815301015439));
#27035=CARTESIAN_POINT('Ctrl Pts',(97.3426426176655,0.780371817689689,-4.26908963197026));
#27036=CARTESIAN_POINT('Ctrl Pts',(97.3490478823332,0.773070632916621,-4.26973469230489));
#27037=CARTESIAN_POINT('Ctrl Pts',(97.3815700112641,0.735061230626066,-4.27302930677366));
#27038=CARTESIAN_POINT('Ctrl Pts',(97.4061907091836,0.703102986382873,-4.27558964153519));
#27039=CARTESIAN_POINT('Ctrl Pts',(97.4620625049863,0.622319933320045,-4.28173855853479));
#27040=CARTESIAN_POINT('Ctrl Pts',(97.4914428460861,0.572333441733387,-4.28528276355393));
#27041=CARTESIAN_POINT('Ctrl Pts',(97.5435694844135,0.466500380239278,-4.29262798170492));
#27042=CARTESIAN_POINT('Ctrl Pts',(97.5659462505032,0.410668279389681,-4.29642401419777));
#27043=CARTESIAN_POINT('Ctrl Pts',(97.5870592784507,0.343544176072423,-4.30104299682733));
#27044=CARTESIAN_POINT('Ctrl Pts',(97.5900230283504,0.333670516136409,-4.30172359705247));
#27045=CARTESIAN_POINT('Ctrl Pts',(97.5946987397951,0.317316825295883,-4.30285343429817));
#27046=CARTESIAN_POINT('Ctrl Pts',(97.5964857184333,0.310858690217144,-4.3033002637008));
#27047=CARTESIAN_POINT('Ctrl Pts',(97.5996199451794,0.299143542621406,-4.30411216041211));
#27048=CARTESIAN_POINT('Ctrl Pts',(97.6009861623459,0.293891762997231,-4.30447661026915));
#27049=CARTESIAN_POINT('Ctrl Pts',(97.6038454386111,0.282580351082738,-4.30526270218992));
#27050=CARTESIAN_POINT('Ctrl Pts',(97.6053267188345,0.276517940878452,-4.30568470691842));
#27051=CARTESIAN_POINT('Ctrl Pts',(97.6082583603111,0.264092164704042,-4.30655119583667));
#27052=CARTESIAN_POINT('Ctrl Pts',(97.6097041462393,0.257727952168722,-4.30699580908717));
#27053=CARTESIAN_POINT('Ctrl Pts',(97.6132259145132,0.241606336744269,-4.30812427783247));
#27054=CARTESIAN_POINT('Ctrl Pts',(97.6152309243582,0.231834124568334,-4.30881032795707));
#27055=CARTESIAN_POINT('Ctrl Pts',(97.6312287180095,0.148499076971638,-4.3146790396435));
#27056=CARTESIAN_POINT('Ctrl Pts',(97.6382975384426,0.0737968844927355,
-4.32007700864419));
#27057=CARTESIAN_POINT('Ctrl Pts',(97.6382304769022,-0.0010551707271996,
-4.32555912700301));
#27058=CARTESIAN_POINT('Ctrl Pts',(97.6382304770817,-0.00105497038035304,
-4.32555911232973));
#27059=CARTESIAN_POINT('Ctrl Pts',(97.6381590127215,-0.0808364676042963,
-4.33140225987333));
#27060=CARTESIAN_POINT('Ctrl Pts',(97.6299811960951,-0.160412517676923,
-4.33731172291847));
#27061=CARTESIAN_POINT('Ctrl Pts',(97.6125249667081,-0.244806794199073,
-4.34334031373377));
#27062=CARTESIAN_POINT('Ctrl Pts',(97.6111816025224,-0.251045405210151,
-4.34378442241072));
#27063=CARTESIAN_POINT('Ctrl Pts',(97.608920682197,-0.261145536909812,-4.3445005960345));
#27064=CARTESIAN_POINT('Ctrl Pts',(97.6080342186751,-0.265013785676053,
-4.34477420834012));
#27065=CARTESIAN_POINT('Ctrl Pts',(97.6062877123972,-0.272461884815933,
-4.34529963603447));
#27066=CARTESIAN_POINT('Ctrl Pts',(97.6054304039228,-0.276042323432719,
-4.34555159410763));
#27067=CARTESIAN_POINT('Ctrl Pts',(97.6038342640051,-0.282573017039366,
-4.34600994908937));
#27068=CARTESIAN_POINT('Ctrl Pts',(97.6031007912454,-0.285524446360398,
-4.34621663282572));
#27069=CARTESIAN_POINT('Ctrl Pts',(97.6014243762727,-0.292160268300362,
-4.34668030507632));
#27070=CARTESIAN_POINT('Ctrl Pts',(97.6004750161854,-0.295842955648073,
-4.34693692730569));
#27071=CARTESIAN_POINT('Ctrl Pts',(97.5979850549535,-0.305311848728775,
-4.34759509535677));
#27072=CARTESIAN_POINT('Ctrl Pts',(97.5964181144976,-0.311091105237087,
-4.34799520533479));
#27073=CARTESIAN_POINT('Ctrl Pts',(97.5859054453073,-0.348725579592806,
-4.35059179372531));
#27074=CARTESIAN_POINT('Ctrl Pts',(97.5756638780198,-0.380206929209565,
-4.35272214029631));
#27075=CARTESIAN_POINT('Ctrl Pts',(97.5607027344933,-0.420359675527784,
-4.35543449619461));
#27076=CARTESIAN_POINT('Ctrl Pts',(97.5571830232217,-0.429458730726963,
-4.35604880694301));
#27077=CARTESIAN_POINT('Ctrl Pts',(97.5455701993813,-0.458405696016684,
-4.35800505541286));
#27078=CARTESIAN_POINT('Ctrl Pts',(97.5370480587913,-0.47807715370527,-4.35933744420477));
#27079=CARTESIAN_POINT('Ctrl Pts',(97.5055014729214,-0.545767623324874,
-4.36396592454119));
#27080=CARTESIAN_POINT('Ctrl Pts',(97.4797630093447,-0.592447534941329,
-4.36723890911897));
#27081=CARTESIAN_POINT('Ctrl Pts',(97.4253685574996,-0.676995818616726,
-4.3735535583009));
#27082=CARTESIAN_POINT('Ctrl Pts',(97.3974127317104,-0.715184915811135,
-4.37657393646717));
#27083=CARTESIAN_POINT('Ctrl Pts',(97.3607674773099,-0.759395871460964,
-4.38035025250674));
#27084=CARTESIAN_POINT('Ctrl Pts',(97.3541949200233,-0.767120101510726,
-4.38102102844242));
#27085=CARTESIAN_POINT('Ctrl Pts',(97.3440903625904,-0.778689094559577,
-4.3820430787077));
#27086=CARTESIAN_POINT('Ctrl Pts',(97.340631091064,-0.782596976557167,-4.38239139078954));
#27087=CARTESIAN_POINT('Ctrl Pts',(97.3335546868617,-0.790484809686945,
-4.38310080296619));
#27088=CARTESIAN_POINT('Ctrl Pts',(97.3299360422196,-0.794463230943686,
-4.38346196065832));
#27089=CARTESIAN_POINT('Ctrl Pts',(97.3220812392535,-0.802981041625491,
-4.3842425466257));
#27090=CARTESIAN_POINT('Ctrl Pts',(97.3178361946371,-0.807511977372892,
-4.38466234280406));
#27091=CARTESIAN_POINT('Ctrl Pts',(97.3063214176267,-0.819609089013073,
-4.38579569184843));
#27092=CARTESIAN_POINT('Ctrl Pts',(97.2989862145478,-0.827111881455714,
-4.38651202721525));
#27093=CARTESIAN_POINT('Ctrl Pts',(97.2611887074042,-0.864753379323755,
-4.39017597154798));
#27094=CARTESIAN_POINT('Ctrl Pts',(97.2292015092608,-0.893308030011768,
-4.39319019462524));
#27095=CARTESIAN_POINT('Ctrl Pts',(97.1242259797899,-0.977198211523787,
-4.40282393658955));
#27096=CARTESIAN_POINT('Ctrl Pts',(97.0463098422742,-1.02580495150212,-4.40964147106556));
#27097=CARTESIAN_POINT('Ctrl Pts',(96.9447059589486,-1.07380440723321,-4.41776000124902));
#27098=CARTESIAN_POINT('Ctrl Pts',(96.9256199042467,-1.08220867744155,-4.4192526955667));
#27099=CARTESIAN_POINT('Ctrl Pts',(96.8941626346657,-1.09507432368605,-4.42165032767276));
#27100=CARTESIAN_POINT('Ctrl Pts',(96.8819226021935,-1.09984296505078,-4.42256816157993));
#27101=CARTESIAN_POINT('Ctrl Pts',(96.8651414385208,-1.10605949478209,-4.42380372714481));
#27102=CARTESIAN_POINT('Ctrl Pts',(96.8606680616567,-1.107685873607,-4.42413091014296));
#27103=CARTESIAN_POINT('Ctrl Pts',(96.853185939306,-1.11035489436167,-4.42467437438377));
#27104=CARTESIAN_POINT('Ctrl Pts',(96.8501826467349,-1.11141251943367,-4.42489150772265));
#27105=CARTESIAN_POINT('Ctrl Pts',(96.8444859836768,-1.1133926984969,-4.42530140673185));
#27106=CARTESIAN_POINT('Ctrl Pts',(96.8417935030906,-1.11431768551511,-4.42549431716674));
#27107=CARTESIAN_POINT('Ctrl Pts',(96.8354065372272,-1.11648603256416,-4.42595003672646));
#27108=CARTESIAN_POINT('Ctrl Pts',(96.8317091522699,-1.11772084161616,-4.42621235482406));
#27109=CARTESIAN_POINT('Ctrl Pts',(96.8186909794605,-1.12199677375328,-4.42713093051323));
#27110=CARTESIAN_POINT('Ctrl Pts',(96.8093381059047,-1.12493994757703,-4.42778185371708));
#27111=CARTESIAN_POINT('Ctrl Pts',(96.7325203172675,-1.14806282773389,-4.43306286875708));
#27112=CARTESIAN_POINT('Ctrl Pts',(96.6633971727737,-1.16227425203348,-4.43741078147543));
#27113=CARTESIAN_POINT('Ctrl Pts',(96.5344288176955,-1.17692415923969,-4.44543969979147));
#27114=CARTESIAN_POINT('Ctrl Pts',(96.4750292299028,-1.1791549739972,-4.44910666175506));
#27115=CARTESIAN_POINT('Ctrl Pts',(96.3944125090177,-1.17608866889308,-4.45424789918991));
#27116=CARTESIAN_POINT('Ctrl Pts',(96.3731350917396,-1.1747000534647,-4.45561985497873));
#27117=CARTESIAN_POINT('Ctrl Pts',(96.3362056892201,-1.17128109253765,-4.4580355687082));
#27118=CARTESIAN_POINT('Ctrl Pts',(96.3205348099975,-1.16951219654817,-4.45907152978353));
#27119=CARTESIAN_POINT('Ctrl Pts',(96.2977611770346,-1.16647729297186,-4.46059507133588));
#27120=CARTESIAN_POINT('Ctrl Pts',(96.2906266291146,-1.16545978281375,-4.46107495512229));
#27121=CARTESIAN_POINT('Ctrl Pts',(96.2780822236582,-1.16355310143397,-4.4619234807627));
#27122=CARTESIAN_POINT('Ctrl Pts',(96.2726683455444,-1.1626915064229,-4.46229125262517));
#27123=CARTESIAN_POINT('Ctrl Pts',(96.2613929450991,-1.16081626993552,-4.46306056958167));
#27124=CARTESIAN_POINT('Ctrl Pts',(96.2555327056261,-1.15979595668282,-4.46346231389843));
#27125=CARTESIAN_POINT('Ctrl Pts',(96.2402641362235,-1.15701824567792,-4.46451413480269));
#27126=CARTESIAN_POINT('Ctrl Pts',(96.2308692153122,-1.15519050715775,-4.46516639820493));
#27127=CARTESIAN_POINT('Ctrl Pts',(96.1913428258655,-1.14699961076327,-4.46793268923841));
#27128=CARTESIAN_POINT('Ctrl Pts',(96.1614471385815,-1.13957093472753,-4.47007975837751));
#27129=CARTESIAN_POINT('Ctrl Pts',(96.0519711435078,-1.1077631095234,-4.47815196254911));
#27130=CARTESIAN_POINT('Ctrl Pts',(95.9747568183585,-1.0761449966183,-4.48428507505218));
#27131=CARTESIAN_POINT('Ctrl Pts',(95.8555775850517,-1.0118856500779,-4.49419670799488));
#27132=CARTESIAN_POINT('Ctrl Pts',(95.8113170751539,-0.984077342442661,
-4.49798450104213));
#27133=CARTESIAN_POINT('Ctrl Pts',(95.7634106201733,-0.94933473665084,-4.50210051372358));
#27134=CARTESIAN_POINT('Ctrl Pts',(95.7578134929777,-0.945199416861917,
-4.50258162884902));
#27135=CARTESIAN_POINT('Ctrl Pts',(95.7493275472846,-0.938812712197127,
-4.50331099849869));
#27136=CARTESIAN_POINT('Ctrl Pts',(95.7464121476213,-0.936597147745537,
-4.50356156673596));
#27137=CARTESIAN_POINT('Ctrl Pts',(95.741093650821,-0.932516075513854,-4.5040185803336));
#27138=CARTESIAN_POINT('Ctrl Pts',(95.7386874388978,-0.93065484745509,-4.50422530171658));
#27139=CARTESIAN_POINT('Ctrl Pts',(95.7332713034991,-0.926431772992456,
-4.50469053362215));
#27140=CARTESIAN_POINT('Ctrl Pts',(95.7302656589297,-0.924064570090515,
-4.50494866600544));
#27141=CARTESIAN_POINT('Ctrl Pts',(95.7225266572997,-0.917908103654629,
-4.50561335237244));
#27142=CARTESIAN_POINT('Ctrl Pts',(95.7178108600713,-0.914096803526146,
-4.50601842242882));
#27143=CARTESIAN_POINT('Ctrl Pts',(95.6863447999047,-0.888261722910321,
-4.50872314023797));
#27144=CARTESIAN_POINT('Ctrl Pts',(95.6605454706052,-0.865100804245516,
-4.51095021651394));
#27145=CARTESIAN_POINT('Ctrl Pts',(95.6156696949907,-0.821087240804572,
-4.51492199762463));
#27146=CARTESIAN_POINT('Ctrl Pts',(95.5962515941291,-0.800623541267971,
-4.51667793852155));
#27147=CARTESIAN_POINT('Ctrl Pts',(95.545853186944,-0.74353883393383,-4.52139933902527));
#27148=CARTESIAN_POINT('Ctrl Pts',(95.5163452324756,-0.705692282249907,
-4.52434784306921));
#27149=CARTESIAN_POINT('Ctrl Pts',(95.4590437540472,-0.622146425964342,
-4.53068303098925));
#27150=CARTESIAN_POINT('Ctrl Pts',(95.4318903058464,-0.576144802910152,
-4.5340751677861));
#27151=CARTESIAN_POINT('Ctrl Pts',(95.4030896757561,-0.518783305602544,
-4.53829370492658));
#27152=CARTESIAN_POINT('Ctrl Pts',(95.3983626212747,-0.509035429050284,
-4.53901005972738));
#27153=CARTESIAN_POINT('Ctrl Pts',(95.3911330082118,-0.493587651021954,
-4.5401451515588));
#27154=CARTESIAN_POINT('Ctrl Pts',(95.3885399397014,-0.487930587054474,
-4.54056079807132));
#27155=CARTESIAN_POINT('Ctrl Pts',(95.383769154985,-0.477300995120827,-4.54134187062565));
#27156=CARTESIAN_POINT('Ctrl Pts',(95.381580740406,-0.472333426212919,-4.54170692257745));
#27157=CARTESIAN_POINT('Ctrl Pts',(95.3767582149237,-0.461178188369389,
-4.54252684688482));
#27158=CARTESIAN_POINT('Ctrl Pts',(95.3741426218582,-0.454982770572812,
-4.54298232702065));
#27159=CARTESIAN_POINT('Ctrl Pts',(95.3676220450393,-0.439161006106172,
-4.54414596848129));
#27160=CARTESIAN_POINT('Ctrl Pts',(95.3637911710571,-0.429504938528318,
-4.54485655995583));
#27161=CARTESIAN_POINT('Ctrl Pts',(95.333194912088,-0.349305056106681,-4.55076339538371));
#27162=CARTESIAN_POINT('Ctrl Pts',(95.3131424443414,-0.27640243780273,-4.55618119939496));
#27163=CARTESIAN_POINT('Ctrl Pts',(95.2902843587849,-0.145169035259185,
-4.56592568141551));
#27164=CARTESIAN_POINT('Ctrl Pts',(95.284571674238,-0.0875884456413804,
-4.57019350228826));
#27165=CARTESIAN_POINT('Ctrl Pts',(95.282588917164,-0.0093047954862436,
-4.57584854251918));
#27166=CARTESIAN_POINT('Ctrl Pts',(95.2826055807556,0.0112220653214549,
-4.57731713905188));
#27167=CARTESIAN_POINT('Ctrl Pts',(95.2835107354156,0.0447975927934336,
-4.57968597059511));
#27168=CARTESIAN_POINT('Ctrl Pts',(95.28408002885,0.0578499656139854,-4.58059857526384));
#27169=CARTESIAN_POINT('Ctrl Pts',(95.2851495262588,0.0755859247006364,
-4.58182506206358));
#27170=CARTESIAN_POINT('Ctrl Pts',(95.2854607761377,0.0802793905693871,
-4.5821483302139));
#27171=CARTESIAN_POINT('Ctrl Pts',(95.2860290187556,0.0881350586497589,
-4.58268708816283));
#27172=CARTESIAN_POINT('Ctrl Pts',(95.2862706821197,0.0912982746195974,
-4.58290339994693));
#27173=CARTESIAN_POINT('Ctrl Pts',(95.2867542498045,0.0973080551311807,
-4.58331312787679));
#27174=CARTESIAN_POINT('Ctrl Pts',(95.2869937335371,0.100154768164082,-4.583506679955));
#27175=CARTESIAN_POINT('Ctrl Pts',(95.2875878982213,0.106922651816111,-4.58396564238258));
#27176=CARTESIAN_POINT('Ctrl Pts',(95.2879518909175,0.110843001998878,-4.58423054482192));
#27177=CARTESIAN_POINT('Ctrl Pts',(95.2893108424806,0.124722992397453,-4.58516528074529));
#27178=CARTESIAN_POINT('Ctrl Pts',(95.2904131288713,0.13467203057951,-4.58582953972797));
#27179=CARTESIAN_POINT('Ctrl Pts',(95.2993739978702,0.207101918053159,-4.59063133904514));
#27180=CARTESIAN_POINT('Ctrl Pts',(95.3121067829252,0.268885518810642,-4.59454535885249));
#27181=CARTESIAN_POINT('Ctrl Pts',(95.3471684112106,0.38925873646743,-4.60230755711784));
#27182=CARTESIAN_POINT('Ctrl Pts',(95.3693456094675,0.447672079174441,-4.60614556528667));
#27183=CARTESIAN_POINT('Ctrl Pts',(95.4112738234477,0.536214320762865,-4.61236555844668));
#27184=CARTESIAN_POINT('Ctrl Pts',(95.4279521566382,0.56766654011599,-4.61466006267309));
#27185=CARTESIAN_POINT('Ctrl Pts',(95.4509530069537,0.606664986294496,-4.61764306619461));
#27186=CARTESIAN_POINT('Ctrl Pts',(95.4559814662184,0.614955161970502,-4.61828539210684));
#27187=CARTESIAN_POINT('Ctrl Pts',(95.4642734694365,0.628252677811625,-4.61932954803901));
#27188=CARTESIAN_POINT('Ctrl Pts',(95.4674738454123,0.633299028515112,-4.61972908194516));
#27189=CARTESIAN_POINT('Ctrl Pts',(95.473679108493,0.642920796603565,-4.62049729839353));
#27190=CARTESIAN_POINT('Ctrl Pts',(95.4766777700103,0.647500059005047,-4.62086574499462));
#27191=CARTESIAN_POINT('Ctrl Pts',(95.4835991262727,0.657910598658043,-4.62170996432585));
#27192=CARTESIAN_POINT('Ctrl Pts',(95.4875422818925,0.663727954623449,-4.62218648836277));
#27193=CARTESIAN_POINT('Ctrl Pts',(95.5001825439267,0.682021499083477,-4.62370042877183));
#27194=CARTESIAN_POINT('Ctrl Pts',(95.5090690636578,0.694364269649437,-4.62474491069148));
#27195=CARTESIAN_POINT('Ctrl Pts',(95.5699501598089,0.775560421020918,-4.63177485300641));
#27196=CARTESIAN_POINT('Ctrl Pts',(95.629127894075,0.83868102583114,-4.63804598630359));
#27197=CARTESIAN_POINT('Ctrl Pts',(95.7321239454832,0.926835401469966,-4.64799537611612));
#27198=CARTESIAN_POINT('Ctrl Pts',(95.7715752031079,0.956523488697504,-4.65161801347587));
#27199=CARTESIAN_POINT('Ctrl Pts',(95.8257328350741,0.99218478542195,-4.65626278907697));
#27200=CARTESIAN_POINT('Ctrl Pts',(95.8388600005971,1.00046152448989,-4.65736474698867));
#27201=CARTESIAN_POINT('Ctrl Pts',(95.8612552849237,1.01397080836982,-4.65920035201054));
#27202=CARTESIAN_POINT('Ctrl Pts',(95.8704374474205,1.01934139656302,-4.65994073574979));
#27203=CARTESIAN_POINT('Ctrl Pts',(95.8834681120871,1.02672785761334,-4.66097304730748));
#27204=CARTESIAN_POINT('Ctrl Pts',(95.8872566056097,1.02884778330312,-4.66127101985226));
#27205=CARTESIAN_POINT('Ctrl Pts',(95.8937732886332,1.03244715118033,-4.66177976852051));
#27206=CARTESIAN_POINT('Ctrl Pts',(95.8964957396692,1.03393683408772,-4.66199117583912));
#27207=CARTESIAN_POINT('Ctrl Pts',(95.9021782187256,1.03701707508994,-4.66243004923524));
#27208=CARTESIAN_POINT('Ctrl Pts',(95.9051391973361,1.0386057443689,-4.66265739947779));
#27209=CARTESIAN_POINT('Ctrl Pts',(95.9126560784275,1.04259747894743,-4.66323129406324));
#27210=CARTESIAN_POINT('Ctrl Pts',(95.9172210732586,1.04498339778935,-4.66357679554692));
#27211=CARTESIAN_POINT('Ctrl Pts',(95.921801673072,1.04733934308038,-4.66392061240651));
#27212=CARTESIAN_POINT('Origin',(96.460480949577,-7.19464945638997E-16,
0.924367114736168));
#27213=CARTESIAN_POINT('',(95.921801349668,1.04733917674356,-5.26198394263683));
#27214=CARTESIAN_POINT('',(95.9218017437159,1.04733937941474,-5.16217169173788));
#27215=CARTESIAN_POINT('',(95.9218016730721,1.04733934308042,0.924367114736168));
#27216=CARTESIAN_POINT('',(97.6382308254874,0.000540641388559765,-4.92534013812095));
#27217=CARTESIAN_POINT('Ctrl Pts',(95.921801349668,1.04733917674357,-5.26198394263684));
#27218=CARTESIAN_POINT('Ctrl Pts',(95.8863949474338,1.02912854640219,-5.25949681132839));
#27219=CARTESIAN_POINT('Ctrl Pts',(95.8519052197883,1.00911906816238,-5.25697856025019));
#27220=CARTESIAN_POINT('Ctrl Pts',(95.8012871418023,0.976206235024907,-5.25307639562409));
#27221=CARTESIAN_POINT('Ctrl Pts',(95.7844007619948,0.964588299927166,-5.25173772463044));
#27222=CARTESIAN_POINT('Ctrl Pts',(95.7611771527045,0.947700829467667,-5.24983910458976));
#27223=CARTESIAN_POINT('Ctrl Pts',(95.7545784186168,0.942795987258968,-5.24929290723313));
#27224=CARTESIAN_POINT('Ctrl Pts',(95.7439732518351,0.934739406751148,-5.24840381804272));
#27225=CARTESIAN_POINT('Ctrl Pts',(95.7399348994296,0.931629984322131,-5.24806256718612));
#27226=CARTESIAN_POINT('Ctrl Pts',(95.7315359121621,0.925075713708643,-5.24734709620885));
#27227=CARTESIAN_POINT('Ctrl Pts',(95.7271792314717,0.921626026146741,-5.246972692029));
#27228=CARTESIAN_POINT('Ctrl Pts',(95.7168700304592,0.913343664411881,-5.24607879522826));
#27229=CARTESIAN_POINT('Ctrl Pts',(95.7109400305796,0.908483491477129,-5.2455582200061));
#27230=CARTESIAN_POINT('Ctrl Pts',(95.6908969574289,0.891726553748058,-5.2437764394318));
#27231=CARTESIAN_POINT('Ctrl Pts',(95.6770169091999,0.879556591911642,-5.2425043028009));
#27232=CARTESIAN_POINT('Ctrl Pts',(95.6120262097248,0.81981379811033,-5.23635773731462));
#27233=CARTESIAN_POINT('Ctrl Pts',(95.5649349053213,0.768091508187358,-5.23131133852742));
#27234=CARTESIAN_POINT('Ctrl Pts',(95.4755240763808,0.650413370964499,-5.22048397740461));
#27235=CARTESIAN_POINT('Ctrl Pts',(95.4346229773269,0.583776441392637,-5.21471180321565));
#27236=CARTESIAN_POINT('Ctrl Pts',(95.3965003090428,0.505102965199593,-5.20858970277224));
#27237=CARTESIAN_POINT('Ctrl Pts',(95.3924940058633,0.496575986991457,-5.20793492514289));
#27238=CARTESIAN_POINT('Ctrl Pts',(95.3870003333577,0.484509188270785,-5.20702150567266));
#27239=CARTESIAN_POINT('Ctrl Pts',(95.3854274190753,0.481009037863543,-5.20675810003064));
#27240=CARTESIAN_POINT('Ctrl Pts',(95.3826092790025,0.474655051933135,-5.20628280122511));
#27241=CARTESIAN_POINT('Ctrl Pts',(95.3813582115873,0.471803850906519,-5.20607056465033));
#27242=CARTESIAN_POINT('Ctrl Pts',(95.3788145854194,0.465943840074813,-5.20563654197352));
#27243=CARTESIAN_POINT('Ctrl Pts',(95.37752324603,0.462934550930948,-5.2054148284205));
#27244=CARTESIAN_POINT('Ctrl Pts',(95.3742226322402,0.4551535304282,-5.20484446706169));
#27245=CARTESIAN_POINT('Ctrl Pts',(95.3722322147991,0.450373802485238,-5.20449692444453));
#27246=CARTESIAN_POINT('Ctrl Pts',(95.3638671871024,0.429907002987363,-5.203020109879));
#27247=CARTESIAN_POINT('Ctrl Pts',(95.3577993939736,0.414095682871752,-5.20190759531882));
#27248=CARTESIAN_POINT('Ctrl Pts',(95.342006432324,0.370130669177825,-5.19887730198996));
#27249=CARTESIAN_POINT('Ctrl Pts',(95.3330044858246,0.34172947262847,-5.19698987751931));
#27250=CARTESIAN_POINT('Ctrl Pts',(95.2983321117703,0.215963392391423,-5.18881499321327));
#27251=CARTESIAN_POINT('Ctrl Pts',(95.2841303589861,0.115885999306558,-5.18274298776355));
#27252=CARTESIAN_POINT('Ctrl Pts',(95.282520897245,-0.0086415898098256,
-5.17473148115871));
#27253=CARTESIAN_POINT('Ctrl Pts',(95.2829378364975,-0.0325062091223059,
-5.17317787910972));
#27254=CARTESIAN_POINT('Ctrl Pts',(95.2844965378622,-0.0650522509333797,
-5.17102619768557));
#27255=CARTESIAN_POINT('Ctrl Pts',(95.2850105145556,-0.0737589423348358,
-5.17044737673944));
#27256=CARTESIAN_POINT('Ctrl Pts',(95.2859844824655,-0.0876358593066876,
-5.16951937834214));
#27257=CARTESIAN_POINT('Ctrl Pts',(95.2863820398042,-0.0928102564561942,
-5.16917213567926));
#27258=CARTESIAN_POINT('Ctrl Pts',(95.2872710256096,-0.103458903315663,
-5.16845494886006));
#27259=CARTESIAN_POINT('Ctrl Pts',(95.2877666015458,-0.108932669734362,
-5.16808488471937));
#27260=CARTESIAN_POINT('Ctrl Pts',(95.2890095689832,-0.121668228612362,
-5.16722050295995));
#27261=CARTESIAN_POINT('Ctrl Pts',(95.2897861941,-0.128926873651446,-5.16672529112122));
#27262=CARTESIAN_POINT('Ctrl Pts',(95.2925136765484,-0.152357637371185,
-5.16511822866275));
#27263=CARTESIAN_POINT('Ctrl Pts',(95.2947325017154,-0.168496026239607,
-5.16399814703587));
#27264=CARTESIAN_POINT('Ctrl Pts',(95.3007711502575,-0.206550169858913,
-5.16132441417298));
#27265=CARTESIAN_POINT('Ctrl Pts',(95.3048784954533,-0.228413329369444,
-5.15976244206133));
#27266=CARTESIAN_POINT('Ctrl Pts',(95.3331721169167,-0.358587464523163,
-5.15030672285739));
#27267=CARTESIAN_POINT('Ctrl Pts',(95.3719441862428,-0.463132723739411,
-5.14198966251668));
#27268=CARTESIAN_POINT('Ctrl Pts',(95.4359701446762,-0.581400727260943,
-5.13234744333606));
#27269=CARTESIAN_POINT('Ctrl Pts',(95.447796071451,-0.60176300393703,-5.13068112479173));
#27270=CARTESIAN_POINT('Ctrl Pts',(95.4634080093114,-0.626878743439909,
-5.12863006279034));
#27271=CARTESIAN_POINT('Ctrl Pts',(95.466630013006,-0.631974466992667,-5.12821415461369));
#27272=CARTESIAN_POINT('Ctrl Pts',(95.47176393676,-0.639957592135436,-5.12756321656541));
#27273=CARTESIAN_POINT('Ctrl Pts',(95.4736496493511,-0.642861600067037,
-5.12732656013158));
#27274=CARTESIAN_POINT('Ctrl Pts',(95.4772312874345,-0.648324446193072,
-5.12688169258991));
#27275=CARTESIAN_POINT('Ctrl Pts',(95.4789243972829,-0.650884951832206,
-5.12667331763676));
#27276=CARTESIAN_POINT('Ctrl Pts',(95.4829137392218,-0.656867102985931,
-5.12618676808588));
#27277=CARTESIAN_POINT('Ctrl Pts',(95.4852179413447,-0.660283354173536,
-5.12590912282841));
#27278=CARTESIAN_POINT('Ctrl Pts',(95.492800225436,-0.671398697006397,-5.1250061996922));
#27279=CARTESIAN_POINT('Ctrl Pts',(95.4981520732879,-0.679047377938776,
-5.12438557778369));
#27280=CARTESIAN_POINT('Ctrl Pts',(95.5281763068772,-0.720888984611513,
-5.12098951830207));
#27281=CARTESIAN_POINT('Ctrl Pts',(95.5545828511405,-0.753805209553397,
-5.11831370604711));
#27282=CARTESIAN_POINT('Ctrl Pts',(95.591666117294,-0.795258862296566,-5.11483471483392));
#27283=CARTESIAN_POINT('Ctrl Pts',(95.6008023625744,-0.805126455067585,
-5.11399781957354));
#27284=CARTESIAN_POINT('Ctrl Pts',(95.6787449622545,-0.886468580596394,
-5.10700472735521));
#27285=CARTESIAN_POINT('Ctrl Pts',(95.7561514345742,-0.949134142475318,
-5.1009533562629));
#27286=CARTESIAN_POINT('Ctrl Pts',(95.8524205550059,-1.00873901196754,-5.09355640369785));
#27287=CARTESIAN_POINT('Ctrl Pts',(95.8644777883831,-1.01590946563433,-5.09263292055487));
#27288=CARTESIAN_POINT('Ctrl Pts',(95.8826356128607,-1.02627343980089,-5.09124500376506));
#27289=CARTESIAN_POINT('Ctrl Pts',(95.8886410817923,-1.02963176361733,-5.09078642239786));
#27290=CARTESIAN_POINT('Ctrl Pts',(95.8994485838952,-1.03555172003439,-5.08996178690195));
#27291=CARTESIAN_POINT('Ctrl Pts',(95.9042396348135,-1.03813307348434,-5.08959643952062));
#27292=CARTESIAN_POINT('Ctrl Pts',(95.9144561967008,-1.04354659109289,-5.08881773826864));
#27293=CARTESIAN_POINT('Ctrl Pts',(95.9198862203446,-1.04636984609748,-5.08840408683912));
#27294=CARTESIAN_POINT('Ctrl Pts',(95.9345641053784,-1.05385663388473,-5.08728640219269));
#27295=CARTESIAN_POINT('Ctrl Pts',(95.9438517065304,-1.05844061956436,-5.08657965300326));
#27296=CARTESIAN_POINT('Ctrl Pts',(95.9934162055791,-1.0820958808033,-5.08280949181167));
#27297=CARTESIAN_POINT('Ctrl Pts',(96.0346860376224,-1.09898989154639,-5.07967342924336));
#27298=CARTESIAN_POINT('Ctrl Pts',(96.128083675089,-1.13117121123118,-5.07258429166374));
#27299=CARTESIAN_POINT('Ctrl Pts',(96.1805136844178,-1.14527454181078,-5.06860869686611));
#27300=CARTESIAN_POINT('Ctrl Pts',(96.2934723911407,-1.16743755504154,-5.06016077701003));
#27301=CARTESIAN_POINT('Ctrl Pts',(96.3540455617583,-1.17451065872026,-5.05569937904056));
#27302=CARTESIAN_POINT('Ctrl Pts',(96.4248959008259,-1.17725479458165,-5.05072747573586));
#27303=CARTESIAN_POINT('Ctrl Pts',(96.4348975786546,-1.17751460912993,-5.05003142879462));
#27304=CARTESIAN_POINT('Ctrl Pts',(96.4488379187933,-1.17769902709576,-5.04907046552561));
#27305=CARTESIAN_POINT('Ctrl Pts',(96.4527743887818,-1.1777313652192,-5.04880012961801));
#27306=CARTESIAN_POINT('Ctrl Pts',(96.4595677311515,-1.17775311055907,-5.04833544370388));
#27307=CARTESIAN_POINT('Ctrl Pts',(96.4624245081339,-1.17775186114214,-5.04814059416617));
#27308=CARTESIAN_POINT('Ctrl Pts',(96.468454219585,-1.17772728469232,-5.04773055888914));
#27309=CARTESIAN_POINT('Ctrl Pts',(96.4716271163979,-1.17770152990905,-5.04751551425137));
#27310=CARTESIAN_POINT('Ctrl Pts',(96.479505009166,-1.17760574426296,-5.0469832895037));
#27311=CARTESIAN_POINT('Ctrl Pts',(96.484209826273,-1.17752033784881,-5.04666694381643));
#27312=CARTESIAN_POINT('Ctrl Pts',(96.501984895155,-1.17709108832297,-5.04547704469838));
#27313=CARTESIAN_POINT('Ctrl Pts',(96.5150501959939,-1.17655779289567,-5.04461320046953));
#27314=CARTESIAN_POINT('Ctrl Pts',(96.5486171539396,-1.17462727285692,-5.04241534191477));
#27315=CARTESIAN_POINT('Ctrl Pts',(96.569096604823,-1.17291089193164,-5.0410950563964));
#27316=CARTESIAN_POINT('Ctrl Pts',(96.6469300457998,-1.16433137283572,-5.03612100145978));
#27317=CARTESIAN_POINT('Ctrl Pts',(96.7037983899,-1.15378864259685,-5.03257461021558));
#27318=CARTESIAN_POINT('Ctrl Pts',(96.8326194826648,-1.11995413798603,-5.02432752590203));
#27319=CARTESIAN_POINT('Ctrl Pts',(96.9035529262069,-1.09383242625444,-5.01961666833807));
#27320=CARTESIAN_POINT('Ctrl Pts',(96.9808586597993,-1.05660307731737,-5.01398537807644));
#27321=CARTESIAN_POINT('Ctrl Pts',(96.9901597823292,-1.05197117224223,-5.01329947448174));
#27322=CARTESIAN_POINT('Ctrl Pts',(97.0053786698346,-1.04413925099332,-5.01216263762108));
#27323=CARTESIAN_POINT('Ctrl Pts',(97.0113325915872,-1.04101045448719,-5.01171416463297));
#27324=CARTESIAN_POINT('Ctrl Pts',(97.0218142541754,-1.03538722363846,-5.01091787315539));
#27325=CARTESIAN_POINT('Ctrl Pts',(97.026353022843,-1.03291363480598,-5.01057079150637));
#27326=CARTESIAN_POINT('Ctrl Pts',(97.0361164876793,-1.0275089670874,-5.00981917504025));
#27327=CARTESIAN_POINT('Ctrl Pts',(97.0413353773573,-1.02456775354864,-5.00941428929032));
#27328=CARTESIAN_POINT('Ctrl Pts',(97.0520142635072,-1.01844163024283,-5.00857926842199));
#27329=CARTESIAN_POINT('Ctrl Pts',(97.0574715036771,-1.01525232888928,-5.00814898620579));
#27330=CARTESIAN_POINT('Ctrl Pts',(97.0710447434838,-1.00717262621326,-5.00706973108455));
#27331=CARTESIAN_POINT('Ctrl Pts',(97.0791277719823,-1.00222799076971,-5.00641883479909));
#27332=CARTESIAN_POINT('Ctrl Pts',(97.1018766351386,-0.987931758311911,
-5.00456324447949));
#27333=CARTESIAN_POINT('Ctrl Pts',(97.1163956911033,-0.978352381338273,
-5.00335052409774));
#27334=CARTESIAN_POINT('Ctrl Pts',(97.1656109530749,-0.944293155305185,
-4.99913971703986));
#27335=CARTESIAN_POINT('Ctrl Pts',(97.1991896560734,-0.918262865612945,
-4.99608937971528));
#27336=CARTESIAN_POINT('Ctrl Pts',(97.2780930069972,-0.849963469299813,
-4.9884963204906));
#27337=CARTESIAN_POINT('Ctrl Pts',(97.3216303845538,-0.805821814943679,
-4.98391829555737));
#27338=CARTESIAN_POINT('Ctrl Pts',(97.3706501988728,-0.747588828411519,
-4.97838655316168));
#27339=CARTESIAN_POINT('Ctrl Pts',(97.3796070088654,-0.736549001064288,
-4.9773584794489));
#27340=CARTESIAN_POINT('Ctrl Pts',(97.4036155383651,-0.705836822745895,
-4.97455942836815));
#27341=CARTESIAN_POINT('Ctrl Pts',(97.4182510799551,-0.685846234172395,
-4.9728040077675));
#27342=CARTESIAN_POINT('Ctrl Pts',(97.4356676152608,-0.660411006653339,
-4.97066528858081));
#27343=CARTESIAN_POINT('Ctrl Pts',(97.4390503265042,-0.655388212501684,
-4.97024740590606));
#27344=CARTESIAN_POINT('Ctrl Pts',(97.4443288332128,-0.647418472827872,
-4.96959162340487));
#27345=CARTESIAN_POINT('Ctrl Pts',(97.4462504189586,-0.644488860366185,
-4.96935209833419));
#27346=CARTESIAN_POINT('Ctrl Pts',(97.4496588929402,-0.639241457663262,
-4.96892586616344));
#27347=CARTESIAN_POINT('Ctrl Pts',(97.4511507225163,-0.636927033532626,
-4.96873884162254));
#27348=CARTESIAN_POINT('Ctrl Pts',(97.4547217537303,-0.631344035892799,
-4.96828999097046));
#27349=CARTESIAN_POINT('Ctrl Pts',(97.4567929624061,-0.628070412027001,
-4.96802868666455));
#27350=CARTESIAN_POINT('Ctrl Pts',(97.4630960970019,-0.61799842535261,-4.96723029048899));
#27351=CARTESIAN_POINT('Ctrl Pts',(97.4672749771739,-0.611166902101886,
-4.96669648583553));
#27352=CARTESIAN_POINT('Ctrl Pts',(97.4768708747801,-0.595114223770564,
-4.96545877901235));
#27353=CARTESIAN_POINT('Ctrl Pts',(97.4822327025247,-0.585860727820751,
-4.96475792286878));
#27354=CARTESIAN_POINT('Ctrl Pts',(97.5007237189864,-0.552922520800517,
-4.96230274421573));
#27355=CARTESIAN_POINT('Ctrl Pts',(97.5131621147691,-0.528858107079123,
-4.96058015464498));
#27356=CARTESIAN_POINT('Ctrl Pts',(97.5670866081688,-0.415074449010268,
-4.95266338362854));
#27357=CARTESIAN_POINT('Ctrl Pts',(97.5980022321457,-0.320794307986144,
-4.9467107817822));
#27358=CARTESIAN_POINT('Ctrl Pts',(97.6221910474631,-0.195795567192737,
-4.93856790084562));
#27359=CARTESIAN_POINT('Ctrl Pts',(97.6265856949111,-0.167647763682192,
-4.93672154156754));
#27360=CARTESIAN_POINT('Ctrl Pts',(97.6310567883002,-0.130130150370132,
-4.93422998123106));
#27361=CARTESIAN_POINT('Ctrl Pts',(97.6320483631002,-0.12087777970812,-4.9336131097182));
#27362=CARTESIAN_POINT('Ctrl Pts',(97.6334884652477,-0.105750341674214,
-4.93260015605715));
#27363=CARTESIAN_POINT('Ctrl Pts',(97.6340027370177,-0.0998818244306157,
-4.93220611905824));
#27364=CARTESIAN_POINT('Ctrl Pts',(97.6348892665153,-0.0888108647380515,
-4.93146063662626));
#27365=CARTESIAN_POINT('Ctrl Pts',(97.6352710356966,-0.0836093095477796,
-4.9311094952366));
#27366=CARTESIAN_POINT('Ctrl Pts',(97.6359741471251,-0.0730711092015981,
-4.93039622912685));
#27367=CARTESIAN_POINT('Ctrl Pts',(97.6362937254813,-0.0677344732917057,
-4.93003405828905));
#27368=CARTESIAN_POINT('Ctrl Pts',(97.6370681607453,-0.0531372016219196,
-4.92904068274541));
#27369=CARTESIAN_POINT('Ctrl Pts',(97.6374500051863,-0.0438732412298451,
-4.92840724397924));
#27370=CARTESIAN_POINT('Ctrl Pts',(97.6380667310664,-0.0228931782140255,
-4.9269655944772));
#27371=CARTESIAN_POINT('Ctrl Pts',(97.638236204125,-0.011176348649317,-4.92615545629199));
#27372=CARTESIAN_POINT('Ctrl Pts',(97.6382308254874,0.000540641388559765,
-4.92534013812095));
#27373=CARTESIAN_POINT('Ctrl Pts',(97.6382308259868,0.000539552390703118,
-4.92534021389806));
#27374=CARTESIAN_POINT('Ctrl Pts',(97.6381825996176,0.105809404331348,-4.91801509121512));
#27375=CARTESIAN_POINT('Ctrl Pts',(97.6240200727271,0.210588653155426,-4.91024330285112));
#27376=CARTESIAN_POINT('Ctrl Pts',(97.5846280733161,0.353940616701876,-4.89938094608901));
#27377=CARTESIAN_POINT('Ctrl Pts',(97.5708137622644,0.395148756127041,-4.89623916600129));
#27378=CARTESIAN_POINT('Ctrl Pts',(97.551252259339,0.444300184375672,-4.89253604397674));
#27379=CARTESIAN_POINT('Ctrl Pts',(97.5476451622415,0.453054845377181,-4.89187827616222));
#27380=CARTESIAN_POINT('Ctrl Pts',(97.542307919798,0.465577751964426,-4.89094096264452));
#27381=CARTESIAN_POINT('Ctrl Pts',(97.540662957022,0.469381581150236,-4.89065673304485));
#27382=CARTESIAN_POINT('Ctrl Pts',(97.5377633647082,0.475990654213664,-4.89016382484868));
#27383=CARTESIAN_POINT('Ctrl Pts',(97.5365177854713,0.478799784392014,-4.88995461710823));
#27384=CARTESIAN_POINT('Ctrl Pts',(97.5338503969027,0.484752508857821,-4.88951195641959));
#27385=CARTESIAN_POINT('Ctrl Pts',(97.5324257593637,0.487894753852724,-4.88927867547932));
#27386=CARTESIAN_POINT('Ctrl Pts',(97.5284974460808,0.496458951539987,-4.88864379918167));
#27387=CARTESIAN_POINT('Ctrl Pts',(97.5259662644863,0.501868284315993,-4.88824382162014));
#27388=CARTESIAN_POINT('Ctrl Pts',(97.5135433144474,0.527899433068322,-4.88632287042263));
#27389=CARTESIAN_POINT('Ctrl Pts',(97.503092687984,0.548250931473133,-4.88483274675239));
#27390=CARTESIAN_POINT('Ctrl Pts',(97.4425272916067,0.658191394000198,-4.87677759668569));
#27391=CARTESIAN_POINT('Ctrl Pts',(97.3814564194461,0.741241479014468,-4.87063628108073));
#27392=CARTESIAN_POINT('Ctrl Pts',(97.2914426349604,0.835072740120318,-4.86242727616788));
#27393=CARTESIAN_POINT('Ctrl Pts',(97.2718185350027,0.854151608082793,-4.86068095991212));
#27394=CARTESIAN_POINT('Ctrl Pts',(97.2419392730528,0.881241284186539,-4.85806730035447));
#27395=CARTESIAN_POINT('Ctrl Pts',(97.2321867356845,0.88979406127399,-4.85722093424411));
#27396=CARTESIAN_POINT('Ctrl Pts',(97.2163846722061,0.903196928110292,-4.85585868697372));
#27397=CARTESIAN_POINT('Ctrl Pts',(97.2104249034407,0.908151523832824,-4.85534692716612));
#27398=CARTESIAN_POINT('Ctrl Pts',(97.1991921130397,0.917303820166746,-4.85438580159248));
#27399=CARTESIAN_POINT('Ctrl Pts',(97.1939310938734,0.921515797038926,-4.8539370202997));
#27400=CARTESIAN_POINT('Ctrl Pts',(97.1844741014515,0.928954786245003,-4.85313257649093));
#27401=CARTESIAN_POINT('Ctrl Pts',(97.1802919430436,0.932199126246907,-4.85277760619345));
#27402=CARTESIAN_POINT('Ctrl Pts',(97.1714469397591,0.938965691794266,-4.85202841062739));
#27403=CARTESIAN_POINT('Ctrl Pts',(97.1667794777384,0.942481616032628,-4.85163395400226));
#27404=CARTESIAN_POINT('Ctrl Pts',(97.1547887149101,0.951374970894183,-4.85062273168189));
#27405=CARTESIAN_POINT('Ctrl Pts',(97.1474291130166,0.956702577070535,-4.8500040838758));
#27406=CARTESIAN_POINT('Ctrl Pts',(97.1182931628985,0.977284525055812,-4.8475622054245));
#27407=CARTESIAN_POINT('Ctrl Pts',(97.0960659652995,0.991883784928601,-4.84571487321962));
#27408=CARTESIAN_POINT('Ctrl Pts',(96.9903440454676,1.05631073253277,-4.83699276730838));
#27409=CARTESIAN_POINT('Ctrl Pts',(96.9013855576243,1.09642365897743,-4.82979275792665));
#27410=CARTESIAN_POINT('Ctrl Pts',(96.7801085359821,1.13393938001223,-4.82053466748179));
#27411=CARTESIAN_POINT('Ctrl Pts',(96.7513593237808,1.14165245180465,-4.81838219493692));
#27412=CARTESIAN_POINT('Ctrl Pts',(96.7058486639721,1.15203129344284,-4.81506803314242));
#27413=CARTESIAN_POINT('Ctrl Pts',(96.6892700015894,1.15543803788808,-4.81387986422216));
#27414=CARTESIAN_POINT('Ctrl Pts',(96.6675310453554,1.15941886915581,-4.81235152599497));
#27415=CARTESIAN_POINT('Ctrl Pts',(96.6624332246221,1.16031768813986,-4.81199524599042));
#27416=CARTESIAN_POINT('Ctrl Pts',(96.6541012470027,1.16173015981304,-4.81141656756626));
#27417=CARTESIAN_POINT('Ctrl Pts',(96.6508706489711,1.16226397467406,-4.81119308306013));
#27418=CARTESIAN_POINT('Ctrl Pts',(96.6445636517208,1.16327912239248,-4.81075856970003));
#27419=CARTESIAN_POINT('Ctrl Pts',(96.6414875142851,1.16376173750699,-4.81054747530442));
#27420=CARTESIAN_POINT('Ctrl Pts',(96.6346156506074,1.16481195805586,-4.81007769327211));
#27421=CARTESIAN_POINT('Ctrl Pts',(96.6308189547716,1.16537322637189,-4.80981935410606));
#27422=CARTESIAN_POINT('Ctrl Pts',(96.6176900749443,1.16724854583192,-4.80893000661741));
#27423=CARTESIAN_POINT('Ctrl Pts',(96.6083446125399,1.16846918133681,-4.80830389146124));
#27424=CARTESIAN_POINT('Ctrl Pts',(96.5216064622259,1.17874092259645,-4.80254857468887));
#27425=CARTESIAN_POINT('Ctrl Pts',(96.4434976580434,1.18020405445402,-4.79776875738766));
#27426=CARTESIAN_POINT('Ctrl Pts',(96.3116099222756,1.16956786298637,-4.78958234826573));
#27427=CARTESIAN_POINT('Ctrl Pts',(96.2577827761113,1.16144926411757,-4.78620904856263));
#27428=CARTESIAN_POINT('Ctrl Pts',(96.1849318684126,1.1452416328441,-4.7814441130559));
#27429=CARTESIAN_POINT('Ctrl Pts',(96.1652692377537,1.14033138513873,-4.78013804928604));
#27430=CARTESIAN_POINT('Ctrl Pts',(96.1311297363394,1.13086375793522,-4.77782810874798));
#27431=CARTESIAN_POINT('Ctrl Pts',(96.1165958225777,1.12652920334162,-4.77683109983049));
#27432=CARTESIAN_POINT('Ctrl Pts',(96.0953900374026,1.11975624565842,-4.7753543743319));
#27433=CARTESIAN_POINT('Ctrl Pts',(96.0886496781884,1.11753609595964,-4.77488168766651));
#27434=CARTESIAN_POINT('Ctrl Pts',(96.0767526897184,1.11349790160669,-4.77404131980248));
#27435=CARTESIAN_POINT('Ctrl Pts',(96.0715878386512,1.11170459244003,-4.77367445306594));
#27436=CARTESIAN_POINT('Ctrl Pts',(96.0607805295306,1.10786761362216,-4.77290242003057));
#27437=CARTESIAN_POINT('Ctrl Pts',(96.0551408451198,1.10581665411519,-4.77249702352789));
#27438=CARTESIAN_POINT('Ctrl Pts',(96.0403229510976,1.10029931026965,-4.77142508551925));
#27439=CARTESIAN_POINT('Ctrl Pts',(96.031172117544,1.09676124681055,-4.77075620061471));
#27440=CARTESIAN_POINT('Ctrl Pts',(95.991448503128,1.08082926811975,-4.76782157783471));
#27441=CARTESIAN_POINT('Ctrl Pts',(95.9613625562976,1.0672693211444,-4.76551759496211));
#27442=CARTESIAN_POINT('Ctrl Pts',(95.9285169888683,1.05077287490871,-4.76290853512532));
#27443=CARTESIAN_POINT('Ctrl Pts',(95.9251549404675,1.04906403309099,-4.76264035901828));
#27444=CARTESIAN_POINT('Ctrl Pts',(95.9218016616992,1.04733933723097,-4.76237177033706));
#27445=CARTESIAN_POINT('Ctrl Pts',(95.921801673072,1.04733934308038,-4.66392061240651));
#27446=CARTESIAN_POINT('Ctrl Pts',(95.9221705646186,1.04752907550354,-4.66394830116743));
#27447=CARTESIAN_POINT('Ctrl Pts',(95.9225395573735,1.04771861352914,-4.66397597900242));
#27448=CARTESIAN_POINT('Ctrl Pts',(95.9395117997437,1.05642530124754,-4.66524820462356));
#27449=CARTESIAN_POINT('Ctrl Pts',(95.9563161643211,1.06454743235825,-4.66647055066501));
#27450=CARTESIAN_POINT('Ctrl Pts',(96.0707824950419,1.1165540077375,-4.67459565258095));
#27451=CARTESIAN_POINT('Ctrl Pts',(96.1738488912569,1.14734691528063,-4.68098157065748));
#27452=CARTESIAN_POINT('Ctrl Pts',(96.3210300509534,1.17021395041679,-4.69038080141231));
#27453=CARTESIAN_POINT('Ctrl Pts',(96.3627019195113,1.17443003821052,-4.69306605453373));
#27454=CARTESIAN_POINT('Ctrl Pts',(96.4146735100156,1.17690285932458,-4.69649042384808));
#27455=CARTESIAN_POINT('Ctrl Pts',(96.4248459551064,1.17725477205649,-4.69716416865052));
#27456=CARTESIAN_POINT('Ctrl Pts',(96.4411008831706,1.17760623834006,-4.69824691702232));
#27457=CARTESIAN_POINT('Ctrl Pts',(96.4471811664844,1.17769060154973,-4.69865329929652));
#27458=CARTESIAN_POINT('Ctrl Pts',(96.4587102597247,1.17776127236764,-4.69942658239779));
#27459=CARTESIAN_POINT('Ctrl Pts',(96.4641588700541,1.17775685997684,-4.69979318661607));
#27460=CARTESIAN_POINT('Ctrl Pts',(96.4765522646717,1.17766082234335,-4.70062977949987));
#27461=CARTESIAN_POINT('Ctrl Pts',(96.4834966093245,1.17754557257178,-4.7011004851427));
#27462=CARTESIAN_POINT('Ctrl Pts',(96.5047994475771,1.1770035164188,-4.70255061925052));
#27463=CARTESIAN_POINT('Ctrl Pts',(96.5191510279033,1.17637544909335,-4.70353619086242));
#27464=CARTESIAN_POINT('Ctrl Pts',(96.6297028295073,1.16950938978424,-4.71119795696563));
#27465=CARTESIAN_POINT('Ctrl Pts',(96.7248036524084,1.15174412415181,-4.71824198481139));
#27466=CARTESIAN_POINT('Ctrl Pts',(96.8730652775247,1.10470433450429,-4.72965288664079));
#27467=CARTESIAN_POINT('Ctrl Pts',(96.9280526792058,1.08257827227701,-4.7339766794005));
#27468=CARTESIAN_POINT('Ctrl Pts',(96.9887551864931,1.05266011230374,-4.73870277340241));
#27469=CARTESIAN_POINT('Ctrl Pts',(96.9963215241315,1.04882880892294,-4.73929090046884));
#27470=CARTESIAN_POINT('Ctrl Pts',(97.0073631309057,1.0430870801246,-4.74014703946401));
#27471=CARTESIAN_POINT('Ctrl Pts',(97.0108709870057,1.04124040683633,-4.74041871259547));
#27472=CARTESIAN_POINT('Ctrl Pts',(97.0170383142447,1.03795380798756,-4.74089570559588));
#27473=CARTESIAN_POINT('Ctrl Pts',(97.0197016405743,1.03652131053901,-4.74110147352221));
#27474=CARTESIAN_POINT('Ctrl Pts',(97.0254751909377,1.0333872157502,-4.74154704493221));
#27475=CARTESIAN_POINT('Ctrl Pts',(97.028583266506,1.03168182535968,-4.74178660832252));
#27476=CARTESIAN_POINT('Ctrl Pts',(97.0371394048963,1.02693671105166,-4.74244539644105));
#27477=CARTESIAN_POINT('Ctrl Pts',(97.0425711850867,1.02386764014367,-4.7428628347188));
#27478=CARTESIAN_POINT('Ctrl Pts',(97.0717558146544,1.00707037778058,-4.74510286148963));
#27479=CARTESIAN_POINT('Ctrl Pts',(97.0950499210339,0.992557402848831,-4.7468805895713));
#27480=CARTESIAN_POINT('Ctrl Pts',(97.1741465874145,0.939353474041304,-4.75295762864868));
#27481=CARTESIAN_POINT('Ctrl Pts',(97.2270977096641,0.896662486993835,-4.7571051882413));
#27482=CARTESIAN_POINT('Ctrl Pts',(97.3180208416616,0.80938282512673,-4.76492450685179));
#27483=CARTESIAN_POINT('Ctrl Pts',(97.3569200318188,0.766075133480703,-4.7685677265626));
#27484=CARTESIAN_POINT('Ctrl Pts',(97.4035480472587,0.705725424600364,-4.77351674610085));
#27485=CARTESIAN_POINT('Ctrl Pts',(97.4143020868223,0.691121629339043,-4.77470492971462));
#27486=CARTESIAN_POINT('Ctrl Pts',(97.4290863302964,0.670042277254638,-4.77641020172323));
#27487=CARTESIAN_POINT('Ctrl Pts',(97.4333977763163,0.663766435260243,-4.77691670134802));
#27488=CARTESIAN_POINT('Ctrl Pts',(97.4407446465999,0.652846781226984,-4.77779616247406));
#27489=CARTESIAN_POINT('Ctrl Pts',(97.4438087061145,0.648222459415354,-4.77816804538233));
#27490=CARTESIAN_POINT('Ctrl Pts',(97.4496310545137,0.639299008009149,-4.77888468482447));
#27491=CARTESIAN_POINT('Ctrl Pts',(97.4523942746596,0.635003232941863,-4.77922924875282));
#27492=CARTESIAN_POINT('Ctrl Pts',(97.4588489425677,0.624823701167232,-4.7800448168545));
#27493=CARTESIAN_POINT('Ctrl Pts',(97.462516422323,0.618925047761424,-4.78051668118401));
#27494=CARTESIAN_POINT('Ctrl Pts',(97.4733264490928,0.601190613889158,-4.78193339084917));
#27495=CARTESIAN_POINT('Ctrl Pts',(97.4803127978783,0.589261515108182,-4.78288377427852));
#27496=CARTESIAN_POINT('Ctrl Pts',(97.5278598815303,0.504696251920259,-4.78960562340895));
#27497=CARTESIAN_POINT('Ctrl Pts',(97.5608270618603,0.428076795848594,-4.79564211032697));
#27498=CARTESIAN_POINT('Ctrl Pts',(97.5927919549359,0.324935000251129,-4.80356519361236));
#27499=CARTESIAN_POINT('Ctrl Pts',(97.5993874225799,0.301003379707759,-4.80538805973982));
#27500=CARTESIAN_POINT('Ctrl Pts',(97.6156597218724,0.233726962044449,-4.8104478104215));
#27501=CARTESIAN_POINT('Ctrl Pts',(97.6236500608284,0.190012429149564,-4.81366274102418));
#27502=CARTESIAN_POINT('Ctrl Pts',(97.6303388625139,0.136451792809364,-4.81744204259469));
#27503=CARTESIAN_POINT('Ctrl Pts',(97.6314089380747,0.126942067867184,-4.81810694778348));
#27504=CARTESIAN_POINT('Ctrl Pts',(97.6327779409745,0.113279061882614,-4.8190525075962));
#27505=CARTESIAN_POINT('Ctrl Pts',(97.6331709090606,0.109135888470177,-4.81933795751664));
#27506=CARTESIAN_POINT('Ctrl Pts',(97.633816041812,0.101927816928756,-4.81983224042097));
#27507=CARTESIAN_POINT('Ctrl Pts',(97.634078176545,0.0988638876425055,-4.8200416116822));
#27508=CARTESIAN_POINT('Ctrl Pts',(97.6346081749494,0.0923696851907753,
-4.8204838051852));
#27509=CARTESIAN_POINT('Ctrl Pts',(97.6348730104365,0.0889392391256996,
-4.82071646097562));
#27510=CARTESIAN_POINT('Ctrl Pts',(97.6355533306411,0.0795934927289862,
-4.82134789939502));
#27511=CARTESIAN_POINT('Ctrl Pts',(97.635939187809,0.0736760384583882,-4.82174509330303));
#27512=CARTESIAN_POINT('Ctrl Pts',(97.637568465268,0.0454023806028048,-4.82363148964865));
#27513=CARTESIAN_POINT('Ctrl Pts',(97.6382189761102,0.0230150375271749,
-4.82509116130169));
#27514=CARTESIAN_POINT('Ctrl Pts',(97.6382560001883,-0.0471910872588473,
-4.82960001635612));
#27515=CARTESIAN_POINT('Ctrl Pts',(97.6353696927734,-0.0949642835910884,
-4.832569571209));
#27516=CARTESIAN_POINT('Ctrl Pts',(97.6188906997424,-0.230225778237202,
-4.84100497441288));
#27517=CARTESIAN_POINT('Ctrl Pts',(97.5983419198175,-0.316523842856713,
-4.84644244000345));
#27518=CARTESIAN_POINT('Ctrl Pts',(97.5632110705512,-0.413894778747374,
-4.85319261988044));
#27519=CARTESIAN_POINT('Ctrl Pts',(97.5578197198743,-0.427983874916434,
-4.85418439438245));
#27520=CARTESIAN_POINT('Ctrl Pts',(97.5495306791967,-0.448458271723652,
-4.85564975043778));
#27521=CARTESIAN_POINT('Ctrl Pts',(97.5468440687512,-0.45492780175818,-4.85611634835398));
#27522=CARTESIAN_POINT('Ctrl Pts',(97.5419569091997,-0.466406194533013,
-4.85695077095576));
#27523=CARTESIAN_POINT('Ctrl Pts',(97.5397788548255,-0.471424457941079,
-4.85731783337144));
#27524=CARTESIAN_POINT('Ctrl Pts',(97.5351441387186,-0.481902411786874,
-4.85808908413645));
#27525=CARTESIAN_POINT('Ctrl Pts',(97.5326806556856,-0.48735889498491,-4.85849349462092));
#27526=CARTESIAN_POINT('Ctrl Pts',(97.526097268077,-0.501649212625475,-4.85956007762258));
#27527=CARTESIAN_POINT('Ctrl Pts',(97.5219091843042,-0.510450941229398,
-4.86022455170116));
#27528=CARTESIAN_POINT('Ctrl Pts',(97.5016571727848,-0.551685652117717,
-4.86337403754441));
#27529=CARTESIAN_POINT('Ctrl Pts',(97.4842145716792,-0.583415781406397,
-4.86590595561628));
#27530=CARTESIAN_POINT('Ctrl Pts',(97.4317828707908,-0.669183913258349,
-4.87306172654879));
#27531=CARTESIAN_POINT('Ctrl Pts',(97.3937865131363,-0.721230667587447,
-4.8777748154155));
#27532=CARTESIAN_POINT('Ctrl Pts',(97.3123170935076,-0.815540476956679,
-4.88692064865298));
#27533=CARTESIAN_POINT('Ctrl Pts',(97.2694483699655,-0.858081727212322,
-4.89133740014115));
#27534=CARTESIAN_POINT('Ctrl Pts',(97.2158714965398,-0.903648508265781,
-4.89626953920377));
#27535=CARTESIAN_POINT('Ctrl Pts',(97.2081542385449,-0.9100440508581,-4.89696685021218));
#27536=CARTESIAN_POINT('Ctrl Pts',(97.1972910434755,-0.91881525123025,-4.89792924994538));
#27537=CARTESIAN_POINT('Ctrl Pts',(97.1942136672407,-0.9212745956056,-4.89819977908327));
#27538=CARTESIAN_POINT('Ctrl Pts',(97.1888829769944,-0.925491065832029,
-4.89866469565099));
#27539=CARTESIAN_POINT('Ctrl Pts',(97.1866355257515,-0.92725549792166,-4.89885958384979));
#27540=CARTESIAN_POINT('Ctrl Pts',(97.1818797462606,-0.930961276728047,
-4.89926957901612));
#27541=CARTESIAN_POINT('Ctrl Pts',(97.1793699562479,-0.932900701655032,
-4.89948454555573));
#27542=CARTESIAN_POINT('Ctrl Pts',(97.1731212455115,-0.937689163329424,
-4.90001637059439));
#27543=CARTESIAN_POINT('Ctrl Pts',(97.1693729946145,-0.940526038323484,
-4.90033239725096));
#27544=CARTESIAN_POINT('Ctrl Pts',(97.1551620300666,-0.951148430627917,
-4.90151977598607));
#27545=CARTESIAN_POINT('Ctrl Pts',(97.1445867757886,-0.958782766813826,
-4.90238147125986));
#27546=CARTESIAN_POINT('Ctrl Pts',(97.1170887560734,-0.977947064022778,
-4.90457261695953));
#27547=CARTESIAN_POINT('Ctrl Pts',(97.0999877150538,-0.98921457122118,-4.90588844327649));
#27548=CARTESIAN_POINT('Ctrl Pts',(97.0334950154001,-1.03057970089655,-4.91086343910632));
#27549=CARTESIAN_POINT('Ctrl Pts',(96.9822031333988,-1.05747170458792,-4.9144145201672));
#27550=CARTESIAN_POINT('Ctrl Pts',(96.8599028743865,-1.11051921516038,-4.92266891278167));
#27551=CARTESIAN_POINT('Ctrl Pts',(96.7879490157584,-1.13382241066399,-4.9273822933451));
#27552=CARTESIAN_POINT('Ctrl Pts',(96.7041214963406,-1.15232038598896,-4.93301629207463));
#27553=CARTESIAN_POINT('Ctrl Pts',(96.6939479312492,-1.15442459488227,-4.93370208235926));
#27554=CARTESIAN_POINT('Ctrl Pts',(96.6771449474128,-1.15766877894936,-4.93483874958851));
#27555=CARTESIAN_POINT('Ctrl Pts',(96.6705310950574,-1.15888706220545,-4.93528716722955));
#27556=CARTESIAN_POINT('Ctrl Pts',(96.6585605921416,-1.16098621176764,-4.93610075627695));
#27557=CARTESIAN_POINT('Ctrl Pts',(96.653207559021,-1.16188681937624,-4.93646529812694));
#27558=CARTESIAN_POINT('Ctrl Pts',(96.6417049079532,-1.16374037656825,-4.93725025606719));
#27559=CARTESIAN_POINT('Ctrl Pts',(96.6355536032837,-1.16468165199916,-4.93767102538642));
#27560=CARTESIAN_POINT('Ctrl Pts',(96.6186745240865,-1.16712775769264,-4.93882848210026));
#27561=CARTESIAN_POINT('Ctrl Pts',(96.6079332177222,-1.1685333648726,-4.93956822812783));
#27562=CARTESIAN_POINT('Ctrl Pts',(96.5441853166413,-1.17598249113657,-4.94397856460056));
#27563=CARTESIAN_POINT('Ctrl Pts',(96.4908445990453,-1.178566000117,-4.94775513492852));
#27564=CARTESIAN_POINT('Ctrl Pts',(96.3895698413714,-1.17659112237072,-4.95507632748259));
#27565=CARTESIAN_POINT('Ctrl Pts',(96.3417247429082,-1.17272826537954,-4.95859845079308));
#27566=CARTESIAN_POINT('Ctrl Pts',(96.266325107793,-1.16197860683751,-4.96418636160127));
#27567=CARTESIAN_POINT('Ctrl Pts',(96.2385503432698,-1.15699510534415,-4.96625232789598));
#27568=CARTESIAN_POINT('Ctrl Pts',(96.1771190299253,-1.14367896115836,-4.97080975736508));
#27569=CARTESIAN_POINT('Ctrl Pts',(96.1435941925275,-1.13484748863921,-4.97328875617494));
#27570=CARTESIAN_POINT('Ctrl Pts',(96.1047153041129,-1.12274780286211,-4.97611889990995));
#27571=CARTESIAN_POINT('Ctrl Pts',(96.0989399558145,-1.12090139487028,-4.97653811545212));
#27572=CARTESIAN_POINT('Ctrl Pts',(96.0895439912383,-1.11781728029376,-4.97721790299206));
#27573=CARTESIAN_POINT('Ctrl Pts',(96.0859147786827,-1.11660641402698,-4.97747992476473));
#27574=CARTESIAN_POINT('Ctrl Pts',(96.0794105199354,-1.11440102486579,-4.97794845418759));
#27575=CARTESIAN_POINT('Ctrl Pts',(96.0765333766969,-1.11341303139861,-4.97815532558996));
#27576=CARTESIAN_POINT('Ctrl Pts',(96.0702014500086,-1.11121122318567,-4.97860975893374));
#27577=CARTESIAN_POINT('Ctrl Pts',(96.0667484824984,-1.10999243943222,-4.97885702923968));
#27578=CARTESIAN_POINT('Ctrl Pts',(96.0567500249524,-1.10641078635289,-4.97957160168267));
#27579=CARTESIAN_POINT('Ctrl Pts',(96.0502195851766,-1.10400593581433,-4.98003654157876));
#27580=CARTESIAN_POINT('Ctrl Pts',(95.9948776583237,-1.08306724738804,-4.9839645841931));
#27581=CARTESIAN_POINT('Ctrl Pts',(95.9473204222118,-1.0613617790898,-4.98726110046474));
#27582=CARTESIAN_POINT('Ctrl Pts',(95.8281131971778,-0.997061343697797,
-4.99569792028873));
#27583=CARTESIAN_POINT('Ctrl Pts',(95.7592678105945,-0.9499052788285,-5.00076195123938));
#27584=CARTESIAN_POINT('Ctrl Pts',(95.6725536163826,-0.875906966767105,
-5.00803313694736));
#27585=CARTESIAN_POINT('Ctrl Pts',(95.6499337088355,-0.855017784576169,
-5.0100244756171));
#27586=CARTESIAN_POINT('Ctrl Pts',(95.6213888251713,-0.826505318896142,
-5.01268340277329));
#27587=CARTESIAN_POINT('Ctrl Pts',(95.6147012565486,-0.819660501294488,
-5.0133174869601));
#27588=CARTESIAN_POINT('Ctrl Pts',(95.6039933897057,-0.808430270196311,
-5.01435152675391));
#27589=CARTESIAN_POINT('Ctrl Pts',(95.5999215175054,-0.804094461901574,
-5.01474926867878));
#27590=CARTESIAN_POINT('Ctrl Pts',(95.5921601906039,-0.795703572831049,
-5.01551628500619));
#27591=CARTESIAN_POINT('Ctrl Pts',(95.5884658556924,-0.791653200949639,
-5.01588534000642));
#27592=CARTESIAN_POINT('Ctrl Pts',(95.5799802362742,-0.782218322710378,
-5.01674236526036));
#27593=CARTESIAN_POINT('Ctrl Pts',(95.5752098756405,-0.776815378429923,
-5.01723118327001));
#27594=CARTESIAN_POINT('Ctrl Pts',(95.5601584581916,-0.759449330161668,
-5.01879637431942));
#27595=CARTESIAN_POINT('Ctrl Pts',(95.550068384301,-0.747323753659946,-5.01988039097897));
#27596=CARTESIAN_POINT('Ctrl Pts',(95.5269154244496,-0.718335112006344,
-5.02245271275015));
#27597=CARTESIAN_POINT('Ctrl Pts',(95.5140614568668,-0.70131303199242,-5.02394851269682));
#27598=CARTESIAN_POINT('Ctrl Pts',(95.467181882569,-0.635594549512398,-5.02966955841261));
#27599=CARTESIAN_POINT('Ctrl Pts',(95.4363978618898,-0.584701522818449,
-5.03399738009116));
#27600=CARTESIAN_POINT('Ctrl Pts',(95.3778184412167,-0.468922585421363,
-5.04351618725935));
#27601=CARTESIAN_POINT('Ctrl Pts',(95.3517386823039,-0.403409055696163,
-5.04870181968));
#27602=CARTESIAN_POINT('Ctrl Pts',(95.328858353833,-0.326530297693514,-5.05432377948637));
#27603=CARTESIAN_POINT('Ctrl Pts',(95.3261717160383,-0.317071463481642,
-5.05500759914016));
#27604=CARTESIAN_POINT('Ctrl Pts',(95.3225880496707,-0.303825503523244,
-5.05595321532764));
#27605=CARTESIAN_POINT('Ctrl Pts',(95.3215909393134,-0.300066215765981,
-5.05622024740033));
#27606=CARTESIAN_POINT('Ctrl Pts',(95.3198967759879,-0.293548799547081,
-5.05668079891315));
#27607=CARTESIAN_POINT('Ctrl Pts',(95.3191910677639,-0.290792986276538,
-5.05687479788204));
#27608=CARTESIAN_POINT('Ctrl Pts',(95.3177159722246,-0.284944599169217,
-5.05728489616348));
#27609=CARTESIAN_POINT('Ctrl Pts',(95.3169491375731,-0.281851403239069,
-5.05750084454948));
#27610=CARTESIAN_POINT('Ctrl Pts',(95.3150651976784,-0.274117854075262,
-5.05803846774445));
#27611=CARTESIAN_POINT('Ctrl Pts',(95.3139637127855,-0.269473691315058,
-5.05835927056009));
#27612=CARTESIAN_POINT('Ctrl Pts',(95.309838244532,-0.251596276689614,-5.05958675967539));
#27613=CARTESIAN_POINT('Ctrl Pts',(95.3070147527344,-0.23831721032918,-5.06048292862793));
#27614=CARTESIAN_POINT('Ctrl Pts',(95.3002854599901,-0.203740526996326,
-5.0627831311805));
#27615=CARTESIAN_POINT('Ctrl Pts',(95.2967360834668,-0.182378117106677,
-5.06417177354963));
#27616=CARTESIAN_POINT('Ctrl Pts',(95.2797914601859,-0.0595327570435999,
-5.07203356250995));
#27617=CARTESIAN_POINT('Ctrl Pts',(95.279082211168,0.0432546870418731,-5.07817041039214));
#27618=CARTESIAN_POINT('Ctrl Pts',(95.2956597998526,0.177026458367084,-5.08675225369376));
#27619=CARTESIAN_POINT('Ctrl Pts',(95.3009751395235,0.209027891472727,-5.08884722088288));
#27620=CARTESIAN_POINT('Ctrl Pts',(95.309596302135,0.250309024981939,-5.09162537709721));
#27621=CARTESIAN_POINT('Ctrl Pts',(95.3117073495849,0.259825491994906,-5.09227107727238));
#27622=CARTESIAN_POINT('Ctrl Pts',(95.3153052491891,0.275142728474053,-5.0933193761027));
#27623=CARTESIAN_POINT('Ctrl Pts',(95.3167186704959,0.280960410919459,-5.09371964455285));
#27624=CARTESIAN_POINT('Ctrl Pts',(95.3195083690748,0.29207286723613,-5.09448836948864));
#27625=CARTESIAN_POINT('Ctrl Pts',(95.3208773057176,0.29736933669096,-5.09485658334345));
#27626=CARTESIAN_POINT('Ctrl Pts',(95.3241137182056,0.309540507290239,-5.09570702377823));
#27627=CARTESIAN_POINT('Ctrl Pts',(95.3260067529637,0.316408128132529,-5.09619005615569));
#27628=CARTESIAN_POINT('Ctrl Pts',(95.3321653903272,0.337984619261349,-5.09771787620785));
#27629=CARTESIAN_POINT('Ctrl Pts',(95.3366555047764,0.35262719047301,-5.0987698017193));
#27630=CARTESIAN_POINT('Ctrl Pts',(95.3478280874545,0.386678007584853,-5.10125267787087));
#27631=CARTESIAN_POINT('Ctrl Pts',(95.3547347764921,0.406006879533665,-5.1026904347257));
#27632=CARTESIAN_POINT('Ctrl Pts',(95.3822010244374,0.47696448555228,-5.10807517442894));
#27633=CARTESIAN_POINT('Ctrl Pts',(95.4058995232217,0.52729451275876,-5.1121118988069));
#27634=CARTESIAN_POINT('Ctrl Pts',(95.4702810301025,0.642181114430442,-5.12176407325156));
#27635=CARTESIAN_POINT('Ctrl Pts',(95.5138597117022,0.704842250797179,-5.12739348410932));
#27636=CARTESIAN_POINT('Ctrl Pts',(95.5693374635881,0.770096446118507,-5.13339244988422));
#27637=CARTESIAN_POINT('Ctrl Pts',(95.5755762408864,0.777257305993525,-5.13405260663785));
#27638=CARTESIAN_POINT('Ctrl Pts',(95.5844653436938,0.787214421423958,-5.13497223138542));
#27639=CARTESIAN_POINT('Ctrl Pts',(95.5870436070076,0.79007410835775,-5.13523654651609));
#27640=CARTESIAN_POINT('Ctrl Pts',(95.5917342609425,0.795225733827696,-5.13571297996965));
#27641=CARTESIAN_POINT('Ctrl Pts',(95.593841810491,0.797522024882389,-5.13592544706737));
#27642=CARTESIAN_POINT('Ctrl Pts',(95.5981784369695,0.802209527021386,-5.13635932435101));
#27643=CARTESIAN_POINT('Ctrl Pts',(95.6004083914253,0.804599865689834,-5.13658066591109));
#27644=CARTESIAN_POINT('Ctrl Pts',(95.6061787964826,0.810733891514326,-5.13714899931682));
#27645=CARTESIAN_POINT('Ctrl Pts',(95.6097339605441,0.814463734438341,-5.1374949007123));
#27646=CARTESIAN_POINT('Ctrl Pts',(95.6249205423656,0.830188551318374,-5.13895520616683));
#27647=CARTESIAN_POINT('Ctrl Pts',(95.6367826798277,0.841959295319741,-5.14005331342416));
#27648=CARTESIAN_POINT('Ctrl Pts',(95.6700492244388,0.873593239648491,-5.14303235507286));
#27649=CARTESIAN_POINT('Ctrl Pts',(95.69194876966,0.892919922577796,-5.14488416526939));
#27650=CARTESIAN_POINT('Ctrl Pts',(95.7786842299896,0.963907493491577,-5.15191236718003));
#27651=CARTESIAN_POINT('Ctrl Pts',(95.8481569370433,1.00946156563831,-5.15693593302965));
#27652=CARTESIAN_POINT('Ctrl Pts',(95.9218017437159,1.04733937941473,-5.16217169173788));
#27653=CARTESIAN_POINT('Origin',(96.460480949577,-7.19464945638997E-16,
0.924367114736168));
#27654=CARTESIAN_POINT('',(95.921801673071,1.04733934307987,-5.76048914482438));
#27655=CARTESIAN_POINT('',(95.9218018640415,1.0473394413019,-5.66223110129989));
#27656=CARTESIAN_POINT('',(95.9218016730721,1.04733934308042,0.924367114736168));
#27657=CARTESIAN_POINT('Ctrl Pts',(95.921801673071,1.04733934307989,-5.76048914482438));
#27658=CARTESIAN_POINT('Ctrl Pts',(95.9182792703783,1.04552766155889,-5.76021575466029));
#27659=CARTESIAN_POINT('Ctrl Pts',(95.9147659592519,1.04369818558514,-5.75994336455603));
#27660=CARTESIAN_POINT('Ctrl Pts',(95.9083340398797,1.04030755404686,-5.75944532432093));
#27661=CARTESIAN_POINT('Ctrl Pts',(95.9054126772423,1.03875176564439,-5.7592193566938));
#27662=CARTESIAN_POINT('Ctrl Pts',(95.8997741700574,1.03571836688476,-5.75878374118157));
#27663=CARTESIAN_POINT('Ctrl Pts',(95.8970562448979,1.03424234612522,-5.75857400405198));
#27664=CARTESIAN_POINT('Ctrl Pts',(95.8910507559638,1.03095025235945,-5.75811104399781));
#27665=CARTESIAN_POINT('Ctrl Pts',(95.8877659703997,1.02912910843476,-5.75785813547155));
#27666=CARTESIAN_POINT('Ctrl Pts',(95.8761075000208,1.02259233701673,-5.75696141955584));
#27667=CARTESIAN_POINT('Ctrl Pts',(95.8677826103802,1.01778981600199,-5.75632279569602));
#27668=CARTESIAN_POINT('Ctrl Pts',(95.7920261476623,0.972842106316879,-5.75051808766608));
#27669=CARTESIAN_POINT('Ctrl Pts',(95.7286961979165,0.926147007071749,-5.74570644331157));
#27670=CARTESIAN_POINT('Ctrl Pts',(95.630418325696,0.837262388101087,-5.73750754102063));
#27671=CARTESIAN_POINT('Ctrl Pts',(95.5929021564932,0.798322417069381,-5.73415567233252));
#27672=CARTESIAN_POINT('Ctrl Pts',(95.5452201168959,0.741485039964303,-5.72941832147816));
#27673=CARTESIAN_POINT('Ctrl Pts',(95.5326479713191,0.725691635990643,-5.72811725936082));
#27674=CARTESIAN_POINT('Ctrl Pts',(95.5113789973254,0.69751641219175,-5.7258153715045));
#27675=CARTESIAN_POINT('Ctrl Pts',(95.5025032228997,0.685275347883298,-5.72482134574947));
#27676=CARTESIAN_POINT('Ctrl Pts',(95.489816379428,0.667049919035916,-5.72334821345533));
#27677=CARTESIAN_POINT('Ctrl Pts',(95.4858195670488,0.661196255253561,-5.72287608700587));
#27678=CARTESIAN_POINT('Ctrl Pts',(95.4788344687226,0.650765033421525,-5.72203635217434));
#27679=CARTESIAN_POINT('Ctrl Pts',(95.4758247319586,0.646202037667464,-5.72166955395892));
#27680=CARTESIAN_POINT('Ctrl Pts',(95.4695753175003,0.636582402064186,-5.72089729611531));
#27681=CARTESIAN_POINT('Ctrl Pts',(95.4663423419096,0.631521617002292,-5.72049160379644));
#27682=CARTESIAN_POINT('Ctrl Pts',(95.4579195315733,0.618111885446169,-5.7194180284362));
#27683=CARTESIAN_POINT('Ctrl Pts',(95.4527953726369,0.609722451338708,-5.71874778904177));
#27684=CARTESIAN_POINT('Ctrl Pts',(95.430850584584,0.57276139946719,-5.71580033007014));
#27685=CARTESIAN_POINT('Ctrl Pts',(95.415137157913,0.543553394594989,-5.71348445856564));
#27686=CARTESIAN_POINT('Ctrl Pts',(95.3563772424238,0.422332742654527,-5.70392025898488));
#27687=CARTESIAN_POINT('Ctrl Pts',(95.3240872874809,0.325598630340479,-5.69634748999376));
#27688=CARTESIAN_POINT('Ctrl Pts',(95.300464323838,0.204750875911249,-5.68744238117124));
#27689=CARTESIAN_POINT('Ctrl Pts',(95.2969045661051,0.18344374177579,-5.68589462020311));
#27690=CARTESIAN_POINT('Ctrl Pts',(95.2920681372671,0.148627673997437,-5.68341332514271));
#27691=CARTESIAN_POINT('Ctrl Pts',(95.2904353332735,0.135173890054132,-5.68246601490637));
#27692=CARTESIAN_POINT('Ctrl Pts',(95.2885421434898,0.116949775552905,-5.68120094494768));
#27693=CARTESIAN_POINT('Ctrl Pts',(95.288078089193,0.112202273345499,-5.68087304481481));
#27694=CARTESIAN_POINT('Ctrl Pts',(95.2873521747314,0.10427891907399,-5.68032870412396));
#27695=CARTESIAN_POINT('Ctrl Pts',(95.287074341012,0.101104634078135,-5.68011140601076));
#27696=CARTESIAN_POINT('Ctrl Pts',(95.2865727868972,0.0950935589645371,
-5.67970143388091));
#27697=CARTESIAN_POINT('Ctrl Pts',(95.286346459544,0.0922570274612839,-5.67950861355182));
#27698=CARTESIAN_POINT('Ctrl Pts',(95.2858349315525,0.0855391184827548,
-5.67905340038521));
#27699=CARTESIAN_POINT('Ctrl Pts',(95.2855586825128,0.0816570626192244,
-5.67879149581972));
#27700=CARTESIAN_POINT('Ctrl Pts',(95.2846586381988,0.0680571666291416,
-5.67787776797413));
#27701=CARTESIAN_POINT('Ctrl Pts',(95.2841361036617,0.0583327044476577,
-5.67723119768886));
#27702=CARTESIAN_POINT('Ctrl Pts',(95.2807707702813,-0.0231475728569918,
-5.67186202260817));
#27703=CARTESIAN_POINT('Ctrl Pts',(95.2843753718439,-0.095028845834061,
-5.66743346157478));
#27704=CARTESIAN_POINT('Ctrl Pts',(95.3027482586768,-0.223968492128474,
-5.65937737689349));
#27705=CARTESIAN_POINT('Ctrl Pts',(95.3152778584639,-0.281098013369817,
-5.65576623500236));
#27706=CARTESIAN_POINT('Ctrl Pts',(95.3380386338425,-0.357301815401976,
-5.6506962472904));
#27707=CARTESIAN_POINT('Ctrl Pts',(95.3446276939245,-0.377376167546177,
-5.64933642128387));
#27708=CARTESIAN_POINT('Ctrl Pts',(95.3570346614309,-0.412003109071487,
-5.64694012448366));
#27709=CARTESIAN_POINT('Ctrl Pts',(95.3626098538399,-0.426637190606166,
-5.64591127443769));
#27710=CARTESIAN_POINT('Ctrl Pts',(95.3711670526367,-0.44781910534316,-5.64439624875106));
#27711=CARTESIAN_POINT('Ctrl Pts',(95.3739200557026,-0.454458069850465,
-5.64391764568959));
#27712=CARTESIAN_POINT('Ctrl Pts',(95.3788787941259,-0.466113576535248,
-5.64307055663204));
#27713=CARTESIAN_POINT('Ctrl Pts',(95.3810591206591,-0.471140745884402,
-5.64270293058108));
#27714=CARTESIAN_POINT('Ctrl Pts',(95.3856832030918,-0.481601874131068,
-5.64193309564437));
#27715=CARTESIAN_POINT('Ctrl Pts',(95.3881332660104,-0.487032857533316,
-5.64153068200183));
#27716=CARTESIAN_POINT('Ctrl Pts',(95.3946441178202,-0.501177946739725,
-5.64047525685493));
#27717=CARTESIAN_POINT('Ctrl Pts',(95.3987705132837,-0.509861183256431,
-5.63982003105973));
#27718=CARTESIAN_POINT('Ctrl Pts',(95.4167347212565,-0.546499615684872,
-5.63702336286759));
#27719=CARTESIAN_POINT('Ctrl Pts',(95.4315727757329,-0.573947450620124,
-5.63484796475069));
#27720=CARTESIAN_POINT('Ctrl Pts',(95.5003974252902,-0.689997021034247,
-5.62529010168684));
#27721=CARTESIAN_POINT('Ctrl Pts',(95.5648682690301,-0.771834586700886,
-5.6175542614041));
#27722=CARTESIAN_POINT('Ctrl Pts',(95.6547827204412,-0.859312490623622,
-5.60848026762067));
#27723=CARTESIAN_POINT('Ctrl Pts',(95.6707809644618,-0.874037551648785,
-5.60692212977617));
#27724=CARTESIAN_POINT('Ctrl Pts',(95.6974466788012,-0.89725085600912,-5.60442615975323));
#27725=CARTESIAN_POINT('Ctrl Pts',(95.7078695679955,-0.906011338315213,
-5.60347436226587));
#27726=CARTESIAN_POINT('Ctrl Pts',(95.7221532384821,-0.917600177844721,
-5.60220431860783));
#27727=CARTESIAN_POINT('Ctrl Pts',(95.7258822842986,-0.92058823493353,-5.60187583249435));
#27728=CARTESIAN_POINT('Ctrl Pts',(95.7321295098562,-0.925531958840676,
-5.60133078601179));
#27729=CARTESIAN_POINT('Ctrl Pts',(95.7346375935797,-0.927500215551443,
-5.60111336355869));
#27730=CARTESIAN_POINT('Ctrl Pts',(95.7393981997716,-0.931205036166788,
-5.60070335906815));
#27731=CARTESIAN_POINT('Ctrl Pts',(95.741649066718,-0.932943661788935,-5.60051062942343));
#27732=CARTESIAN_POINT('Ctrl Pts',(95.7469903425233,-0.937038589629881,
-5.60005588041998));
#27733=CARTESIAN_POINT('Ctrl Pts',(95.7500861831338,-0.939387801540041,
-5.59979434691962));
#27734=CARTESIAN_POINT('Ctrl Pts',(95.7610379419842,-0.947613204065069,
-5.59887609961655));
#27735=CARTESIAN_POINT('Ctrl Pts',(95.7689558551335,-0.953406715171152,
-5.59822473640774));
#27736=CARTESIAN_POINT('Ctrl Pts',(95.8346585394253,-1.00023193802587,-5.59291328236898));
#27737=CARTESIAN_POINT('Ctrl Pts',(95.8959747132288,-1.03607583160094,-5.58853916238241));
#27738=CARTESIAN_POINT('Ctrl Pts',(95.9893717519733,-1.07990423901555,-5.58215750248245));
#27739=CARTESIAN_POINT('Ctrl Pts',(96.0191448159215,-1.0924099011946,-5.58016236542273));
#27740=CARTESIAN_POINT('Ctrl Pts',(96.0841198429742,-1.1166112185005,-5.575833384827));
#27741=CARTESIAN_POINT('Ctrl Pts',(96.1194350390286,-1.12789878028869,-5.57349535293581));
#27742=CARTESIAN_POINT('Ctrl Pts',(96.1705962544478,-1.14162836724377,-5.57008488847906));
#27743=CARTESIAN_POINT('Ctrl Pts',(96.186052376743,-1.14544200520022,-5.56905172734688));
#27744=CARTESIAN_POINT('Ctrl Pts',(96.2138386284544,-1.15170331222544,-5.56718606237049));
#27745=CARTESIAN_POINT('Ctrl Pts',(96.2261397704475,-1.1542690960081,-5.5663572519445));
#27746=CARTESIAN_POINT('Ctrl Pts',(96.2449498724244,-1.15787945351502,-5.56508444074358));
#27747=CARTESIAN_POINT('Ctrl Pts',(96.2514307037255,-1.15906706701358,-5.56464492929147));
#27748=CARTESIAN_POINT('Ctrl Pts',(96.2627433148094,-1.16104214108223,-5.56387589064436));
#27749=CARTESIAN_POINT('Ctrl Pts',(96.2675707187557,-1.16185397842449,-5.56354713586417));
#27750=CARTESIAN_POINT('Ctrl Pts',(96.2784635032953,-1.16361608911865,-5.56280393188108));
#27751=CARTESIAN_POINT('Ctrl Pts',(96.2845314965744,-1.16454907201559,-5.56238895219395));
#27752=CARTESIAN_POINT('Ctrl Pts',(96.3009424486907,-1.16694114365526,-5.56126388603723));
#27753=CARTESIAN_POINT('Ctrl Pts',(96.3112977735901,-1.16831011886119,-5.56055102137778));
#27754=CARTESIAN_POINT('Ctrl Pts',(96.3616154086442,-1.17428225257527,-5.55707191237516));
#27755=CARTESIAN_POINT('Ctrl Pts',(96.4017732889135,-1.17697321977398,-5.55424747332402));
#27756=CARTESIAN_POINT('Ctrl Pts',(96.5255688587743,-1.17891746530055,-5.54539287080836));
#27757=CARTESIAN_POINT('Ctrl Pts',(96.6090494376241,-1.17132736313746,-5.53919640709423));
#27758=CARTESIAN_POINT('Ctrl Pts',(96.7183874491382,-1.14950364492487,-5.53107756824948));
#27759=CARTESIAN_POINT('Ctrl Pts',(96.7455628764944,-1.14306731825633,-5.52906182501057));
#27760=CARTESIAN_POINT('Ctrl Pts',(96.7830066083711,-1.1327803450723,-5.52630803074809));
#27761=CARTESIAN_POINT('Ctrl Pts',(96.7934874546576,-1.12974368657491,-5.52553986236412));
#27762=CARTESIAN_POINT('Ctrl Pts',(96.8117049614386,-1.1241898902565,-5.52421099644646));
#27763=CARTESIAN_POINT('Ctrl Pts',(96.8194604244305,-1.12173747448683,-5.52364730690342));
#27764=CARTESIAN_POINT('Ctrl Pts',(96.830894466228,-1.11799109320917,-5.52281987989255));
#27765=CARTESIAN_POINT('Ctrl Pts',(96.8345928285508,-1.11675895381272,-5.52255281307399));
#27766=CARTESIAN_POINT('Ctrl Pts',(96.8411704705455,-1.11453121609244,-5.52207892117662));
#27767=CARTESIAN_POINT('Ctrl Pts',(96.8440520716712,-1.11354278679734,-5.5218716945255));
#27768=CARTESIAN_POINT('Ctrl Pts',(96.8503345082934,-1.11136054235327,-5.52142074201043));
#27769=CARTESIAN_POINT('Ctrl Pts',(96.8537337158952,-1.11016229218871,-5.52117727638184));
#27770=CARTESIAN_POINT('Ctrl Pts',(96.8632466959516,-1.10675970835665,-5.52049725960169));
#27771=CARTESIAN_POINT('Ctrl Pts',(96.8693479162596,-1.10452030619149,-5.52006268610357));
#27772=CARTESIAN_POINT('Ctrl Pts',(96.9053012610343,-1.09098518504615,-5.51750931701474));
#27773=CARTESIAN_POINT('Ctrl Pts',(96.9347056582239,-1.07852914466909,-5.51545158913015));
#27774=CARTESIAN_POINT('Ctrl Pts',(97.0484599631954,-1.02478796095945,-5.50747684340306));
#27775=CARTESIAN_POINT('Ctrl Pts',(97.1282516015357,-0.974676283019627,
-5.50182500432036));
#27776=CARTESIAN_POINT('Ctrl Pts',(97.2324486018821,-0.890377193533662,
-5.49335376062515));
#27777=CARTESIAN_POINT('Ctrl Pts',(97.2623345652234,-0.863559988907316,
-5.49077574323717));
#27778=CARTESIAN_POINT('Ctrl Pts',(97.2979235537985,-0.828182392055194,
-5.48747220191942));
#27779=CARTESIAN_POINT('Ctrl Pts',(97.3049642361021,-0.821001923493989,
-5.48680640957296));
#27780=CARTESIAN_POINT('Ctrl Pts',(97.3160951657908,-0.809355319620759,
-5.48573340927773));
#27781=CARTESIAN_POINT('Ctrl Pts',(97.3202445181321,-0.804946162335179,
-5.48532873850814));
#27782=CARTESIAN_POINT('Ctrl Pts',(97.3280670439595,-0.796504352581008,
-5.48455674466188));
#27783=CARTESIAN_POINT('Ctrl Pts',(97.3317465694028,-0.792477780660205,
-5.48418970310066));
#27784=CARTESIAN_POINT('Ctrl Pts',(97.3400798211692,-0.78323036248578,-5.48334934717114));
#27785=CARTESIAN_POINT('Ctrl Pts',(97.3447152422995,-0.777993372432849,
-5.48287529192542));
#27786=CARTESIAN_POINT('Ctrl Pts',(97.3588940316143,-0.761684097040048,
-5.48140442817136));
#27787=CARTESIAN_POINT('Ctrl Pts',(97.3682778079847,-0.750475556050734,
-5.48040121905146));
#27788=CARTESIAN_POINT('Ctrl Pts',(97.436473413914,-0.665867739332167,-5.47288111427207));
#27789=CARTESIAN_POINT('Ctrl Pts',(97.4865016509802,-0.585846323151347,
-5.46601669660043));
#27790=CARTESIAN_POINT('Ctrl Pts',(97.5339384633548,-0.484862985224618,
-5.45783004902265));
#27791=CARTESIAN_POINT('Ctrl Pts',(97.5410453059725,-0.468811087128935,
-5.45654325510106));
#27792=CARTESIAN_POINT('Ctrl Pts',(97.5598981192014,-0.423520388132378,
-5.45296097173667));
#27793=CARTESIAN_POINT('Ctrl Pts',(97.5708343322387,-0.393958456902307,
-5.45067781824604));
#27794=CARTESIAN_POINT('Ctrl Pts',(97.5860054142911,-0.347273325861935,
-5.44718901233288));
#27795=CARTESIAN_POINT('Ctrl Pts',(97.5910637033339,-0.330434262781404,
-5.44595372779672));
#27796=CARTESIAN_POINT('Ctrl Pts',(97.5971398660988,-0.308430048561292,
-5.4443746873436));
#27797=CARTESIAN_POINT('Ctrl Pts',(97.5985025546664,-0.303363505224976,
-5.44401350535972));
#27798=CARTESIAN_POINT('Ctrl Pts',(97.6006645749986,-0.295105380370486,
-5.44342888241791));
#27799=CARTESIAN_POINT('Ctrl Pts',(97.6014844520393,-0.291919326607394,
-5.44320431402822));
#27800=CARTESIAN_POINT('Ctrl Pts',(97.6030519666137,-0.28572043865021,-5.4427693524694));
#27801=CARTESIAN_POINT('Ctrl Pts',(97.6038010562302,-0.282708033228517,
-5.44255888327028));
#27802=CARTESIAN_POINT('Ctrl Pts',(97.605610563367,-0.275306409867426,-5.44204389264466));
#27803=CARTESIAN_POINT('Ctrl Pts',(97.6066576801282,-0.270913926734831,
-5.44174011582839));
#27804=CARTESIAN_POINT('Ctrl Pts',(97.6096044133528,-0.258229903016054,
-5.44086793137785));
#27805=CARTESIAN_POINT('Ctrl Pts',(97.6114395452146,-0.249923466283105,
-5.4403029308484));
#27806=CARTESIAN_POINT('Ctrl Pts',(97.6297635801912,-0.162496345475907,
-5.43441381042546));
#27807=CARTESIAN_POINT('Ctrl Pts',(97.6381589362903,-0.0818864593552734,
-5.42946830519488));
#27808=CARTESIAN_POINT('Ctrl Pts',(97.6382994290975,0.0768514002990383,
-5.41964384216038));
#27809=CARTESIAN_POINT('Ctrl Pts',(97.6306411435783,0.154548747557045,-5.41478873483599));
#27810=CARTESIAN_POINT('Ctrl Pts',(97.6133286927285,0.241134252189176,-5.40899400712145));
#27811=CARTESIAN_POINT('Ctrl Pts',(97.6111501544426,0.251324523573465,-5.40830616440694));
#27812=CARTESIAN_POINT('Ctrl Pts',(97.6073414308672,0.26805122568323,-5.40716677634204));
#27813=CARTESIAN_POINT('Ctrl Pts',(97.60578984222,0.274605099016429,-5.40671771070679));
#27814=CARTESIAN_POINT('Ctrl Pts',(97.6028860716366,0.286417664239892,-5.40590339921509));
#27815=CARTESIAN_POINT('Ctrl Pts',(97.601553565,0.291681034595023,-5.4055387876645));
#27816=CARTESIAN_POINT('Ctrl Pts',(97.598617359946,0.302950857302568,-5.40475418342152));
#27817=CARTESIAN_POINT('Ctrl Pts',(97.5970024068985,0.308954179512459,-5.40433384099797));
#27818=CARTESIAN_POINT('Ctrl Pts',(97.5924512798941,0.325353546610647,-5.40317887652352));
#27819=CARTESIAN_POINT('Ctrl Pts',(97.5894195419895,0.335722206733086,-5.40244121817134));
#27820=CARTESIAN_POINT('Ctrl Pts',(97.5707633930291,0.396414569854131,-5.39807833650425));
#27821=CARTESIAN_POINT('Ctrl Pts',(97.5519207142527,0.44567862147027,-5.39434985427729));
#27822=CARTESIAN_POINT('Ctrl Pts',(97.4960200978936,0.566807208304178,-5.38471244433334));
#27823=CARTESIAN_POINT('Ctrl Pts',(97.4547501518101,0.636427082316978,-5.37871355981902));
#27824=CARTESIAN_POINT('Ctrl Pts',(97.3881225908172,0.726325048281785,-5.37062514353316));
#27825=CARTESIAN_POINT('Ctrl Pts',(97.3685692265334,0.750628503650095,-5.36840156045603));
#27826=CARTESIAN_POINT('Ctrl Pts',(97.3438262925529,0.778997946605039,-5.36578658686824));
#27827=CARTESIAN_POINT('Ctrl Pts',(97.3395399745868,0.783831634365499,-5.36534033699336));
#27828=CARTESIAN_POINT('Ctrl Pts',(97.3328064593485,0.791300318824106,-5.3646500522102));
#27829=CARTESIAN_POINT('Ctrl Pts',(97.3303866815795,0.7939597016652,-5.36440410748264));
#27830=CARTESIAN_POINT('Ctrl Pts',(97.325893600454,0.798852484575092,-5.36395139596623));
#27831=CARTESIAN_POINT('Ctrl Pts',(97.3238238103004,0.801088917421071,-5.363744389655));
#27832=CARTESIAN_POINT('Ctrl Pts',(97.3190785226344,0.806176504433217,-5.36327327255492));
#27833=CARTESIAN_POINT('Ctrl Pts',(97.3163974895489,0.809022389345375,-5.36300958313007));
#27834=CARTESIAN_POINT('Ctrl Pts',(97.308054015397,0.817790988240682,-5.36219642777955));
#27835=CARTESIAN_POINT('Ctrl Pts',(97.3023437559443,0.823668153348542,-5.36165042765428));
#27836=CARTESIAN_POINT('Ctrl Pts',(97.288814036332,0.837305623865464,-5.36037975620669));
#27837=CARTESIAN_POINT('Ctrl Pts',(97.2809460012071,0.845016880650662,-5.35965835878946));
#27838=CARTESIAN_POINT('Ctrl Pts',(97.2524648315658,0.872157623555244,-5.35710365577217));
#27839=CARTESIAN_POINT('Ctrl Pts',(97.2312592988316,0.890953617489837,-5.35530492022628));
#27840=CARTESIAN_POINT('Ctrl Pts',(97.1430395633735,0.963639379116592,-5.34812958377198));
#27841=CARTESIAN_POINT('Ctrl Pts',(97.0708978518712,1.01088024767369,-5.34292399197283));
#27842=CARTESIAN_POINT('Ctrl Pts',(96.9607245276159,1.0668956568461,-5.33509787021397));
#27843=CARTESIAN_POINT('Ctrl Pts',(96.9263997047152,1.08232585333287,-5.33267840654164));
#27844=CARTESIAN_POINT('Ctrl Pts',(96.8818677017838,1.09983322899141,-5.32952959915147));
#27845=CARTESIAN_POINT('Ctrl Pts',(96.8722892319809,1.10345541561006,-5.32885182274335));
#27846=CARTESIAN_POINT('Ctrl Pts',(96.8569366488752,1.10903340188167,-5.32776409832691));
#27847=CARTESIAN_POINT('Ctrl Pts',(96.8511923325133,1.11107012419607,-5.32735681445409));
#27848=CARTESIAN_POINT('Ctrl Pts',(96.840799922149,1.114664330606,-5.32661931059646));
#27849=CARTESIAN_POINT('Ctrl Pts',(96.8361573912865,1.11623756464453,-5.326289614486));
#27850=CARTESIAN_POINT('Ctrl Pts',(96.8251908348327,1.11987768379753,-5.32551018268503));
#27851=CARTESIAN_POINT('Ctrl Pts',(96.8188589037513,1.12192003542727,-5.32505966150492));
#27852=CARTESIAN_POINT('Ctrl Pts',(96.8002177201358,1.12775880240779,-5.32373171085577));
#27853=CARTESIAN_POINT('Ctrl Pts',(96.7878634256494,1.1314069476608,-5.32284955112851));
#27854=CARTESIAN_POINT('Ctrl Pts',(96.7596209580207,1.13924547484234,-5.32082746164635));
#27855=CARTESIAN_POINT('Ctrl Pts',(96.7437002266553,1.14330739159579,-5.31968369510516));
#27856=CARTESIAN_POINT('Ctrl Pts',(96.6898312963472,1.15585698978664,-5.31579983411951));
#27857=CARTESIAN_POINT('Ctrl Pts',(96.6515520616501,1.16279760964249,-5.3130160256141));
#27858=CARTESIAN_POINT('Ctrl Pts',(96.5416988677981,1.17714472093669,-5.30498036705704));
#27859=CARTESIAN_POINT('Ctrl Pts',(96.4696951751851,1.17990704433475,-5.29964893226738));
#27860=CARTESIAN_POINT('Ctrl Pts',(96.3644121172927,1.17430398017979,-5.29201178424458));
#27861=CARTESIAN_POINT('Ctrl Pts',(96.331021232215,1.17109337628063,-5.28961545520223));
#27862=CARTESIAN_POINT('Ctrl Pts',(96.2918498230298,1.16563065230088,-5.28686688124989));
#27863=CARTESIAN_POINT('Ctrl Pts',(96.2858961654597,1.16475380719038,-5.28645085604166));
#27864=CARTESIAN_POINT('Ctrl Pts',(96.2761821506405,1.16324698511417,-5.28577517633201));
#27865=CARTESIAN_POINT('Ctrl Pts',(96.2724177571025,1.16264432752759,-5.28551410035349));
#27866=CARTESIAN_POINT('Ctrl Pts',(96.2656551243243,1.16152796469055,-5.28504653959556));
#27867=CARTESIAN_POINT('Ctrl Pts',(96.2626559005756,1.16102091521025,-5.28483969832842));
#27868=CARTESIAN_POINT('Ctrl Pts',(96.2560383190335,1.15987575711783,-5.2843844692746));
#27869=CARTESIAN_POINT('Ctrl Pts',(96.2524209652957,1.15923233434639,-5.2841363796478));
#27870=CARTESIAN_POINT('Ctrl Pts',(96.2419036282824,1.15731078757132,-5.2834170984713));
#27871=CARTESIAN_POINT('Ctrl Pts',(96.235011838196,1.15598788494674,-5.2829483169619));
#27872=CARTESIAN_POINT('Ctrl Pts',(96.1734638051566,1.14360214650284,-5.27878128716008));
#27873=CARTESIAN_POINT('Ctrl Pts',(96.1196379030029,1.12873046166619,-5.27527322457391));
#27874=CARTESIAN_POINT('Ctrl Pts',(96.0172455471707,1.09244260747017,-5.26851957117317));
#27875=CARTESIAN_POINT('Ctrl Pts',(95.9687186069067,1.07147020317641,-5.26527965674562));
#27876=CARTESIAN_POINT('Ctrl Pts',(95.921801349668,1.04733917674357,-5.26198394263684));
#27877=CARTESIAN_POINT('',(97.6382308590426,0.000461794101737356,-5.32468518566653));
#27878=CARTESIAN_POINT('Ctrl Pts',(95.9218017437159,1.04733937941473,-5.16217169173788));
#27879=CARTESIAN_POINT('Ctrl Pts',(95.9325114231549,1.05284770052691,-5.16293309366042));
#27880=CARTESIAN_POINT('Ctrl Pts',(95.9433093591508,1.05819369090224,-5.16369858274992));
#27881=CARTESIAN_POINT('Ctrl Pts',(95.980440187364,1.07587223909229,-5.16632690890821));
#27882=CARTESIAN_POINT('Ctrl Pts',(96.0071401828503,1.08739235765067,-5.16821049507675));
#27883=CARTESIAN_POINT('Ctrl Pts',(96.0429821275043,1.10130731070932,-5.17074547651919));
#27884=CARTESIAN_POINT('Ctrl Pts',(96.0517669104993,1.10459761222691,-5.17136726210828));
#27885=CARTESIAN_POINT('Ctrl Pts',(96.0661459615139,1.10978821073429,-5.17238621639936));
#27886=CARTESIAN_POINT('Ctrl Pts',(96.0717169906452,1.11175201262678,-5.17278129224412));
#27887=CARTESIAN_POINT('Ctrl Pts',(96.08249975661,1.11546200730409,-5.17354663900523));
#27888=CARTESIAN_POINT('Ctrl Pts',(96.0877094180057,1.11721379129877,-5.17391671576547));
#27889=CARTESIAN_POINT('Ctrl Pts',(96.0998698778694,1.12120830338109,-5.17478135081686));
#27890=CARTESIAN_POINT('Ctrl Pts',(96.1068295928854,1.12342294722857,-5.17527680526923));
#27891=CARTESIAN_POINT('Ctrl Pts',(96.129397858974,1.13037387781512,-5.17688562150878));
#27892=CARTESIAN_POINT('Ctrl Pts',(96.1450837378275,1.13485050521425,-5.17800724002358));
#27893=CARTESIAN_POINT('Ctrl Pts',(96.1824060124109,1.14466846368908,-5.18068535063957));
#27894=CARTESIAN_POINT('Ctrl Pts',(96.2041104000099,1.14972413773879,-5.18225020093183));
#27895=CARTESIAN_POINT('Ctrl Pts',(96.288938193836,1.16696199047061,-5.1883948937014));
#27896=CARTESIAN_POINT('Ctrl Pts',(96.3528683155052,1.17458292080017,-5.19309491776227));
#27897=CARTESIAN_POINT('Ctrl Pts',(96.4804886117314,1.17928757440343,-5.20246763211301));
#27898=CARTESIAN_POINT('Ctrl Pts',(96.5439754131948,1.17649892969447,-5.20712347759578));
#27899=CARTESIAN_POINT('Ctrl Pts',(96.6168562138963,1.16736534236046,-5.21227396370946));
#27900=CARTESIAN_POINT('Ctrl Pts',(96.6267629389786,1.1659954469632,-5.2129697231798));
#27901=CARTESIAN_POINT('Ctrl Pts',(96.6405427691712,1.16391077529573,-5.21393034287619));
#27902=CARTESIAN_POINT('Ctrl Pts',(96.6444312206168,1.16330256194206,-5.21420061809634));
#27903=CARTESIAN_POINT('Ctrl Pts',(96.6511364027448,1.16221930778189,-5.21466521704936));
#27904=CARTESIAN_POINT('Ctrl Pts',(96.6539545580521,1.16175349557094,-5.2148600400038));
#27905=CARTESIAN_POINT('Ctrl Pts',(96.6598994657244,1.16074863112626,-5.21527003888125));
#27906=CARTESIAN_POINT('Ctrl Pts',(96.6630257858721,1.16020718795231,-5.21548507362493));
#27907=CARTESIAN_POINT('Ctrl Pts',(96.6707833108322,1.15883136088811,-5.21601730513316));
#27908=CARTESIAN_POINT('Ctrl Pts',(96.6754118376694,1.15798183118038,-5.21633366725215));
#27909=CARTESIAN_POINT('Ctrl Pts',(96.6928842217307,1.15466654135741,-5.2175238241673));
#27910=CARTESIAN_POINT('Ctrl Pts',(96.7056923580069,1.1520145410591,-5.21838790381682));
#27911=CARTESIAN_POINT('Ctrl Pts',(96.7385100491239,1.14464727587447,-5.22058653337873));
#27912=CARTESIAN_POINT('Ctrl Pts',(96.7584457068214,1.13962040619926,-5.22190734172225));
#27913=CARTESIAN_POINT('Ctrl Pts',(96.8630663760272,1.11030641302517,-5.22880885995858));
#27914=CARTESIAN_POINT('Ctrl Pts',(96.9449609144002,1.07709625997903,-5.23412641153768));
#27915=CARTESIAN_POINT('Ctrl Pts',(97.0630166444056,1.01300679332722,-5.24256641136791));
#27916=CARTESIAN_POINT('Ctrl Pts',(97.1023053083475,0.98858118792749,-5.24551906601836));
#27917=CARTESIAN_POINT('Ctrl Pts',(97.1488517974383,0.955696953102273,-5.24926420194541));
#27918=CARTESIAN_POINT('Ctrl Pts',(97.1575634536765,0.949361396033293,-5.24997635012737));
#27919=CARTESIAN_POINT('Ctrl Pts',(97.1712083271043,0.939149082161794,-5.25111036606283));
#27920=CARTESIAN_POINT('Ctrl Pts',(97.1761997120439,0.935350765317167,-5.25152922066824));
#27921=CARTESIAN_POINT('Ctrl Pts',(97.1852673607145,0.928335436848108,-5.2522976687945));
#27922=CARTESIAN_POINT('Ctrl Pts',(97.1893531671586,0.925130971288498,-5.25264676651902));
#27923=CARTESIAN_POINT('Ctrl Pts',(97.1935394262451,0.921802775277868,-5.25300742559174));
#27924=CARTESIAN_POINT('Ctrl Pts',(97.1936612390565,0.921705891184178,-5.25301792275109));
#27925=CARTESIAN_POINT('Ctrl Pts',(97.1938925314831,0.92152185736795,-5.25303785922484));
#27926=CARTESIAN_POINT('Ctrl Pts',(97.194002014803,0.92143471225615,-5.25304729835756));
#27927=CARTESIAN_POINT('Ctrl Pts',(97.1942103985456,0.921268784993963,-5.25306526823877));
#27928=CARTESIAN_POINT('Ctrl Pts',(97.1943093017797,0.921190006454349,-5.25307379884187));
#27929=CARTESIAN_POINT('Ctrl Pts',(97.1944979534539,0.921039691702677,-5.25309007372226));
#27930=CARTESIAN_POINT('Ctrl Pts',(97.1945877042653,0.920968158186419,-5.25309781790002));
#27931=CARTESIAN_POINT('Ctrl Pts',(97.194759229824,0.920831407260833,-5.25311262075844));
#27932=CARTESIAN_POINT('Ctrl Pts',(97.1948410062387,0.920766192157478,-5.25311967934184));
#27933=CARTESIAN_POINT('Ctrl Pts',(97.1949975640776,0.920641306196632,-5.25313319499576));
#27934=CARTESIAN_POINT('Ctrl Pts',(97.1950723470267,0.920581637034882,-5.25313965200468));
#27935=CARTESIAN_POINT('Ctrl Pts',(97.1952157427541,0.920467193279049,-5.25315203516747));
#27936=CARTESIAN_POINT('Ctrl Pts',(97.1952843565894,0.920412420195925,-5.25315796125634));
#27937=CARTESIAN_POINT('Ctrl Pts',(97.1954161121977,0.920307218147145,-5.25316934242036));
#27938=CARTESIAN_POINT('Ctrl Pts',(97.1954792549115,0.920256790350043,-5.25317479744935));
#27939=CARTESIAN_POINT('Ctrl Pts',(97.1956006635515,0.920159809048524,-5.25318528755037));
#27940=CARTESIAN_POINT('Ctrl Pts',(97.195658930367,0.920113256411223,-5.25319032259453));
#27941=CARTESIAN_POINT('Ctrl Pts',(97.1957710986809,0.920023621377334,-5.25320001661933));
#27942=CARTESIAN_POINT('Ctrl Pts',(97.1958250007531,0.91998053982756,-5.25320467556288));
#27943=CARTESIAN_POINT('Ctrl Pts',(97.1959288813152,0.919897497711922,-5.2532136553148));
#27944=CARTESIAN_POINT('Ctrl Pts',(97.1959788602175,0.919857537903602,-5.25321797608661));
#27945=CARTESIAN_POINT('Ctrl Pts',(97.2013289860205,0.915579218119432,-5.25368055218572));
#27946=CARTESIAN_POINT('Ctrl Pts',(97.2065923057161,0.911295209390987,-5.25414061265473));
#27947=CARTESIAN_POINT('Ctrl Pts',(97.2176641728282,0.902123194033613,-5.25511917498667));
#27948=CARTESIAN_POINT('Ctrl Pts',(97.2234630506065,0.897224052072272,-5.25563811122635));
#27949=CARTESIAN_POINT('Ctrl Pts',(97.2387430188533,0.884059621304366,-5.25702287318334));
#27950=CARTESIAN_POINT('Ctrl Pts',(97.2481395368949,0.875698116540824,-5.25789255003654));
#27951=CARTESIAN_POINT('Ctrl Pts',(97.2766665918279,0.84948263079792,-5.26058997347246));
#27952=CARTESIAN_POINT('Ctrl Pts',(97.2953364183069,0.831141332368948,-5.26243701815565));
#27953=CARTESIAN_POINT('Ctrl Pts',(97.3454627794579,0.778502882479704,-5.26762876682549));
#27954=CARTESIAN_POINT('Ctrl Pts',(97.3755196509311,0.742942201573209,-5.27101751918493));
#27955=CARTESIAN_POINT('Ctrl Pts',(97.4482753649633,0.645730634051767,-5.27991884891027));
#27956=CARTESIAN_POINT('Ctrl Pts',(97.4873382723476,0.581611364097249,-5.28545317347696));
#27957=CARTESIAN_POINT('Ctrl Pts',(97.5242300271725,0.505593435052069,-5.29137252419021));
#27958=CARTESIAN_POINT('Ctrl Pts',(97.528307182252,0.49692451444722,-5.29203850791343));
#27959=CARTESIAN_POINT('Ctrl Pts',(97.5338801976453,0.484689644019447,-5.29296486162387));
#27960=CARTESIAN_POINT('Ctrl Pts',(97.5354648330367,0.481164886634185,-5.29323016966514));
#27961=CARTESIAN_POINT('Ctrl Pts',(97.5382976439475,0.474779921264936,-5.29370785763682));
#27962=CARTESIAN_POINT('Ctrl Pts',(97.5395518532134,0.471922436451773,-5.29392059211006));
#27963=CARTESIAN_POINT('Ctrl Pts',(97.5420944159229,0.466066541990372,-5.29435436675902));
#27964=CARTESIAN_POINT('Ctrl Pts',(97.5433816878933,0.463067709687528,-5.29457534241328));
#27965=CARTESIAN_POINT('Ctrl Pts',(97.546659349676,0.45534364417822,-5.29514162070483));
#27966=CARTESIAN_POINT('Ctrl Pts',(97.5486314038657,0.450610632768498,-5.29548584793617));
#27967=CARTESIAN_POINT('Ctrl Pts',(97.5568112728848,0.430611730348203,-5.29692933806477));
#27968=CARTESIAN_POINT('Ctrl Pts',(97.5627295750134,0.415228461125412,-5.29801276699189));
#27969=CARTESIAN_POINT('Ctrl Pts',(97.5780322361848,0.372816971000223,-5.30093996531587));
#27970=CARTESIAN_POINT('Ctrl Pts',(97.5867581948483,0.345562102544989,-5.30275582802512));
#27971=CARTESIAN_POINT('Ctrl Pts',(97.6234718630875,0.214645550701067,-5.31128789975765));
#27972=CARTESIAN_POINT('Ctrl Pts',(97.6381887681913,0.107809410902377,-5.31774410507905));
#27973=CARTESIAN_POINT('Ctrl Pts',(97.6382308590426,0.000461794101737356,
-5.32468518566653));
#27974=CARTESIAN_POINT('Ctrl Pts',(97.638230859503,0.000460618401015764,
-5.32468526168717));
#27975=CARTESIAN_POINT('Ctrl Pts',(97.6382378236093,-0.0173458250786842,
-5.32583662409341));
#27976=CARTESIAN_POINT('Ctrl Pts',(97.6378409637853,-0.0351495341057705,
-5.3269987006894));
#27977=CARTESIAN_POINT('Ctrl Pts',(97.6367313540619,-0.0598113954557334,
-5.32862679494736));
#27978=CARTESIAN_POINT('Ctrl Pts',(97.6363618105115,-0.0666829413758868,
-5.32908240637083));
#27979=CARTESIAN_POINT('Ctrl Pts',(97.6356001256255,-0.0788558086913148,
-5.32989321504635));
#27980=CARTESIAN_POINT('Ctrl Pts',(97.6352322688323,-0.0841584982872386,
-5.33024766120918));
#27981=CARTESIAN_POINT('Ctrl Pts',(97.6344302213695,-0.0946872137314863,
-5.33095399399462));
#27982=CARTESIAN_POINT('Ctrl Pts',(97.6339969971204,-0.099913191460944,
-5.33130584291699));
#27983=CARTESIAN_POINT('Ctrl Pts',(97.6329978402688,-0.111061214489211,
-5.33205917212182));
#27984=CARTESIAN_POINT('Ctrl Pts',(97.6324219107043,-0.116982194009348,
-5.33246095289328));
#27985=CARTESIAN_POINT('Ctrl Pts',(97.630802174728,-0.132419567441288,-5.33351297572821));
#27986=CARTESIAN_POINT('Ctrl Pts',(97.6296871666797,-0.14192788445596,-5.33416540616123));
#27987=CARTESIAN_POINT('Ctrl Pts',(97.6244929331619,-0.18199316363182,-5.33693407147658));
#27988=CARTESIAN_POINT('Ctrl Pts',(97.6193310265985,-0.212394929965198,
-5.33908342214081));
#27989=CARTESIAN_POINT('Ctrl Pts',(97.5929021273988,-0.33797105029485,-5.34817017477487));
#27990=CARTESIAN_POINT('Ctrl Pts',(97.5610507856395,-0.430515144994756,
-5.35541367492539));
#27991=CARTESIAN_POINT('Ctrl Pts',(97.5067139889575,-0.541451832904505,
-5.36439309909972));
#27992=CARTESIAN_POINT('Ctrl Pts',(97.4944816094563,-0.564461223123242,
-5.36627019358033));
#27993=CARTESIAN_POINT('Ctrl Pts',(97.4763004907727,-0.596082497040434,
-5.3688537006441));
#27994=CARTESIAN_POINT('Ctrl Pts',(97.4709856868373,-0.60504865614563,-5.36958667748986));
#27995=CARTESIAN_POINT('Ctrl Pts',(97.4614605742922,-0.620641979600681,
-5.37086067588182));
#27996=CARTESIAN_POINT('Ctrl Pts',(97.4573017846765,-0.627299694666744,
-5.37140437779457));
#27997=CARTESIAN_POINT('Ctrl Pts',(97.4510084106993,-0.637153965702715,
-5.37220819786072));
#27998=CARTESIAN_POINT('Ctrl Pts',(97.4489243435179,-0.640382296191599,
-5.37247138468805));
#27999=CARTESIAN_POINT('Ctrl Pts',(97.4453217458339,-0.645903421974288,
-5.3729211532705));
#28000=CARTESIAN_POINT('Ctrl Pts',(97.443810948052,-0.648201156388453,-5.37310822989889));
#28001=CARTESIAN_POINT('Ctrl Pts',(97.4403453926368,-0.653431831299147,
-5.3735338521341));
#28002=CARTESIAN_POINT('Ctrl Pts',(97.4383855073629,-0.656361304166322,
-5.37377205496725));
#28003=CARTESIAN_POINT('Ctrl Pts',(97.4329708054791,-0.664376657797896,
-5.37442346710587));
#28004=CARTESIAN_POINT('Ctrl Pts',(97.429489209423,-0.669444441046857,-5.37483495441179));
#28005=CARTESIAN_POINT('Ctrl Pts',(97.4110385993011,-0.695855448986054,
-5.37697879156716));
#28006=CARTESIAN_POINT('Ctrl Pts',(97.3954024539975,-0.716726354976169,
-5.37867072954338));
#28007=CARTESIAN_POINT('Ctrl Pts',(97.3359828655634,-0.790781217796423,
-5.3847350472745));
#28008=CARTESIAN_POINT('Ctrl Pts',(97.2882486473289,-0.840619167683486,
-5.38894242112025));
#28009=CARTESIAN_POINT('Ctrl Pts',(97.2015819794642,-0.916520606239502,
-5.3960885207993));
#28010=CARTESIAN_POINT('Ctrl Pts',(97.1649674287411,-0.944954525189039,
-5.39898351779418));
#28011=CARTESIAN_POINT('Ctrl Pts',(97.1116203950136,-0.981555032600435,
-5.40312843161472));
#28012=CARTESIAN_POINT('Ctrl Pts',(97.0962244432419,-0.991596195692752,
-5.40431647152264));
#28013=CARTESIAN_POINT('Ctrl Pts',(97.0722309882125,-1.00645609388381,-5.40616008147104));
#28014=CARTESIAN_POINT('Ctrl Pts',(97.0637970750983,-1.01153429109864,-5.40680666712876));
#28015=CARTESIAN_POINT('Ctrl Pts',(97.0497143895474,-1.01977493011572,-5.40788452336012));
#28016=CARTESIAN_POINT('Ctrl Pts',(97.04410133097,-1.02299765519692,-5.40831366865909));
#28017=CARTESIAN_POINT('Ctrl Pts',(97.0344968791195,-1.02840725681958,-5.40904734033586));
#28018=CARTESIAN_POINT('Ctrl Pts',(97.0305188094087,-1.0306175869972,-5.40935103628488));
#28019=CARTESIAN_POINT('Ctrl Pts',(97.0218411399399,-1.0353735389047,-5.41001317456163));
#28020=CARTESIAN_POINT('Ctrl Pts',(97.0171368399942,-1.03791032678431,-5.41037191703864));
#28021=CARTESIAN_POINT('Ctrl Pts',(97.0070639276849,-1.04325395264039,-5.41113969520755));
#28022=CARTESIAN_POINT('Ctrl Pts',(97.0016906173684,-1.04605155455228,-5.41154904044489));
#28023=CARTESIAN_POINT('Ctrl Pts',(96.9873255178304,-1.05339040079975,-5.41264294414645));
#28024=CARTESIAN_POINT('Ctrl Pts',(96.9782968104723,-1.05785786326406,-5.41333002248117));
#28025=CARTESIAN_POINT('Ctrl Pts',(96.9374302897532,-1.07743035514373,-5.41643869698796));
#28026=CARTESIAN_POINT('Ctrl Pts',(96.9049844806845,-1.09121629757378,-5.41890424100877));
#28027=CARTESIAN_POINT('Ctrl Pts',(96.7789755310914,-1.13820349061619,-5.42847459571587));
#28028=CARTESIAN_POINT('Ctrl Pts',(96.6819712358574,-1.16098395846934,-5.4358738488012));
#28029=CARTESIAN_POINT('Ctrl Pts',(96.5619597130911,-1.17356582914659,-5.44459881579802));
#28030=CARTESIAN_POINT('Ctrl Pts',(96.5405791338558,-1.1752187400789,-5.44613493297173));
#28031=CARTESIAN_POINT('Ctrl Pts',(96.50570128527,-1.17695874316459,-5.44859972673861));
#28032=CARTESIAN_POINT('Ctrl Pts',(96.4922271668712,-1.17739924338115,-5.44954196900938));
#28033=CARTESIAN_POINT('Ctrl Pts',(96.4739881237726,-1.17768216354567,-5.45080140057567));
#28034=CARTESIAN_POINT('Ctrl Pts',(96.4692279804066,-1.17772713881187,-5.45112861861907));
#28035=CARTESIAN_POINT('Ctrl Pts',(96.4612835012376,-1.17775403075986,-5.45167212504533));
#28036=CARTESIAN_POINT('Ctrl Pts',(96.4580993213388,-1.17775189646947,-5.4518892657946));
#28037=CARTESIAN_POINT('Ctrl Pts',(96.4520683585878,-1.17772339499165,-5.45229916661042));
#28038=CARTESIAN_POINT('Ctrl Pts',(96.4492216051707,-1.17769961976727,-5.4524920715195));
#28039=CARTESIAN_POINT('Ctrl Pts',(96.4424775110639,-1.17761883932614,-5.45294776291437));
#28040=CARTESIAN_POINT('Ctrl Pts',(96.4385802816529,-1.17755280830645,-5.4532100585192));
#28041=CARTESIAN_POINT('Ctrl Pts',(96.4249119360751,-1.17725334350479,-5.45412657123468));
#28042=CARTESIAN_POINT('Ctrl Pts',(96.415143142031,-1.17691762155923,-5.45477549306419));
#28043=CARTESIAN_POINT('Ctrl Pts',(96.3344933813667,-1.17314024223382,-5.46009074903455));
#28044=CARTESIAN_POINT('Ctrl Pts',(96.2640422679642,-1.16341976501805,-5.46447028486917));
#28045=CARTESIAN_POINT('Ctrl Pts',(96.1374195657284,-1.13411017828015,-5.47250973570675));
#28046=CARTESIAN_POINT('Ctrl Pts',(96.0810362311465,-1.11651045763795,-5.47615475961267));
#28047=CARTESIAN_POINT('Ctrl Pts',(96.0064639804205,-1.08692913343066,-5.48126800021397));
#28048=CARTESIAN_POINT('Ctrl Pts',(95.9869338523051,-1.07856358893874,-5.48263520065668));
#28049=CARTESIAN_POINT('Ctrl Pts',(95.9533583934763,-1.06309411042212,-5.48504329802931));
#28050=CARTESIAN_POINT('Ctrl Pts',(95.939209151816,-1.05622821845859,-5.48607646728509));
#28051=CARTESIAN_POINT('Ctrl Pts',(95.9187897278934,-1.0458094983757,-5.48759665637089));
#28052=CARTESIAN_POINT('Ctrl Pts',(95.9124075671126,-1.042478992656,-5.48807602827467));
#28053=CARTESIAN_POINT('Ctrl Pts',(95.9012208319326,-1.03651011748646,-5.48892396877215));
#28054=CARTESIAN_POINT('Ctrl Pts',(95.896403348143,-1.03389630073277,-5.48929167132338));
#28055=CARTESIAN_POINT('Ctrl Pts',(95.8863927958785,-1.02837409517696,-5.49006116053804));
#28056=CARTESIAN_POINT('Ctrl Pts',(95.8812031911007,-1.02545978182514,-5.49046314854303));
#28057=CARTESIAN_POINT('Ctrl Pts',(95.8677126132603,-1.01774882656706,-5.49151631923112));
#28058=CARTESIAN_POINT('Ctrl Pts',(95.859447867508,-1.01289002332626,-5.49216969912916));
#28059=CARTESIAN_POINT('Ctrl Pts',(95.8247574794527,-0.991921642050991,
-5.49494767095819));
#28060=CARTESIAN_POINT('Ctrl Pts',(95.7989150422382,-0.974875950549584,
-5.49710565566995));
#28061=CARTESIAN_POINT('Ctrl Pts',(95.706279430953,-0.908392762490096,-5.50518071900474));
#28062=CARTESIAN_POINT('Ctrl Pts',(95.6441051078397,-0.852950450643157,
-5.51130429991718));
#28063=CARTESIAN_POINT('Ctrl Pts',(95.5532410473624,-0.752815428918454,
-5.5212023291402));
#28064=CARTESIAN_POINT('Ctrl Pts',(95.5207925828441,-0.711900543259572,
-5.52498626150539));
#28065=CARTESIAN_POINT('Ctrl Pts',(95.487208750986,-0.663238042333523,-5.52909863909753));
#28066=CARTESIAN_POINT('Ctrl Pts',(95.483307413545,-0.657476508841074,-5.52957968866295));
#28067=CARTESIAN_POINT('Ctrl Pts',(95.4774312689445,-0.648630707070114,
-5.53030897987359));
#28068=CARTESIAN_POINT('Ctrl Pts',(95.4754194871042,-0.645571363067762,
-5.53055953449048));
#28069=CARTESIAN_POINT('Ctrl Pts',(95.4717624122841,-0.639953100449615,
-5.53101653503211));
#28070=CARTESIAN_POINT('Ctrl Pts',(95.4701127593949,-0.637397180009341,
-5.53122325687331));
#28071=CARTESIAN_POINT('Ctrl Pts',(95.4664106398737,-0.63161215985099,-5.53168850446219));
#28072=CARTESIAN_POINT('Ctrl Pts',(95.4643639926712,-0.628379431795095,
-5.53194665195216));
#28073=CARTESIAN_POINT('Ctrl Pts',(95.4591144466176,-0.619997548518764,
-5.53261140361551));
#28074=CARTESIAN_POINT('Ctrl Pts',(95.4559354483774,-0.614833451641219,
-5.53301652337617));
#28075=CARTESIAN_POINT('Ctrl Pts',(95.4348507485854,-0.579982464840983,
-5.53572253217352));
#28076=CARTESIAN_POINT('Ctrl Pts',(95.4182216341332,-0.549538892354571,
-5.5379507701974));
#28077=CARTESIAN_POINT('Ctrl Pts',(95.3905176189747,-0.493023743390293,
-5.54192771611037));
#28078=CARTESIAN_POINT('Ctrl Pts',(95.3789937844784,-0.467203995578871,
-5.54368757396448));
#28079=CARTESIAN_POINT('Ctrl Pts',(95.3503928273341,-0.396376954943047,
-5.54842340347874));
#28080=CARTESIAN_POINT('Ctrl Pts',(95.3351274094051,-0.350698793242993,
-5.55138237740456));
#28081=CARTESIAN_POINT('Ctrl Pts',(95.3089759934743,-0.252891090980864,
-5.55771452055728));
#28082=CARTESIAN_POINT('Ctrl Pts',(95.2987431469547,-0.200703192690539,
-5.56109232144069));
#28083=CARTESIAN_POINT('Ctrl Pts',(95.2907078964055,-0.137270506138952,
-5.56529477092193));
#28084=CARTESIAN_POINT('Ctrl Pts',(95.2894959390874,-0.126515928830653,
-5.56601041612388));
#28085=CARTESIAN_POINT('Ctrl Pts',(95.287821037343,-0.109555875515638,-5.56714463664446));
#28086=CARTESIAN_POINT('Ctrl Pts',(95.2872587480136,-0.103360644712729,
-5.5675601295288));
#28087=CARTESIAN_POINT('Ctrl Pts',(95.2862977354553,-0.0917513530614053,
-5.56834106588334));
#28088=CARTESIAN_POINT('Ctrl Pts',(95.2858873137597,-0.086338404674241,
-5.56870613651701));
#28089=CARTESIAN_POINT('Ctrl Pts',(95.2850520423498,-0.0742106119814917,
-5.56952630307908));
#28090=CARTESIAN_POINT('Ctrl Pts',(95.284647286223,-0.067494620169433,-5.5699820084033));
#28091=CARTESIAN_POINT('Ctrl Pts',(95.2837634917776,-0.0503906954931974,
-5.57114661504496));
#28092=CARTESIAN_POINT('Ctrl Pts',(95.2833644581691,-0.039999391485766,
-5.57185795346008));
#28093=CARTESIAN_POINT('Ctrl Pts',(95.2812174229251,0.0453888502322086,
-5.57773583824771));
#28094=CARTESIAN_POINT('Ctrl Pts',(95.2865012949004,0.120376768314819,-5.58312120834398));
#28095=CARTESIAN_POINT('Ctrl Pts',(95.3082424323486,0.250327253599703,-5.59275807377661));
#28096=CARTESIAN_POINT('Ctrl Pts',(95.3216446802525,0.305564218632168,-5.59695003686976));
#28097=CARTESIAN_POINT('Ctrl Pts',(95.3455190167178,0.380018182784622,-5.602603277735));
#28098=CARTESIAN_POINT('Ctrl Pts',(95.3526155817885,0.400235391954122,-5.60413808164149));
#28099=CARTESIAN_POINT('Ctrl Pts',(95.36506707584,0.432833675955351,-5.60660101504056));
#28100=CARTESIAN_POINT('Ctrl Pts',(95.370089882657,0.445335722447427,-5.60754268650243));
#28101=CARTESIAN_POINT('Ctrl Pts',(95.3771760676975,0.462134444453824,-5.60880148476715));
#28102=CARTESIAN_POINT('Ctrl Pts',(95.3790523752516,0.466508255489532,-5.60912862775357));
#28103=CARTESIAN_POINT('Ctrl Pts',(95.3822281183213,0.473789015824457,-5.60967204383177));
#28104=CARTESIAN_POINT('Ctrl Pts',(95.3835129041438,0.476702244041119,-5.60988916871125));
#28105=CARTESIAN_POINT('Ctrl Pts',(95.385968878002,0.482210509913384,-5.61029906566339));
#28106=CARTESIAN_POINT('Ctrl Pts',(95.387137684739,0.484806563587004,-5.61049198241161));
#28107=CARTESIAN_POINT('Ctrl Pts',(95.3899292279519,0.490947320534827,-5.61094773414656));
#28108=CARTESIAN_POINT('Ctrl Pts',(95.3915601857716,0.494488282968222,-5.61121007793835));
#28109=CARTESIAN_POINT('Ctrl Pts',(95.3973540539785,0.506904692767635,-5.6121286021303));
#28110=CARTESIAN_POINT('Ctrl Pts',(95.4016103026919,0.515736494935508,-5.61277944987483));
#28111=CARTESIAN_POINT('Ctrl Pts',(95.4373376312303,0.587564116471556,-5.61806046933466));
#28112=CARTESIAN_POINT('Ctrl Pts',(95.4742948396696,0.647683220535143,-5.62240845072104));
#28113=CARTESIAN_POINT('Ctrl Pts',(95.5518977328858,0.75172814692553,-5.63043739231747));
#28114=CARTESIAN_POINT('Ctrl Pts',(95.5909315187167,0.796556210939607,-5.63410430716551));
#28115=CARTESIAN_POINT('Ctrl Pts',(95.6483503045073,0.853225295165076,-5.63924548449146));
#28116=CARTESIAN_POINT('Ctrl Pts',(95.6639273942333,0.867785653831878,-5.64061743009629));
#28117=CARTESIAN_POINT('Ctrl Pts',(95.6916986814796,0.892366269762142,-5.6430331275175));
#28118=CARTESIAN_POINT('Ctrl Pts',(95.7037152219328,0.902579265438339,-5.6440690826172));
#28119=CARTESIAN_POINT('Ctrl Pts',(95.7215166634698,0.917103474539165,-5.64559261699479));
#28120=CARTESIAN_POINT('Ctrl Pts',(95.7271421785552,0.921607965574694,-5.64607249968651));
#28121=CARTESIAN_POINT('Ctrl Pts',(95.7371190688649,0.929447526533811,-5.64692102407508));
#28122=CARTESIAN_POINT('Ctrl Pts',(95.7414530936686,0.932804403796896,-5.64728879578888));
#28123=CARTESIAN_POINT('Ctrl Pts',(95.7505384148764,0.939740412872528,-5.64805811311137));
#28124=CARTESIAN_POINT('Ctrl Pts',(95.7552936968788,0.943314042383193,-5.6484598579474));
#28125=CARTESIAN_POINT('Ctrl Pts',(95.7677703649107,0.95254328629406,-5.64951168172808));
#28126=CARTESIAN_POINT('Ctrl Pts',(95.7755338502618,0.95814097508483,-5.6501639475096));
#28127=CARTESIAN_POINT('Ctrl Pts',(95.8085620128926,0.98134864181115,-5.65293026343886));
#28128=CARTESIAN_POINT('Ctrl Pts',(95.8344420576964,0.998057343695313,-5.65507735584128));
#28129=CARTESIAN_POINT('Ctrl Pts',(95.8809073276512,1.02553759155734,-5.65889973545223));
#28130=CARTESIAN_POINT('Ctrl Pts',(95.901202188743,1.03674439082019,-5.66055885234695));
#28131=CARTESIAN_POINT('Ctrl Pts',(95.9218018640414,1.04733944130189,-5.66223110129989));
#28132=CARTESIAN_POINT('Origin',(96.460480949577,-7.19464945638997E-16,
0.924367114736168));
#28133=CARTESIAN_POINT('',(95.9218016184021,1.04733931496196,-6.2623154905088));
#28134=CARTESIAN_POINT('',(95.9218016730721,1.04733934308043,-6.16392795844921));
#28135=CARTESIAN_POINT('',(95.9218016730721,1.04733934308042,0.924367114736168));
#28136=CARTESIAN_POINT('',(97.6382308542487,0.000473862668674378,-5.92345611052503));
#28137=CARTESIAN_POINT('Ctrl Pts',(95.9218016184021,1.04733931496196,-6.26231549050881));
#28138=CARTESIAN_POINT('Ctrl Pts',(95.9027034372951,1.03751652374386,-6.26077924530074));
#28139=CARTESIAN_POINT('Ctrl Pts',(95.8838728183822,1.02717078126495,-6.25922892834475));
#28140=CARTESIAN_POINT('Ctrl Pts',(95.8384588123809,1.00057647339736,-6.25540622018832));
#28141=CARTESIAN_POINT('Ctrl Pts',(95.812221971306,0.983780972517538,-6.25312452485025));
#28142=CARTESIAN_POINT('Ctrl Pts',(95.7321245931071,0.927909962335828,-6.24595783254306));
#28143=CARTESIAN_POINT('Ctrl Pts',(95.6808838306992,0.885296495316674,-6.24106678465804));
#28144=CARTESIAN_POINT('Ctrl Pts',(95.626445505066,0.83161194890941,-6.23570647197124));
#28145=CARTESIAN_POINT('Ctrl Pts',(95.6194672107343,0.824554099799341,-6.23501607191353));
#28146=CARTESIAN_POINT('Ctrl Pts',(95.6098558098326,0.814584142833932,-6.23406159144968));
#28147=CARTESIAN_POINT('Ctrl Pts',(95.607147012134,0.811746047992397,-6.23379218353898));
#28148=CARTESIAN_POINT('Ctrl Pts',(95.6024926690338,0.806820497166007,-6.23332865759519));
#28149=CARTESIAN_POINT('Ctrl Pts',(95.6005404558491,0.804739431049845,-6.2331340456809));
#28150=CARTESIAN_POINT('Ctrl Pts',(95.5964307527875,0.800326440989442,-6.23272399221954));
#28151=CARTESIAN_POINT('Ctrl Pts',(95.594275098128,0.797992843385805,-6.2325086945338));
#28152=CARTESIAN_POINT('Ctrl Pts',(95.5889373682523,0.792167385344054,-6.23197496648532));
#28153=CARTESIAN_POINT('Ctrl Pts',(95.5857667682458,0.788665000759619,-6.23165738092683));
#28154=CARTESIAN_POINT('Ctrl Pts',(95.5738098886506,0.775296094781045,-6.23045716577272));
#28155=CARTESIAN_POINT('Ctrl Pts',(95.565168378576,0.765300621383421,-6.22958446358446));
#28156=CARTESIAN_POINT('Ctrl Pts',(95.5433302029879,0.739164478987613,-6.22735872991474));
#28157=CARTESIAN_POINT('Ctrl Pts',(95.5303902007487,0.722814583418428,-6.22601986943513));
#28158=CARTESIAN_POINT('Ctrl Pts',(95.4907716172202,0.66992890209069,-6.22182465452319));
#28159=CARTESIAN_POINT('Ctrl Pts',(95.4657592764875,0.632194723616556,-6.21902745778775));
#28160=CARTESIAN_POINT('Ctrl Pts',(95.4020667482809,0.522928430592512,-6.21120409595732));
#28161=CARTESIAN_POINT('Ctrl Pts',(95.3685312980728,0.448707803518177,-6.20618228758337));
#28162=CARTESIAN_POINT('Ctrl Pts',(95.3380358388676,0.357001057416308,-6.19988363956184));
#28163=CARTESIAN_POINT('Ctrl Pts',(95.3334587000167,0.342277073073985,-6.19887033907451));
#28164=CARTESIAN_POINT('Ctrl Pts',(95.3272073191105,0.320680329876448,-6.19737909877741));
#28165=CARTESIAN_POINT('Ctrl Pts',(95.32530372324,0.313875224646292,-6.19690850567546));
#28166=CARTESIAN_POINT('Ctrl Pts',(95.3220328984528,0.301763357924753,-6.19606949219819));
#28167=CARTESIAN_POINT('Ctrl Pts',(95.3206412410178,0.296463364273207,-6.19570186395337));
#28168=CARTESIAN_POINT('Ctrl Pts',(95.3178137632152,0.285380904872879,-6.19493203468788));
#28169=CARTESIAN_POINT('Ctrl Pts',(95.3163847382833,0.279596882509461,-6.19452962897953));
#28170=CARTESIAN_POINT('Ctrl Pts',(95.312764813897,0.264452544022053,-6.19347424777148));
#28171=CARTESIAN_POINT('Ctrl Pts',(95.3106445624014,0.255075967834139,-6.19281905832067));
#28172=CARTESIAN_POINT('Ctrl Pts',(95.3014159894006,0.211807967644579,-6.18978691945086));
#28173=CARTESIAN_POINT('Ctrl Pts',(95.295690441113,0.177642458967405,-6.18736724273637));
#28174=CARTESIAN_POINT('Ctrl Pts',(95.2832098098899,0.0758126820904066,
-6.1800764368519));
#28175=CARTESIAN_POINT('Ctrl Pts',(95.2807976416746,0.00776555586291238,
-6.1750941075766));
#28176=CARTESIAN_POINT('Ctrl Pts',(95.2855481287778,-0.0852039474893144,
-6.16826343550903));
#28177=CARTESIAN_POINT('Ctrl Pts',(95.2876341029811,-0.110259595075508,
-6.16642150066938));
#28178=CARTESIAN_POINT('Ctrl Pts',(95.2924675193683,-0.152076612366585,
-6.16336067574171));
#28179=CARTESIAN_POINT('Ctrl Pts',(95.2947784826401,-0.168880049028224,
-6.16213441156213));
#28180=CARTESIAN_POINT('Ctrl Pts',(95.3010894354126,-0.208420479074215,
-6.15926525802658));
#28181=CARTESIAN_POINT('Ctrl Pts',(95.3053967531312,-0.231102681213478,
-6.15763225098994));
#28182=CARTESIAN_POINT('Ctrl Pts',(95.3116583222109,-0.259494726059863,
-6.15561599368471));
#28183=CARTESIAN_POINT('Ctrl Pts',(95.3129929837369,-0.265334343893482,
-6.15520279585967));
#28184=CARTESIAN_POINT('Ctrl Pts',(95.3151674153232,-0.27452486360076,-6.15455513495145));
#28185=CARTESIAN_POINT('Ctrl Pts',(95.3159774505275,-0.277882590168632,
-6.15431907167494));
#28186=CARTESIAN_POINT('Ctrl Pts',(95.3175357960826,-0.284219765338305,
-6.15387465644792));
#28187=CARTESIAN_POINT('Ctrl Pts',(95.3182809854777,-0.287199827906534,
-6.15366614563864));
#28188=CARTESIAN_POINT('Ctrl Pts',(95.3200570385646,-0.294186126814854,
-6.15317839164159));
#28189=CARTESIAN_POINT('Ctrl Pts',(95.321097360191,-0.298189891762895,-6.15289968599989));
#28190=CARTESIAN_POINT('Ctrl Pts',(95.3245770466254,-0.311297632741616,
-6.15198968594972));
#28191=CARTESIAN_POINT('Ctrl Pts',(95.3271046737384,-0.320378095447187,
-6.15136314904091));
#28192=CARTESIAN_POINT('Ctrl Pts',(95.3417730365526,-0.370726343863668,
-6.14790576293948));
#28193=CARTESIAN_POINT('Ctrl Pts',(95.3560598869303,-0.411339709255548,
-6.14517852513907));
#28194=CARTESIAN_POINT('Ctrl Pts',(95.3840109161201,-0.47875307494232,-6.14061700839035));
#28195=CARTESIAN_POINT('Ctrl Pts',(95.3965346349489,-0.505974857824101,
-6.13876500369727));
#28196=CARTESIAN_POINT('Ctrl Pts',(95.4460162743963,-0.603546460294404,
-6.1319980489023));
#28197=CARTESIAN_POINT('Ctrl Pts',(95.4890221970525,-0.670576476632717,
-6.12708033453048));
#28198=CARTESIAN_POINT('Ctrl Pts',(95.5480689366773,-0.744874945999224,
-6.12089562403105));
#28199=CARTESIAN_POINT('Ctrl Pts',(95.5579308989155,-0.756794381829892,
-6.11987901299108));
#28200=CARTESIAN_POINT('Ctrl Pts',(95.572641433413,-0.773877328917242,-6.11838379939193));
#28201=CARTESIAN_POINT('Ctrl Pts',(95.5773066049556,-0.779197150933951,
-6.11791260021202));
#28202=CARTESIAN_POINT('Ctrl Pts',(95.5856701436583,-0.788562716622741,
-6.1170728917149));
#28203=CARTESIAN_POINT('Ctrl Pts',(95.5893493835353,-0.792625319501041,
-6.11670517909261));
#28204=CARTESIAN_POINT('Ctrl Pts',(95.5970839648839,-0.801046911589094,
-6.11593556534024));
#28205=CARTESIAN_POINT('Ctrl Pts',(95.6011442607899,-0.80540111795582,-6.11553346214387));
#28206=CARTESIAN_POINT('Ctrl Pts',(95.6118328261157,-0.81669054999094,-6.11447975630646));
#28207=CARTESIAN_POINT('Ctrl Pts',(95.618513013011,-0.823575786587198,-6.11382595265674));
#28208=CARTESIAN_POINT('Ctrl Pts',(95.6495323993175,-0.854775454429458,
-6.11081077782381));
#28209=CARTESIAN_POINT('Ctrl Pts',(95.6748433441457,-0.878095532601403,
-6.1084072655057));
#28210=CARTESIAN_POINT('Ctrl Pts',(95.7524612090611,-0.943563147588889,
-6.10119289820404));
#28211=CARTESIAN_POINT('Ctrl Pts',(95.8073889823616,-0.982380988018991,
-6.09627384408467));
#28212=CARTESIAN_POINT('Ctrl Pts',(95.9167433583124,-1.04642063506708,-6.08697431757348));
#28213=CARTESIAN_POINT('Ctrl Pts',(95.970386765049,-1.07259303998043,-6.08261109668552));
#28214=CARTESIAN_POINT('Ctrl Pts',(96.0350967775283,-1.09829128012328,-6.07772861390346));
#28215=CARTESIAN_POINT('Ctrl Pts',(96.0444549616281,-1.10187014832249,-6.07703156783505));
#28216=CARTESIAN_POINT('Ctrl Pts',(96.0575546989859,-1.10668921274995,-6.07606945828578));
#28217=CARTESIAN_POINT('Ctrl Pts',(96.0612582109591,-1.10803058762701,-6.07579895885625));
#28218=CARTESIAN_POINT('Ctrl Pts',(96.0676598361303,-1.11031292869552,-6.07533406840223));
#28219=CARTESIAN_POINT('Ctrl Pts',(96.0703547433169,-1.11126269191018,-6.0751391768499));
#28220=CARTESIAN_POINT('Ctrl Pts',(96.0760488470797,-1.11324619220005,-6.07472914397748));
#28221=CARTESIAN_POINT('Ctrl Pts',(96.0790488125957,-1.11427763649572,-6.07451414327494));
#28222=CARTESIAN_POINT('Ctrl Pts',(96.086505781488,-1.11680783784859,-6.0739821803486));
#28223=CARTESIAN_POINT('Ctrl Pts',(96.0909677225731,-1.11829206827427,-6.07366605074161));
#28224=CARTESIAN_POINT('Ctrl Pts',(96.1078466892266,-1.12379467265748,-6.07247794131675));
#28225=CARTESIAN_POINT('Ctrl Pts',(96.1203218682422,-1.12763346085623,-6.07161563310831));
#28226=CARTESIAN_POINT('Ctrl Pts',(96.15254473122,-1.13696542723526,-6.06942259602257));
#28227=CARTESIAN_POINT('Ctrl Pts',(96.1723772073523,-1.14215210488523,-6.06810552025532));
#28228=CARTESIAN_POINT('Ctrl Pts',(96.248628526104,-1.15998090245398,-6.06313080173876));
#28229=CARTESIAN_POINT('Ctrl Pts',(96.3058169985225,-1.16898118351778,-6.05958104630404));
#28230=CARTESIAN_POINT('Ctrl Pts',(96.4386392566096,-1.17996266025842,-6.05132873566836));
#28231=CARTESIAN_POINT('Ctrl Pts',(96.5142532006359,-1.17893819890441,-6.04661608460665));
#28232=CARTESIAN_POINT('Ctrl Pts',(96.5995711055442,-1.16955415778022,-6.0409828660632));
#28233=CARTESIAN_POINT('Ctrl Pts',(96.6098823391683,-1.16828173531115,-6.04029703995749));
#28234=CARTESIAN_POINT('Ctrl Pts',(96.6268386108504,-1.16596115915744,-6.03916030505212));
#28235=CARTESIAN_POINT('Ctrl Pts',(96.6334940401457,-1.16499217313702,-6.03871185575503));
#28236=CARTESIAN_POINT('Ctrl Pts',(96.6455059058222,-1.16313812567222,-6.03789820329052));
#28237=CARTESIAN_POINT('Ctrl Pts',(96.6508652524335,-1.16227292378605,-6.03753362973343));
#28238=CARTESIAN_POINT('Ctrl Pts',(96.6623553514322,-1.16033638269191,-6.03674859648554));
#28239=CARTESIAN_POINT('Ctrl Pts',(96.6684839537484,-1.15925344201018,-6.03632778345609));
#28240=CARTESIAN_POINT('Ctrl Pts',(96.6852571237432,-1.15615228740285,-6.03517018674572));
#28241=CARTESIAN_POINT('Ctrl Pts',(96.6958826554317,-1.15403572883338,-6.03443034356532));
#28242=CARTESIAN_POINT('Ctrl Pts',(96.7586666758923,-1.14062628720696,-6.03001873047136));
#28243=CARTESIAN_POINT('Ctrl Pts',(96.8100305438424,-1.12594700656359,-6.02624091054148));
#28244=CARTESIAN_POINT('Ctrl Pts',(96.9340457390375,-1.08119928844566,-6.01671173642312));
#28245=CARTESIAN_POINT('Ctrl Pts',(97.0050223430032,-1.04724839893012,-6.01088343267503));
#28246=CARTESIAN_POINT('Ctrl Pts',(97.0998905060409,-0.98960019688799,-6.00284912981804));
#28247=CARTESIAN_POINT('Ctrl Pts',(97.1269797058838,-0.971562123928781,
-6.00052625031948));
#28248=CARTESIAN_POINT('Ctrl Pts',(97.1585839164231,-0.948572701511742,
-5.99781069598665));
#28249=CARTESIAN_POINT('Ctrl Pts',(97.1638460934559,-0.944677406127372,
-5.99735837111901));
#28250=CARTESIAN_POINT('Ctrl Pts',(97.1719630714385,-0.938563434212828,
-5.9966607171686));
#28251=CARTESIAN_POINT('Ctrl Pts',(97.1748405000553,-0.936375225694146,
-5.99641341485543));
#28252=CARTESIAN_POINT('Ctrl Pts',(97.1800490161815,-0.932376303820347,
-5.99596585712887));
#28253=CARTESIAN_POINT('Ctrl Pts',(97.182383376658,-0.930570072886297,-5.99576531052032));
#28254=CARTESIAN_POINT('Ctrl Pts',(97.1847269553212,-0.928742583320426,
-5.99556400351155));
#28255=CARTESIAN_POINT('Ctrl Pts',(97.1847429039152,-0.928730146171248,
-5.9955626335721));
#28256=CARTESIAN_POINT('Ctrl Pts',(97.184774498043,-0.928705506898879,-5.99555991972768));
#28257=CARTESIAN_POINT('Ctrl Pts',(97.184790144265,-0.928693304263706,-5.99555857576354));
#28258=CARTESIAN_POINT('Ctrl Pts',(97.1848211446973,-0.928669125475988,
-5.99555591292053));
#28259=CARTESIAN_POINT('Ctrl Pts',(97.1848364985207,-0.928657149648654,
-5.99555459407484));
#28260=CARTESIAN_POINT('Ctrl Pts',(97.1848669215787,-0.928633418757059,
-5.995551980831));
#28261=CARTESIAN_POINT('Ctrl Pts',(97.1848819913527,-0.928621663294376,
-5.99555068638648));
#28262=CARTESIAN_POINT('Ctrl Pts',(97.1849118558488,-0.928598365759052,
-5.99554812112562));
#28263=CARTESIAN_POINT('Ctrl Pts',(97.1849266503091,-0.928586823911997,
-5.99554685033174));
#28264=CARTESIAN_POINT('Ctrl Pts',(97.1849559732172,-0.928563946619245,
-5.99554433159558));
#28265=CARTESIAN_POINT('Ctrl Pts',(97.1849705011142,-0.928552611623555,
-5.99554308370057));
#28266=CARTESIAN_POINT('Ctrl Pts',(97.1849992968908,-0.928530143416615,
-5.99554061024712));
#28267=CARTESIAN_POINT('Ctrl Pts',(97.1850135655155,-0.928519009643252,
-5.99553938462462));
#28268=CARTESIAN_POINT('Ctrl Pts',(97.1850418509155,-0.928496937565013,
-5.99553695501443));
#28269=CARTESIAN_POINT('Ctrl Pts',(97.1850558679194,-0.928485999100242,
-5.99553575100707));
#28270=CARTESIAN_POINT('Ctrl Pts',(97.1850836575746,-0.928464311843944,
-5.99553336398313));
#28271=CARTESIAN_POINT('Ctrl Pts',(97.1850974301347,-0.928453563141104,
-5.99553218097434));
#28272=CARTESIAN_POINT('Ctrl Pts',(97.1851247389717,-0.928432249163397,
-5.99552983525428));
#28273=CARTESIAN_POINT('Ctrl Pts',(97.185138274497,-0.928421684491844,-5.99552867260754));
#28274=CARTESIAN_POINT('Ctrl Pts',(97.1851651158827,-0.928400733460897,
-5.995526367043));
#28275=CARTESIAN_POINT('Ctrl Pts',(97.1851784215235,-0.928390347288889,
-5.99552522414402));
#28276=CARTESIAN_POINT('Ctrl Pts',(97.1852048066402,-0.9283697505729,-5.9955229577743));
#28277=CARTESIAN_POINT('Ctrl Pts',(97.1852178876494,-0.928359538847369,
-5.99552183417181));
#28278=CARTESIAN_POINT('Ctrl Pts',(97.1852438322286,-0.928339284258116,
-5.99551960564546));
#28279=CARTESIAN_POINT('Ctrl Pts',(97.1852566953784,-0.928329241737194,
-5.99551850075766));
#28280=CARTESIAN_POINT('Ctrl Pts',(97.1852822112146,-0.92830932015475,-5.99551630906141));
#28281=CARTESIAN_POINT('Ctrl Pts',(97.1852948631045,-0.928299441729095,
-5.99551522232134));
#28282=CARTESIAN_POINT('Ctrl Pts',(97.1853199600008,-0.928279845583848,
-5.99551306661298));
#28283=CARTESIAN_POINT('Ctrl Pts',(97.1853324055851,-0.928270127426433,
-5.99551199759503));
#28284=CARTESIAN_POINT('Ctrl Pts',(97.1853570971651,-0.928250846161321,
-5.9955098767042));
#28285=CARTESIAN_POINT('Ctrl Pts',(97.1853693425941,-0.928241283509049,
-5.99550882488));
#28286=CARTESIAN_POINT('Ctrl Pts',(97.188438685684,-0.925844286384764,-5.99524518304663));
#28287=CARTESIAN_POINT('Ctrl Pts',(97.191484024883,-0.923441721579667,-5.99498364406355));
#28288=CARTESIAN_POINT('Ctrl Pts',(97.1979193183567,-0.918312930149093,
-5.99443092295136));
#28289=CARTESIAN_POINT('Ctrl Pts',(97.2013061610469,-0.915582870579692,
-5.99414000233541));
#28290=CARTESIAN_POINT('Ctrl Pts',(97.2103567834104,-0.908204261977934,
-5.99336226312612));
#28291=CARTESIAN_POINT('Ctrl Pts',(97.2159925400035,-0.903521438907313,
-5.99287763580293));
#28292=CARTESIAN_POINT('Ctrl Pts',(97.2334556755209,-0.888733436358291,
-5.99137357042186));
#28293=CARTESIAN_POINT('Ctrl Pts',(97.2451272339687,-0.878445960104843,
-5.9903648493703));
#28294=CARTESIAN_POINT('Ctrl Pts',(97.2931014510356,-0.834441466236788,
-5.98618700847161));
#28295=CARTESIAN_POINT('Ctrl Pts',(97.3274643086825,-0.798680206876593,
-5.98311499050986));
#28296=CARTESIAN_POINT('Ctrl Pts',(97.4150047339152,-0.695246641984305,
-5.97472955877326));
#28297=CARTESIAN_POINT('Ctrl Pts',(97.4631787887382,-0.623761559067209,
-5.96943500998131));
#28298=CARTESIAN_POINT('Ctrl Pts',(97.5102240747314,-0.534196802675814,
-5.96283935810681));
#28299=CARTESIAN_POINT('Ctrl Pts',(97.5170415245034,-0.520582913475649,
-5.96183854300716));
#28300=CARTESIAN_POINT('Ctrl Pts',(97.5266187673362,-0.500494408964516,
-5.96036229672799));
#28301=CARTESIAN_POINT('Ctrl Pts',(97.529587658197,-0.494120776590511,-5.95989400045444));
#28302=CARTESIAN_POINT('Ctrl Pts',(97.5347663521593,-0.482737928510596,
-5.95905761462385));
#28303=CARTESIAN_POINT('Ctrl Pts',(97.5369986498103,-0.477739126703279,
-5.95869029992104));
#28304=CARTESIAN_POINT('Ctrl Pts',(97.5415941555605,-0.46725260495907,-5.95791962323901));
#28305=CARTESIAN_POINT('Ctrl Pts',(97.5439506114233,-0.461762114712368,
-5.95751604649715));
#28306=CARTESIAN_POINT('Ctrl Pts',(97.550019245722,-0.447320099982346,-5.95645418144808));
#28307=CARTESIAN_POINT('Ctrl Pts',(97.5536628327313,-0.438340428464417,
-5.95579362883106));
#28308=CARTESIAN_POINT('Ctrl Pts',(97.5701423286806,-0.396242643946171,
-5.95269466548414));
#28309=CARTESIAN_POINT('Ctrl Pts',(97.5815854644715,-0.362602837894717,
-5.95021117507097));
#28310=CARTESIAN_POINT('Ctrl Pts',(97.6225446599052,-0.22158247036711,-5.93976532406914));
#28311=CARTESIAN_POINT('Ctrl Pts',(97.6382756354914,-0.110826536906557,
-5.93141223446537));
#28312=CARTESIAN_POINT('Ctrl Pts',(97.6382308542487,0.000473862668674378,
-5.92345611052503));
#28313=CARTESIAN_POINT('Ctrl Pts',(97.6382308536216,0.00047541875814493,
-5.9234559992906));
#28314=CARTESIAN_POINT('Ctrl Pts',(97.6382224132776,0.0213845943457944,
-5.92196134253803));
#28315=CARTESIAN_POINT('Ctrl Pts',(97.6376571556521,0.0422916652363726,
-5.92048465166223));
#28316=CARTESIAN_POINT('Ctrl Pts',(97.6363006548358,0.0675443221931847,
-5.91873085816825));
#28317=CARTESIAN_POINT('Ctrl Pts',(97.636041549317,0.0719130901754064,-5.91842853155492));
#28318=CARTESIAN_POINT('Ctrl Pts',(97.6355535230143,0.0794322719830097,
-5.91791017054684));
#28319=CARTESIAN_POINT('Ctrl Pts',(97.6353362717538,0.0825833591550827,
-5.91769353855461));
#28320=CARTESIAN_POINT('Ctrl Pts',(97.6348986671935,0.0885789262473102,
-5.9172825417018));
#28321=CARTESIAN_POINT('Ctrl Pts',(97.6346806497204,0.0914235546101246,
-5.91708805167027));
#28322=CARTESIAN_POINT('Ctrl Pts',(97.6342245265763,0.0971039430504702,
-5.91670073301855));
#28323=CARTESIAN_POINT('Ctrl Pts',(97.6339864761895,0.0999396805640717,
-5.91650790191768));
#28324=CARTESIAN_POINT('Ctrl Pts',(97.6333984785972,0.106652162415221,-5.91605263369416));
#28325=CARTESIAN_POINT('Ctrl Pts',(97.6330395832733,0.110528119691324,-5.91579068513029));
#28326=CARTESIAN_POINT('Ctrl Pts',(97.6317054486579,0.124197833378635,-5.9148699201821));
#28327=CARTESIAN_POINT('Ctrl Pts',(97.6306266369606,0.133981397560573,-5.91421649116507));
#28328=CARTESIAN_POINT('Ctrl Pts',(97.6264401654554,0.168024730127037,-5.91195863660057));
#28329=CARTESIAN_POINT('Ctrl Pts',(97.6226994607609,0.192201748569384,-5.91038321946628));
#28330=CARTESIAN_POINT('Ctrl Pts',(97.5993060263675,0.317444132439284,-5.90228802715373));
#28331=CARTESIAN_POINT('Ctrl Pts',(97.567217343523,0.415728716761013,-5.89612095009754));
#28332=CARTESIAN_POINT('Ctrl Pts',(97.5080065308723,0.539399432810971,-5.88740242428797));
#28333=CARTESIAN_POINT('Ctrl Pts',(97.4919256242229,0.569546427275296,-5.88519756575344));
#28334=CARTESIAN_POINT('Ctrl Pts',(97.4696913734066,0.607191062969501,-5.88231623434587));
#28335=CARTESIAN_POINT('Ctrl Pts',(97.4647238466902,0.615372132313187,-5.88168204408834));
#28336=CARTESIAN_POINT('Ctrl Pts',(97.4565080558396,0.628538347127185,-5.88064785152489));
#28337=CARTESIAN_POINT('Ctrl Pts',(97.453320688939,0.633561125674799,-5.88025006379852));
#28338=CARTESIAN_POINT('Ctrl Pts',(97.4471228870298,0.643166236888714,-5.87948297266832));
#28339=CARTESIAN_POINT('Ctrl Pts',(97.4441182303692,0.647752127828456,-5.8791138888068));
#28340=CARTESIAN_POINT('Ctrl Pts',(97.4371570112647,0.658216639324499,-5.87826504099892));
#28341=CARTESIAN_POINT('Ctrl Pts',(97.4331792266071,0.664080817237229,-5.8777844974268));
#28342=CARTESIAN_POINT('Ctrl Pts',(97.4203169927848,0.682679223464562,-5.876244600224));
#28343=CARTESIAN_POINT('Ctrl Pts',(97.4112338498441,0.695273352541443,-5.87517783354379));
#28344=CARTESIAN_POINT('Ctrl Pts',(97.3562931934426,0.768360296896599,-5.86884081723093));
#28345=CARTESIAN_POINT('Ctrl Pts',(97.3049303409396,0.824474760709458,-5.86335568679117));
#28346=CARTESIAN_POINT('Ctrl Pts',(97.2061723055963,0.913394336994797,-5.85361578766679));
#28347=CARTESIAN_POINT('Ctrl Pts',(97.1610925994946,0.948413749704477,-5.84941185117743));
#28348=CARTESIAN_POINT('Ctrl Pts',(97.0996696954013,0.989350885420907,-5.84411220737891));
#28349=CARTESIAN_POINT('Ctrl Pts',(97.0854883460824,0.998370292918983,-5.84291629732138));
#28350=CARTESIAN_POINT('Ctrl Pts',(97.0645078536697,1.01109164855347,-5.84119191042594));
#28351=CARTESIAN_POINT('Ctrl Pts',(97.0578580918265,1.01503466930285,-5.84065179139598));
#28352=CARTESIAN_POINT('Ctrl Pts',(97.0472675919713,1.02117424736929,-5.83980226745843));
#28353=CARTESIAN_POINT('Ctrl Pts',(97.0433523559463,1.02341405717112,-5.83949048643955));
#28354=CARTESIAN_POINT('Ctrl Pts',(97.035943283143,1.02759629397588,-5.83890490824164));
#28355=CARTESIAN_POINT('Ctrl Pts',(97.0324522481458,1.02954352775238,-5.83863083032843));
#28356=CARTESIAN_POINT('Ctrl Pts',(97.0263133842871,1.03292680793241,-5.83815217512753));
#28357=CARTESIAN_POINT('Ctrl Pts',(97.0236698644401,1.03437052438671,-5.83794712518217));
#28358=CARTESIAN_POINT('Ctrl Pts',(97.0179843479686,1.03744732062911,-5.83750843196941));
#28359=CARTESIAN_POINT('Ctrl Pts',(97.0149406881814,1.03907717775735,-5.83727498836125));
#28360=CARTESIAN_POINT('Ctrl Pts',(97.0066029016581,1.04349493291057,-5.83663920173035));
#28361=CARTESIAN_POINT('Ctrl Pts',(97.0012945390218,1.04625595662263,-5.83623848429078));
#28362=CARTESIAN_POINT('Ctrl Pts',(96.9754782513966,1.05943472319369,-5.83430815259919));
#28363=CARTESIAN_POINT('Ctrl Pts',(96.9546876389131,1.06929138666187,-5.83280975205383));
#28364=CARTESIAN_POINT('Ctrl Pts',(96.8397446977243,1.119715414067,-5.82475639510858));
#28365=CARTESIAN_POINT('Ctrl Pts',(96.7408890138456,1.14846797841612,-5.81862247803248));
#28366=CARTESIAN_POINT('Ctrl Pts',(96.6125171454055,1.16821582236168,-5.81042245254633));
#28367=CARTESIAN_POINT('Ctrl Pts',(96.5853477319366,1.1714313221552,-5.80867680181951));
#28368=CARTESIAN_POINT('Ctrl Pts',(96.5391241512246,1.17527553822152,-5.8056709347373));
#28369=CARTESIAN_POINT('Ctrl Pts',(96.5201214162402,1.17639291599921,-5.80442503424251));
#28370=CARTESIAN_POINT('Ctrl Pts',(96.4933461522842,1.17731692707259,-5.80265134578002));
#28371=CARTESIAN_POINT('Ctrl Pts',(96.4855892312208,1.17750789284731,-5.80213536380762));
#28372=CARTESIAN_POINT('Ctrl Pts',(96.4722580457959,1.17770430441587,-5.8012446647939));
#28373=CARTESIAN_POINT('Ctrl Pts',(96.466684520839,1.17774684993088,-5.80087110235214));
#28374=CARTESIAN_POINT('Ctrl Pts',(96.4560331009796,1.17775254788481,-5.80015485636917));
#28375=CARTESIAN_POINT('Ctrl Pts',(96.4509553228979,1.17772242419563,-5.79981238888875));
#28376=CARTESIAN_POINT('Ctrl Pts',(96.4390552107819,1.17757486274269,-5.79900733783508));
#28377=CARTESIAN_POINT('Ctrl Pts',(96.4322334470866,1.17743097243756,-5.79854394809531));
#28378=CARTESIAN_POINT('Ctrl Pts',(96.4086894839268,1.1767296399401,-5.79693789664575));
#28379=CARTESIAN_POINT('Ctrl Pts',(96.3919788294519,1.17587516820561,-5.79578617651147));
#28380=CARTESIAN_POINT('Ctrl Pts',(96.2788656927806,1.1676720613959,-5.78790629559718));
#28381=CARTESIAN_POINT('Ctrl Pts',(96.1836823324974,1.1488332110388,-5.78081633474949));
#28382=CARTESIAN_POINT('Ctrl Pts',(96.0845430228272,1.11616558790066,-5.77316459701475));
#28383=CARTESIAN_POINT('Ctrl Pts',(96.0772174083829,1.11367140749982,-5.77259783640592));
#28384=CARTESIAN_POINT('Ctrl Pts',(96.0378803339102,1.09984405021605,-5.76954849044065));
#28385=CARTESIAN_POINT('Ctrl Pts',(96.0063435715721,1.08720180671491,-5.76708197271567));
#28386=CARTESIAN_POINT('Ctrl Pts',(95.9585707903413,1.06560881758346,-5.76335092717144));
#28387=CARTESIAN_POINT('Ctrl Pts',(95.9419261490843,1.05760908299373,-5.76205213037112));
#28388=CARTESIAN_POINT('Ctrl Pts',(95.9242497424212,1.04859575044457,-5.76067918647434));
#28389=CARTESIAN_POINT('Ctrl Pts',(95.9230251593067,1.04796862019487,-5.76058410531922));
#28390=CARTESIAN_POINT('Ctrl Pts',(95.921801673071,1.04733934307989,-5.76048914482438));
#28391=CARTESIAN_POINT('Ctrl Pts',(95.9218018640414,1.04733944130189,-5.66223110129989));
#28392=CARTESIAN_POINT('Ctrl Pts',(95.9751129005066,1.07475895711457,-5.66655880664564));
#28393=CARTESIAN_POINT('Ctrl Pts',(96.0304650866842,1.09808108406502,-5.67097997349678));
#28394=CARTESIAN_POINT('Ctrl Pts',(96.1368980474905,1.13362901486336,-5.67919426223618));
#28395=CARTESIAN_POINT('Ctrl Pts',(96.1874673220581,1.14685897108738,-5.68298204705487));
#28396=CARTESIAN_POINT('Ctrl Pts',(96.2455873631558,1.15800010053294,-5.68709805198905));
#28397=CARTESIAN_POINT('Ctrl Pts',(96.2524333381618,1.15924962089989,-5.68757916697497));
#28398=CARTESIAN_POINT('Ctrl Pts',(96.262898016566,1.16106393224263,-5.68830853645777));
#28399=CARTESIAN_POINT('Ctrl Pts',(96.2665088027049,1.16167262054602,-5.68855910466603));
#28400=CARTESIAN_POINT('Ctrl Pts',(96.2731245040068,1.16275615629704,-5.68901611823567));
#28401=CARTESIAN_POINT('Ctrl Pts',(96.2761284314487,1.16323620396293,-5.68922283961971));
#28402=CARTESIAN_POINT('Ctrl Pts',(96.2829144878416,1.16429371338558,-5.68968807155876));
#28403=CARTESIAN_POINT('Ctrl Pts',(96.2866975926095,1.16486438920441,-5.68994620397421));
#28404=CARTESIAN_POINT('Ctrl Pts',(96.2964831325831,1.16629179037074,-5.69061089048023));
#28405=CARTESIAN_POINT('Ctrl Pts',(96.3024896121094,1.16712063016978,-5.69101596064249));
#28406=CARTESIAN_POINT('Ctrl Pts',(96.3428624545419,1.172374325467,-5.69372068120018));
#28407=CARTESIAN_POINT('Ctrl Pts',(96.3774068425609,1.17532755755173,-5.6959477599496));
#28408=CARTESIAN_POINT('Ctrl Pts',(96.4402153744239,1.17791335521369,-5.69991982688038));
#28409=CARTESIAN_POINT('Ctrl Pts',(96.4684298611127,1.17806090739991,-5.70167604289869));
#28410=CARTESIAN_POINT('Ctrl Pts',(96.5653392229808,1.1750855806629,-5.70768745599493));
#28411=CARTESIAN_POINT('Ctrl Pts',(96.6337346523555,1.1669635713583,-5.71190245428575));
#28412=CARTESIAN_POINT('Ctrl Pts',(96.7236338575945,1.14820677606705,-5.71773762997425));
#28413=CARTESIAN_POINT('Ctrl Pts',(96.7460932749141,1.14282708771586,-5.71921978550804));
#28414=CARTESIAN_POINT('Ctrl Pts',(96.7845562063631,1.1324094615372,-5.72181122197745));
#28415=CARTESIAN_POINT('Ctrl Pts',(96.8006372842522,1.12768328134515,-5.72291100719064));
#28416=CARTESIAN_POINT('Ctrl Pts',(96.8236480241402,1.12038352149864,-5.7245109946853));
#28417=CARTESIAN_POINT('Ctrl Pts',(96.8306633537164,1.11808521268099,-5.7250023436126));
#28418=CARTESIAN_POINT('Ctrl Pts',(96.842874904989,1.11395703211738,-5.72586408182899));
#28419=CARTESIAN_POINT('Ctrl Pts',(96.8480808097367,1.11215635285133,-5.7262335121111));
#28420=CARTESIAN_POINT('Ctrl Pts',(96.858143522423,1.10859651023689,-5.72695169341057));
#28421=CARTESIAN_POINT('Ctrl Pts',(96.8630017741062,1.10684178124442,-5.72730029190871));
#28422=CARTESIAN_POINT('Ctrl Pts',(96.8759131412568,1.10208213753629,-5.72823179229434));
#28423=CARTESIAN_POINT('Ctrl Pts',(96.8839450435126,1.0990209725564,-5.72881653361714));
#28424=CARTESIAN_POINT('Ctrl Pts',(96.9133216651725,1.08745494921108,-5.73097511408993));
#28425=CARTESIAN_POINT('Ctrl Pts',(96.9344485038801,1.07841439637011,-5.73256650408518));
#28426=CARTESIAN_POINT('Ctrl Pts',(97.0473751696591,1.02613164001487,-5.74129221035787));
#28427=CARTESIAN_POINT('Ctrl Pts',(97.1335479907659,0.971784402148248,-5.74880368552043));
#28428=CARTESIAN_POINT('Ctrl Pts',(97.2348101072412,0.887925644902729,-5.75839429059497));
#28429=CARTESIAN_POINT('Ctrl Pts',(97.2572081820215,0.867884528658782,-5.76056830569385));
#28430=CARTESIAN_POINT('Ctrl Pts',(97.2870494042917,0.839053453328704,-5.76351482141321));
#28431=CARTESIAN_POINT('Ctrl Pts',(97.2951660967796,0.830979442941155,-5.76432167805576));
#28432=CARTESIAN_POINT('Ctrl Pts',(97.3090608174001,0.816748746452408,-5.76571049998446));
#28433=CARTESIAN_POINT('Ctrl Pts',(97.314892653803,0.810646012011345,-5.76629581896176));
#28434=CARTESIAN_POINT('Ctrl Pts',(97.3233612145196,0.801591146244275,-5.76714866373568));
#28435=CARTESIAN_POINT('Ctrl Pts',(97.3260493192466,0.798687746204728,-5.76741981189418));
#28436=CARTESIAN_POINT('Ctrl Pts',(97.3307841738626,0.793521687238794,-5.76789810551688));
#28437=CARTESIAN_POINT('Ctrl Pts',(97.3328368210176,0.791264560465882,-5.76810568314704));
#28438=CARTESIAN_POINT('Ctrl Pts',(97.3372666061745,0.786355300402215,-5.76855413657115));
#28439=CARTESIAN_POINT('Ctrl Pts',(97.3396404981839,0.783700347722821,-5.7687947757105));
#28440=CARTESIAN_POINT('Ctrl Pts',(97.3461870699038,0.776311503625451,-5.76945941157289));
#28441=CARTESIAN_POINT('Ctrl Pts',(97.3503338776922,0.771554698594552,-5.76988156999867));
#28442=CARTESIAN_POINT('Ctrl Pts',(97.3730498177602,0.74507046570746,-5.77220208953741));
#28443=CARTESIAN_POINT('Ctrl Pts',(97.3908631711767,0.722704062826822,-5.77405167845208));
#28444=CARTESIAN_POINT('Ctrl Pts',(97.4564965076343,0.633840395969172,-5.78108366123805));
#28445=CARTESIAN_POINT('Ctrl Pts',(97.4981468236522,0.563073650517971,-5.78604378228458));
#28446=CARTESIAN_POINT('Ctrl Pts',(97.5546267303585,0.439185480955545,-5.79455302259547));
#28447=CARTESIAN_POINT('Ctrl Pts',(97.5736925800913,0.388326682819808,-5.79799958116884));
#28448=CARTESIAN_POINT('Ctrl Pts',(97.5922895461358,0.325918098068583,-5.80227919122276));
#28449=CARTESIAN_POINT('Ctrl Pts',(97.5952503505255,0.315454750547279,-5.80299818705806));
#28450=CARTESIAN_POINT('Ctrl Pts',(97.599679363699,0.298932887760326,-5.80413652162038));
#28451=CARTESIAN_POINT('Ctrl Pts',(97.6012451288838,0.292900977833946,-5.80455273966153));
#28452=CARTESIAN_POINT('Ctrl Pts',(97.6040848457101,0.281593054039978,-5.80533432073931));
#28453=CARTESIAN_POINT('Ctrl Pts',(97.6053703444761,0.276320088110755,-5.80569930503148));
#28454=CARTESIAN_POINT('Ctrl Pts',(97.6081641885741,0.26450578143945,-5.80651833698623));
#28455=CARTESIAN_POINT('Ctrl Pts',(97.6096531351444,0.257960094166874,-5.80697298646781));
#28456=CARTESIAN_POINT('Ctrl Pts',(97.6132950031252,0.241292170957103,-5.80813306947874));
#28457=CARTESIAN_POINT('Ctrl Pts',(97.6153705807465,0.231153805496216,-5.80884090761837));
#28458=CARTESIAN_POINT('Ctrl Pts',(97.6312955305549,0.14779027378089,-5.81468069717354));
#28459=CARTESIAN_POINT('Ctrl Pts',(97.6382972287035,0.0734425629974218,
-5.82002849412964));
#28460=CARTESIAN_POINT('Ctrl Pts',(97.6381596114607,-0.08014390216321,-5.83125971083814));
#28461=CARTESIAN_POINT('Ctrl Pts',(97.6301226225534,-0.159027589705757,
-5.83712704988531));
#28462=CARTESIAN_POINT('Ctrl Pts',(97.6116248238539,-0.249263388658251,
-5.8436258323391));
#28463=CARTESIAN_POINT('Ctrl Pts',(97.6087998454002,-0.261969854422392,
-5.84453549485481));
#28464=CARTESIAN_POINT('Ctrl Pts',(97.6046353006604,-0.279337325100714,
-5.84576900199256));
#28465=CARTESIAN_POINT('Ctrl Pts',(97.6034768683157,-0.284040229718555,
-5.84610202357358));
#28466=CARTESIAN_POINT('Ctrl Pts',(97.6015824904897,-0.291531560896638,
-5.84663076159496));
#28467=CARTESIAN_POINT('Ctrl Pts',(97.6008652746701,-0.294324598377501,
-5.84682750753017));
#28468=CARTESIAN_POINT('Ctrl Pts',(97.5993443178567,-0.30015859794374,-5.8472376144273));
#28469=CARTESIAN_POINT('Ctrl Pts',(97.5985386431533,-0.303199013760541,
-5.84745085529625));
#28470=CARTESIAN_POINT('Ctrl Pts',(97.5965327927153,-0.310647947196378,
-5.84797216986756));
#28471=CARTESIAN_POINT('Ctrl Pts',(97.5953191086098,-0.315052839883116,
-5.84827948364811));
#28472=CARTESIAN_POINT('Ctrl Pts',(97.5907938302741,-0.331111189825382,
-5.84939667298815));
#28473=CARTESIAN_POINT('Ctrl Pts',(97.5873279853533,-0.342720898745185,
-5.85019830380809));
#28474=CARTESIAN_POINT('Ctrl Pts',(97.5781189845763,-0.371917299589439,
-5.85220373708087));
#28475=CARTESIAN_POINT('Ctrl Pts',(97.5721393386185,-0.389426447013213,
-5.85339665234328));
#28476=CARTESIAN_POINT('Ctrl Pts',(97.5430920787854,-0.468349590123832,
-5.85875973596306));
#28477=CARTESIAN_POINT('Ctrl Pts',(97.5153296619533,-0.527914381370928,
-5.86277357260598));
#28478=CARTESIAN_POINT('Ctrl Pts',(97.4475888539103,-0.646317465626108,
-5.8712297563051));
#28479=CARTESIAN_POINT('Ctrl Pts',(97.4069629838279,-0.70447006052,-5.87566738503542));
#28480=CARTESIAN_POINT('Ctrl Pts',(97.3546402894488,-0.766604944021316,
-5.88099798617316));
#28481=CARTESIAN_POINT('Ctrl Pts',(97.3478096233866,-0.774501051359329,
-5.88168713099483));
#28482=CARTESIAN_POINT('Ctrl Pts',(97.3363975636134,-0.787344007577879,
-5.88282821142463));
#28483=CARTESIAN_POINT('Ctrl Pts',(97.3318769712508,-0.792344288333332,
-5.8832776540684));
#28484=CARTESIAN_POINT('Ctrl Pts',(97.323638199661,-0.801301505600868,-5.88409233983769));
#28485=CARTESIAN_POINT('Ctrl Pts',(97.3199350820164,-0.805272086811368,
-5.88445694559869));
#28486=CARTESIAN_POINT('Ctrl Pts',(97.311936751896,-0.813730092694751,-5.88524119357729));
#28487=CARTESIAN_POINT('Ctrl Pts',(97.3076332428558,-0.818209408709606,
-5.88566118304231));
#28488=CARTESIAN_POINT('Ctrl Pts',(97.2957644002983,-0.830369098362103,
-5.88681427867046));
#28489=CARTESIAN_POINT('Ctrl Pts',(97.288128884719,-0.837979811584242,-5.88755040507936));
#28490=CARTESIAN_POINT('Ctrl Pts',(97.2428859115296,-0.881854223154703,
-5.8918806536321));
#28491=CARTESIAN_POINT('Ctrl Pts',(97.2030087229751,-0.915683085681758,
-5.89557619288589));
#28492=CARTESIAN_POINT('Ctrl Pts',(97.0995241842134,-0.992255868331486,
-5.90487297801863));
#28493=CARTESIAN_POINT('Ctrl Pts',(97.0337423295437,-1.0316580336404,-5.91054821157257));
#28494=CARTESIAN_POINT('Ctrl Pts',(96.9325306807919,-1.07959428336482,-5.91867330416047));
#28495=CARTESIAN_POINT('Ctrl Pts',(96.8997803342307,-1.09333039034675,-5.92121461183439));
#28496=CARTESIAN_POINT('Ctrl Pts',(96.8607333041868,-1.10766885168813,-5.92410611400547));
#28497=CARTESIAN_POINT('Ctrl Pts',(96.8549938688502,-1.10972599898721,-5.92452769180868));
#28498=CARTESIAN_POINT('Ctrl Pts',(96.845617633187,-1.11300472228518,-5.92521052811567));
#28499=CARTESIAN_POINT('Ctrl Pts',(96.8419904693556,-1.11425323165662,-5.92547325743078));
#28500=CARTESIAN_POINT('Ctrl Pts',(96.8354755622793,-1.116460191735,-5.92594252804679));
#28501=CARTESIAN_POINT('Ctrl Pts',(96.832590153211,-1.11742519235339,-5.92614943843938));
#28502=CARTESIAN_POINT('Ctrl Pts',(96.8262320099972,-1.11952426022755,-5.92660333746621));
#28503=CARTESIAN_POINT('Ctrl Pts',(96.8227577226697,-1.12065335765313,-5.92685003909689));
#28504=CARTESIAN_POINT('Ctrl Pts',(96.8126892865827,-1.12387374946385,-5.92756130759393));
#28505=CARTESIAN_POINT('Ctrl Pts',(96.8060817582553,-1.12592317860074,-5.92802354564298));
#28506=CARTESIAN_POINT('Ctrl Pts',(96.7514813399379,-1.14233240293969,-5.93180883078943));
#28507=CARTESIAN_POINT('Ctrl Pts',(96.702628665276,-1.15367688326447,-5.93497861184306));
#28508=CARTESIAN_POINT('Ctrl Pts',(96.5763889960245,-1.17461568911899,-5.94296005245186));
#28509=CARTESIAN_POINT('Ctrl Pts',(96.498510344349,-1.1797077471644,-5.94769956346187));
#28510=CARTESIAN_POINT('Ctrl Pts',(96.3836244399372,-1.1758249117246,-5.95498205271896));
#28511=CARTESIAN_POINT('Ctrl Pts',(96.3466332245655,-1.1728211359748,-5.95736908685501));
#28512=CARTESIAN_POINT('Ctrl Pts',(96.2997322596512,-1.16677287862026,-5.96048128352236));
#28513=CARTESIAN_POINT('Ctrl Pts',(96.2896342031307,-1.16533706287848,-5.96115640114669));
#28514=CARTESIAN_POINT('Ctrl Pts',(96.2735430830912,-1.16283546968183,-5.96224083626712));
#28515=CARTESIAN_POINT('Ctrl Pts',(96.2675372773464,-1.16185404955828,-5.96264751785578));
#28516=CARTESIAN_POINT('Ctrl Pts',(96.2561699742928,-1.15990592974048,-5.96342103750785));
#28517=CARTESIAN_POINT('Ctrl Pts',(96.250807035844,-1.15894848404034,-5.96378757638779));
#28518=CARTESIAN_POINT('Ctrl Pts',(96.2386302914167,-1.15668728463125,-5.96462355704434));
#28519=CARTESIAN_POINT('Ctrl Pts',(96.2318210271839,-1.15536047417377,-5.96509371184269));
#28520=CARTESIAN_POINT('Ctrl Pts',(96.2109900773673,-1.15111012413355,-5.96654043305423));
#28521=CARTESIAN_POINT('Ctrl Pts',(96.1970101161149,-1.14799098506005,-5.9675231006559));
#28522=CARTESIAN_POINT('Ctrl Pts',(96.1293686296342,-1.13159855558318,-5.97233705223512));
#28523=CARTESIAN_POINT('Ctrl Pts',(96.0766371957147,-1.11481526090167,-5.97627734729979));
#28524=CARTESIAN_POINT('Ctrl Pts',(96.0087311372148,-1.08781181259783,-5.98158497952861));
#28525=CARTESIAN_POINT('Ctrl Pts',(95.9923289587445,-1.08085434687124,-5.98288536168809));
#28526=CARTESIAN_POINT('Ctrl Pts',(95.9021463523877,-1.04016277809069,-5.99012804347023));
#28527=CARTESIAN_POINT('Ctrl Pts',(95.8318417451423,-0.999245121751286,
-5.99614220333807));
#28528=CARTESIAN_POINT('Ctrl Pts',(95.7594468072158,-0.946423857211277,
-6.00241446591645));
#28529=CARTESIAN_POINT('Ctrl Pts',(95.7526497150005,-0.94135112457957,-6.00300402275569));
#28530=CARTESIAN_POINT('Ctrl Pts',(95.7423238777272,-0.933469769071108,
-6.00389994466016));
#28531=CARTESIAN_POINT('Ctrl Pts',(95.7387556410253,-0.930713688673121,
-6.00420959730892));
#28532=CARTESIAN_POINT('Ctrl Pts',(95.7327587544793,-0.926026508948025,
-6.00472997848996));
#28533=CARTESIAN_POINT('Ctrl Pts',(95.7303217721668,-0.924106197905514,
-6.00494143900239));
#28534=CARTESIAN_POINT('Ctrl Pts',(95.7253150869039,-0.92012882305955,-6.00537581188725));
#28535=CARTESIAN_POINT('Ctrl Pts',(95.7227463794406,-0.918070586264534,
-6.00559863937361));
#28536=CARTESIAN_POINT('Ctrl Pts',(95.7160990673194,-0.912698357915788,
-6.00617529583538));
#28537=CARTESIAN_POINT('Ctrl Pts',(95.7120338989592,-0.90936774418891,-6.00652797270699));
#28538=CARTESIAN_POINT('Ctrl Pts',(95.6944015633905,-0.894723143351059,
-6.00805846434382));
#28539=CARTESIAN_POINT('Ctrl Pts',(95.6810668262231,-0.883131267123109,
-6.00921797313003));
#28540=CARTESIAN_POINT('Ctrl Pts',(95.6445169961382,-0.849885491410347,
-6.01241860812787));
#28541=CARTESIAN_POINT('Ctrl Pts',(95.6219081173027,-0.827585897682627,
-6.01442508734404));
#28542=CARTESIAN_POINT('Ctrl Pts',(95.5831667469715,-0.786154395061466,
-6.01797186058589));
#28543=CARTESIAN_POINT('Ctrl Pts',(95.566691478387,-0.767371732940789,-6.01951938595918));
#28544=CARTESIAN_POINT('Ctrl Pts',(95.4966602615577,-0.682214597378204,
-6.02634163973363));
#28545=CARTESIAN_POINT('Ctrl Pts',(95.4498147219456,-0.610670738457653,
-6.03159699690171));
#28546=CARTESIAN_POINT('Ctrl Pts',(95.4041781380538,-0.521106713352949,
-6.03815005201377));
#28547=CARTESIAN_POINT('Ctrl Pts',(95.397516541759,-0.50738000485435,-6.03915294986812));
#28548=CARTESIAN_POINT('Ctrl Pts',(95.3881750283886,-0.487139188377189,
-6.04063167420698));
#28549=CARTESIAN_POINT('Ctrl Pts',(95.3852837248031,-0.48072393503152,-6.04110033046827));
#28550=CARTESIAN_POINT('Ctrl Pts',(95.3802453364569,-0.469271838329592,
-6.04193710082632));
#28551=CARTESIAN_POINT('Ctrl Pts',(95.3780755433262,-0.464245164644548,
-6.04230443719358));
#28552=CARTESIAN_POINT('Ctrl Pts',(95.3736127033821,-0.453704897874547,
-6.04307489387727));
#28553=CARTESIAN_POINT('Ctrl Pts',(95.3713263884722,-0.448188641871719,
-6.04347822714097));
#28554=CARTESIAN_POINT('Ctrl Pts',(95.3654454394189,-0.433688735638682,
-6.04453884700305));
#28555=CARTESIAN_POINT('Ctrl Pts',(95.3619194579964,-0.424677910251511,
-6.04519838854339));
#28556=CARTESIAN_POINT('Ctrl Pts',(95.3460284655378,-0.382544986985547,
-6.04828502867238));
#28557=CARTESIAN_POINT('Ctrl Pts',(95.3350490270743,-0.348923404741576,
-6.05075676979272));
#28558=CARTESIAN_POINT('Ctrl Pts',(95.3091133940262,-0.255441513658896,
-6.05765645693756));
#28559=CARTESIAN_POINT('Ctrl Pts',(95.2973215400775,-0.19482389157392,-6.06216530922561));
#28560=CARTESIAN_POINT('Ctrl Pts',(95.2830716488148,-0.0699851970086391,
-6.07138696368523));
#28561=CARTESIAN_POINT('Ctrl Pts',(95.2810076555278,-0.00590972651939632,
-6.07608536700387));
#28562=CARTESIAN_POINT('Ctrl Pts',(95.2846532215387,0.0680002942624265,
-6.0812742434572));
#28563=CARTESIAN_POINT('Ctrl Pts',(95.2852724147278,0.0779730858810877,
-6.08196936667564));
#28564=CARTESIAN_POINT('Ctrl Pts',(95.2863122156596,0.0918603519664206,
-6.08292925626069));
#28565=CARTESIAN_POINT('Ctrl Pts',(95.2866256207638,0.0957820865274885,
-6.08319942721361));
#28566=CARTESIAN_POINT('Ctrl Pts',(95.2872004482296,0.102547960475035,-6.08366389577261));
#28567=CARTESIAN_POINT('Ctrl Pts',(95.2874525730672,0.10539282416953,-6.08385869196536));
#28568=CARTESIAN_POINT('Ctrl Pts',(95.2880066725187,0.111396596054765,-6.08426869253285));
#28569=CARTESIAN_POINT('Ctrl Pts',(95.28831107007,0.11455525302986,-6.08448375541922));
#28570=CARTESIAN_POINT('Ctrl Pts',(95.2890987636025,0.122396896150111,-6.08501615447631));
#28571=CARTESIAN_POINT('Ctrl Pts',(95.2895973855799,0.127078350799416,-6.08533265484531));
#28572=CARTESIAN_POINT('Ctrl Pts',(95.2915888597733,0.144768031462634,-6.08652395838492));
#28573=CARTESIAN_POINT('Ctrl Pts',(95.2932705925018,0.157754613208788,-6.08738902227571));
#28574=CARTESIAN_POINT('Ctrl Pts',(95.2981528161411,0.191081768161256,-6.08959074361957));
#28575=CARTESIAN_POINT('Ctrl Pts',(95.3016708081423,0.211371920667645,-6.09091361081455));
#28576=CARTESIAN_POINT('Ctrl Pts',(95.3170661007777,0.288146203006812,-6.09588715099225));
#28577=CARTESIAN_POINT('Ctrl Pts',(95.3325575505042,0.343824592369923,-6.0994308518145));
#28578=CARTESIAN_POINT('Ctrl Pts',(95.3775621783982,0.469114566228311,-6.10767410206813));
#28579=CARTESIAN_POINT('Ctrl Pts',(95.409807556875,0.537461401389556,-6.11238387805394));
#28580=CARTESIAN_POINT('Ctrl Pts',(95.4536733280804,0.611180333613756,-6.11801384643724));
#28581=CARTESIAN_POINT('Ctrl Pts',(95.4591034105055,0.620037095624473,-6.1186996333092));
#28582=CARTESIAN_POINT('Ctrl Pts',(95.4682404535251,0.634506964100623,-6.11983629604845));
#28583=CARTESIAN_POINT('Ctrl Pts',(95.4718796737029,0.640162326046138,-6.12028471264617));
#28584=CARTESIAN_POINT('Ctrl Pts',(95.4785435096522,0.65032560519661,-6.12109830057862));
#28585=CARTESIAN_POINT('Ctrl Pts',(95.4815512582076,0.654844398594778,-6.12146284236517));
#28586=CARTESIAN_POINT('Ctrl Pts',(95.4880738875715,0.664498527500613,-6.12224780103712));
#28587=CARTESIAN_POINT('Ctrl Pts',(95.4915984334809,0.669627101248582,-6.12266857115714));
#28588=CARTESIAN_POINT('Ctrl Pts',(95.5013694303232,0.683606249670348,-6.12382603235099));
#28589=CARTESIAN_POINT('Ctrl Pts',(95.5076974777963,0.692398767520332,-6.12456578209746));
#28590=CARTESIAN_POINT('Ctrl Pts',(95.5459048791662,0.74397041321109,-6.12897620245101));
#28591=CARTESIAN_POINT('Ctrl Pts',(95.5805353828447,0.784624554238826,-6.13275285778048));
#28592=CARTESIAN_POINT('Ctrl Pts',(95.6513005757577,0.857100985021329,-6.14007408115646));
#28593=CARTESIAN_POINT('Ctrl Pts',(95.6868671642407,0.889334725291908,-6.14359614494818));
#28594=CARTESIAN_POINT('Ctrl Pts',(95.7463154850342,0.936940998695649,-6.14918395913571));
#28595=CARTESIAN_POINT('Ctrl Pts',(95.7689605264007,0.953776883903202,-6.15124988896251));
#28596=CARTESIAN_POINT('Ctrl Pts',(95.8207187335665,0.989444214867675,-6.15580728664749));
#28597=CARTESIAN_POINT('Ctrl Pts',(95.8501054047277,1.00783815029033,-6.15828628935765));
#28598=CARTESIAN_POINT('Ctrl Pts',(95.885539553619,1.02789795921767,-6.16111643693731));
#28599=CARTESIAN_POINT('Ctrl Pts',(95.890838935762,1.03084421874284,-6.16153565262914));
#28600=CARTESIAN_POINT('Ctrl Pts',(95.8995189946897,1.03558263038677,-6.1622154403622));
#28601=CARTESIAN_POINT('Ctrl Pts',(95.9028859895067,1.03739942198447,-6.1624774621797));
#28602=CARTESIAN_POINT('Ctrl Pts',(95.9089460211027,1.04063131763476,-6.16294599164961));
#28603=CARTESIAN_POINT('Ctrl Pts',(95.9116357334695,1.0420524199697,-6.16315286305428));
#28604=CARTESIAN_POINT('Ctrl Pts',(95.9168165849491,1.04476408419073,-6.16354925492291));
#28605=CARTESIAN_POINT('Ctrl Pts',(95.9193068175126,1.04605616108533,-6.16373887357585));
#28606=CARTESIAN_POINT('Ctrl Pts',(95.9218016730721,1.04733934308042,-6.16392795844921));
#28607=CARTESIAN_POINT('Origin',(96.460480949577,-7.19464945638997E-16,
0.924367114736168));
#28608=CARTESIAN_POINT('',(95.9218016727113,1.04733934289485,-6.7620578065779));
#28609=CARTESIAN_POINT('',(95.9218016806086,1.04733934695669,-6.66223764680097));
#28610=CARTESIAN_POINT('',(95.9218016730721,1.04733934308042,0.924367114736168));
#28611=CARTESIAN_POINT('Ctrl Pts',(95.9218016727113,1.04733934289486,-6.7620578065779));
#28612=CARTESIAN_POINT('Ctrl Pts',(95.8770371194504,1.02431553753191,-6.75890350241157));
#28613=CARTESIAN_POINT('Ctrl Pts',(95.8337985320487,0.998447554458193,-6.75569629601541));
#28614=CARTESIAN_POINT('Ctrl Pts',(95.7834943659939,0.963794505789377,-6.75168090394736));
#28615=CARTESIAN_POINT('Ctrl Pts',(95.7747235353619,0.957573725666344,-6.75096979162344));
#28616=CARTESIAN_POINT('Ctrl Pts',(95.7610269580201,0.947574635754814,-6.74984111488974));
#28617=CARTESIAN_POINT('Ctrl Pts',(95.7560436588742,0.943875880405588,-6.74942658133005));
#28618=CARTESIAN_POINT('Ctrl Pts',(95.7467549464507,0.936866984251905,-6.74864645378421));
#28619=CARTESIAN_POINT('Ctrl Pts',(95.7424427278433,0.933566100582952,-6.74828122455537));
#28620=CARTESIAN_POINT('Ctrl Pts',(95.7328219697637,0.926095587260169,-6.74745938926478));
#28621=CARTESIAN_POINT('Ctrl Pts',(95.7275261751977,0.921909932195247,-6.74700216308137));
#28622=CARTESIAN_POINT('Ctrl Pts',(95.7141084267697,0.91111621041443,-6.74583110095309));
#28623=CARTESIAN_POINT('Ctrl Pts',(95.7060382225205,0.904445051402049,-6.74511478153101));
#28624=CARTESIAN_POINT('Ctrl Pts',(95.64241746702,0.85040954813092,-6.73936978293451));
#28625=CARTESIAN_POINT('Ctrl Pts',(95.5913011040246,0.798089670711083,-6.73413479314144));
#28626=CARTESIAN_POINT('Ctrl Pts',(95.5122470941611,0.700510562234574,-6.72495563380379));
#28627=CARTESIAN_POINT('Ctrl Pts',(95.4819076367488,0.657462410372481,-6.72107325774696));
#28628=CARTESIAN_POINT('Ctrl Pts',(95.4350517157121,0.580512826719415,-6.71452929555936));
#28629=CARTESIAN_POINT('Ctrl Pts',(95.4170933497884,0.547579384063923,-6.71184211918865));
#28630=CARTESIAN_POINT('Ctrl Pts',(95.3978770438336,0.507947746161185,-6.70878235784957));
#28631=CARTESIAN_POINT('Ctrl Pts',(95.3950682017809,0.502029536064706,-6.70832987232336));
#28632=CARTESIAN_POINT('Ctrl Pts',(95.3908027257513,0.492845152670233,-6.70763482944402));
#28633=CARTESIAN_POINT('Ctrl Pts',(95.3893113955276,0.489595378216683,-6.70739027261354));
#28634=CARTESIAN_POINT('Ctrl Pts',(95.3865756224066,0.483561485219329,-6.70693881126955));
#28635=CARTESIAN_POINT('Ctrl Pts',(95.3853271949711,0.480779331932569,-6.70673167829666));
#28636=CARTESIAN_POINT('Ctrl Pts',(95.3824916276898,0.474393914186683,-6.70625860540465));
#28637=CARTESIAN_POINT('Ctrl Pts',(95.3809117382395,0.470787513613135,-6.70599310093264));
#28638=CARTESIAN_POINT('Ctrl Pts',(95.3767973173392,0.461265931236913,-6.70529636298389));
#28639=CARTESIAN_POINT('Ctrl Pts',(95.3742930880558,0.455337685803935,-6.70486686023385));
#28640=CARTESIAN_POINT('Ctrl Pts',(95.350748802712,0.398301734954217,-6.70077285439712));
#28641=CARTESIAN_POINT('Ctrl Pts',(95.3332793260234,0.345785903789721,-6.69729505969813));
#28642=CARTESIAN_POINT('Ctrl Pts',(95.3174223898593,0.283877687875081,-6.69332141647806));
#28643=CARTESIAN_POINT('Ctrl Pts',(95.3153746662151,0.275501387219925,-6.69278642430557));
#28644=CARTESIAN_POINT('Ctrl Pts',(95.2981235502004,0.201417327575342,-6.68807267907344));
#28645=CARTESIAN_POINT('Ctrl Pts',(95.2884991461971,0.134542665200355,-6.68393349144852));
#28646=CARTESIAN_POINT('Ctrl Pts',(95.2826823498589,0.0327840150691671,
-6.67745481190683));
#28647=CARTESIAN_POINT('Ctrl Pts',(95.28222756025,-0.00171249894724128,
-6.67522918194241));
#28648=CARTESIAN_POINT('Ctrl Pts',(95.2835816054693,-0.0457730014912438,
-6.67232426632857));
#28649=CARTESIAN_POINT('Ctrl Pts',(95.2839938235383,-0.0553648545971774,
-6.67168814806046));
#28650=CARTESIAN_POINT('Ctrl Pts',(95.2848516661288,-0.0708965079276218,
-6.67065158941566));
#28651=CARTESIAN_POINT('Ctrl Pts',(95.2852251720243,-0.0768399769841434,
-6.67025338279986));
#28652=CARTESIAN_POINT('Ctrl Pts',(95.2860289396269,-0.0882472378186994,
-6.6694860163606));
#28653=CARTESIAN_POINT('Ctrl Pts',(95.2864522976471,-0.0937113726519938,
-6.66911707997508));
#28654=CARTESIAN_POINT('Ctrl Pts',(95.2875092817689,-0.106219322765645,
-6.66826932806204));
#28655=CARTESIAN_POINT('Ctrl Pts',(95.2881682430029,-0.113260726815666,
-6.66778973968609));
#28656=CARTESIAN_POINT('Ctrl Pts',(95.2904686796155,-0.135665274855846,
-6.66625606955345));
#28657=CARTESIAN_POINT('Ctrl Pts',(95.2923490111909,-0.15100170166125,-6.66519465902959));
#28658=CARTESIAN_POINT('Ctrl Pts',(95.3058518756613,-0.245674233697498,
-6.6585676260039));
#28659=CARTESIAN_POINT('Ctrl Pts',(95.3252477515618,-0.323674828359904,
-6.6527594652683));
#28660=CARTESIAN_POINT('Ctrl Pts',(95.367985807511,-0.442337745785066,-6.64350834176286));
#28661=CARTESIAN_POINT('Ctrl Pts',(95.3860823872989,-0.484640395431857,
-6.64012579657745));
#28662=CARTESIAN_POINT('Ctrl Pts',(95.4159892121333,-0.544585949723476,
-6.6352847014064));
#28663=CARTESIAN_POINT('Ctrl Pts',(95.4258748662814,-0.563140483989728,
-6.63377955208505));
#28664=CARTESIAN_POINT('Ctrl Pts',(95.4428132697675,-0.592979070246764,
-6.63135867429022));
#28665=CARTESIAN_POINT('Ctrl Pts',(95.4495696285024,-0.604425365480685,
-6.63042993498791));
#28666=CARTESIAN_POINT('Ctrl Pts',(95.4589941440449,-0.619791626180912,
-6.62918547982462));
#28667=CARTESIAN_POINT('Ctrl Pts',(95.4614940188893,-0.623812949350992,
-6.62886003069042));
#28668=CARTESIAN_POINT('Ctrl Pts',(95.4657127585979,-0.630508853916345,
-6.62831863929037));
#28669=CARTESIAN_POINT('Ctrl Pts',(95.4674183007945,-0.633191712671926,
-6.62810185836539));
#28670=CARTESIAN_POINT('Ctrl Pts',(95.470674236865,-0.638267863012345,-6.62769200723682));
#28671=CARTESIAN_POINT('Ctrl Pts',(95.4722224888696,-0.640662476476597,
-6.62749879619482));
#28672=CARTESIAN_POINT('Ctrl Pts',(95.4759174468369,-0.646332039068705,
-6.62704159637374));
#28673=CARTESIAN_POINT('Ctrl Pts',(95.4780718354806,-0.649601977583934,
-6.62677810620311));
#28674=CARTESIAN_POINT('Ctrl Pts',(95.4857192190023,-0.661084141783455,
-6.62585336052541));
#28675=CARTESIAN_POINT('Ctrl Pts',(95.4912993819246,-0.66923820760908,-6.62519752516876));
#28676=CARTESIAN_POINT('Ctrl Pts',(95.5363320299228,-0.733297782744541,
-6.62004388162376));
#28677=CARTESIAN_POINT('Ctrl Pts',(95.5804912541242,-0.78574650224787,-6.6158117083185));
#28678=CARTESIAN_POINT('Ctrl Pts',(95.6902664365645,-0.89518621107208,-6.60622216171109));
#28679=CARTESIAN_POINT('Ctrl Pts',(95.7581141935825,-0.949350995624699,
-6.60087817898132));
#28680=CARTESIAN_POINT('Ctrl Pts',(95.8424503091521,-1.00265039292678,-6.59435115039625));
#28681=CARTESIAN_POINT('Ctrl Pts',(95.853738516747,-1.00952131245255,-6.59348029524783));
#28682=CARTESIAN_POINT('Ctrl Pts',(95.8709380874977,-1.01959768482887,-6.59215626220949));
#28683=CARTESIAN_POINT('Ctrl Pts',(95.8767654580151,-1.02294498723317,-6.59170815778875));
#28684=CARTESIAN_POINT('Ctrl Pts',(95.8873511140098,-1.02890559397645,-6.59089487352994));
#28685=CARTESIAN_POINT('Ctrl Pts',(95.8920994600095,-1.03153623802809,-6.59053032067421));
#28686=CARTESIAN_POINT('Ctrl Pts',(95.9023337699283,-1.03711405772246,-6.58974504468454));
#28687=CARTESIAN_POINT('Ctrl Pts',(95.9078252422478,-1.04005072446527,-6.58932396618008));
#28688=CARTESIAN_POINT('Ctrl Pts',(95.9227020458748,-1.04785528182953,-6.58818384102774));
#28689=CARTESIAN_POINT('Ctrl Pts',(95.9321298731212,-1.05264047437733,-6.58746195533605));
#28690=CARTESIAN_POINT('Ctrl Pts',(95.9810959588417,-1.07667018221481,-6.58371488916381));
#28691=CARTESIAN_POINT('Ctrl Pts',(96.0216203840396,-1.09381406515535,-6.5806193826683));
#28692=CARTESIAN_POINT('Ctrl Pts',(96.1386261593378,-1.13576332831866,-6.57169916182054));
#28693=CARTESIAN_POINT('Ctrl Pts',(96.2168211188963,-1.15506573166786,-6.56574380785287));
#28694=CARTESIAN_POINT('Ctrl Pts',(96.3233663105552,-1.17005912738607,-6.55791348947447));
#28695=CARTESIAN_POINT('Ctrl Pts',(96.350497227059,-1.17292052713774,-6.55594570669523));
#28696=CARTESIAN_POINT('Ctrl Pts',(96.3884220147451,-1.17559261825991,-6.55325065614377));
#28697=CARTESIAN_POINT('Ctrl Pts',(96.3991496217172,-1.17620108002537,-6.55249451763901));
#28698=CARTESIAN_POINT('Ctrl Pts',(96.4179139396726,-1.17700794553109,-6.55118437050939));
#28699=CARTESIAN_POINT('Ctrl Pts',(96.4259470167422,-1.17727102679033,-6.55062747829001));
#28700=CARTESIAN_POINT('Ctrl Pts',(96.4378608406751,-1.17753914706734,-6.54980806483703));
#28701=CARTESIAN_POINT('Ctrl Pts',(96.4417397309224,-1.17760726900286,-6.54954230400516));
#28702=CARTESIAN_POINT('Ctrl Pts',(96.4483729542905,-1.17769098012333,-6.54908965952942));
#28703=CARTESIAN_POINT('Ctrl Pts',(96.4511270821563,-1.17771607527399,-6.5489022626791));
#28704=CARTESIAN_POINT('Ctrl Pts',(96.4573810237441,-1.17775112013457,-6.54847797465331));
#28705=CARTESIAN_POINT('Ctrl Pts',(96.460880812931,-1.17775513220227,-6.54824141232947));
#28706=CARTESIAN_POINT('Ctrl Pts',(96.4704194527739,-1.17772354841607,-6.54759892203324));
#28707=CARTESIAN_POINT('Ctrl Pts',(96.4764581961902,-1.17765710704174,-6.54719463930771));
#28708=CARTESIAN_POINT('Ctrl Pts',(96.5070392354961,-1.1770853638528,-6.54515857853924));
#28709=CARTESIAN_POINT('Ctrl Pts',(96.5315638859691,-1.17585927913545,-6.54356252610402));
#28710=CARTESIAN_POINT('Ctrl Pts',(96.6413452961866,-1.16692302732949,-6.53651201617018));
#28711=CARTESIAN_POINT('Ctrl Pts',(96.7256509405527,-1.15069914691953,-6.53133637836794));
#28712=CARTESIAN_POINT('Ctrl Pts',(96.8423662896013,-1.11471656023951,-6.52370707882488));
#28713=CARTESIAN_POINT('Ctrl Pts',(96.8767519601512,-1.10233731423134,-6.52140104235198));
#28714=CARTESIAN_POINT('Ctrl Pts',(96.9250767686707,-1.08235596042181,-6.51803320752284));
#28715=CARTESIAN_POINT('Ctrl Pts',(96.9395254836066,-1.07603903230836,-6.51700954238216));
#28716=CARTESIAN_POINT('Ctrl Pts',(96.9651675148167,-1.06420960559142,-6.51515952468187));
#28717=CARTESIAN_POINT('Ctrl Pts',(96.976408429865,-1.05880566184313,-6.51433677402654));
#28718=CARTESIAN_POINT('Ctrl Pts',(96.9934359994418,-1.05028431207131,-6.51307135825483));
#28719=CARTESIAN_POINT('Ctrl Pts',(96.9992861253679,-1.04729518329883,-6.51263310103723));
#28720=CARTESIAN_POINT('Ctrl Pts',(97.0094495739748,-1.04199446114889,-6.51186543272601));
#28721=CARTESIAN_POINT('Ctrl Pts',(97.0137741067745,-1.03970461603379,-6.51153678483164));
#28722=CARTESIAN_POINT('Ctrl Pts',(97.023504136168,-1.03447465738387,-6.5107927271788));
#28723=CARTESIAN_POINT('Ctrl Pts',(97.0289010784578,-1.03151901582678,-6.51037677949352));
#28724=CARTESIAN_POINT('Ctrl Pts',(97.0434524863879,-1.02340104621739,-6.50924632855243));
#28725=CARTESIAN_POINT('Ctrl Pts',(97.0525612338912,-1.01815835636783,-6.50852900134568));
#28726=CARTESIAN_POINT('Ctrl Pts',(97.0970351749597,-0.991762027325579,
-6.50497754541005));
#28727=CARTESIAN_POINT('Ctrl Pts',(97.1313396093513,-0.968886555653917,
-6.50208217499418));
#28728=CARTESIAN_POINT('Ctrl Pts',(97.2246286154107,-0.899345267029481,
-6.49375301315903));
#28729=CARTESIAN_POINT('Ctrl Pts',(97.2804437874361,-0.848765357205703,
-6.48820138308741));
#28730=CARTESIAN_POINT('Ctrl Pts',(97.3607237898152,-0.760656683276405,
-6.47948943620218));
#28731=CARTESIAN_POINT('Ctrl Pts',(97.3885467461173,-0.726450577163617,
-6.47630042458242));
#28732=CARTESIAN_POINT('Ctrl Pts',(97.419981390835,-0.683040888322591,-6.47254807776065));
#28733=CARTESIAN_POINT('Ctrl Pts',(97.4254792035999,-0.675251313284863,
-6.47188567271996));
#28734=CARTESIAN_POINT('Ctrl Pts',(97.4332369364403,-0.663971476982828,
-6.47094299065326));
#28735=CARTESIAN_POINT('Ctrl Pts',(97.4355737448172,-0.660534915212928,
-6.47065795757379));
#28736=CARTESIAN_POINT('Ctrl Pts',(97.4396076412911,-0.654534518784581,
-6.47016413491832));
#28737=CARTESIAN_POINT('Ctrl Pts',(97.4413129510756,-0.651976303583453,
-6.4699548102471));
#28738=CARTESIAN_POINT('Ctrl Pts',(97.4449073698435,-0.646538125384458,
-6.46951242701816));
#28739=CARTESIAN_POINT('Ctrl Pts',(97.4467938782767,-0.643656532585285,
-6.46927953689866));
#28740=CARTESIAN_POINT('Ctrl Pts',(97.4519022161957,-0.635778482086857,
-6.46864684674658));
#28741=CARTESIAN_POINT('Ctrl Pts',(97.4550989518948,-0.630765756304915,
-6.4682486458724));
#28742=CARTESIAN_POINT('Ctrl Pts',(97.4702440119052,-0.606615700005522,
-6.4663499910362));
#28743=CARTESIAN_POINT('Ctrl Pts',(97.4816796316555,-0.587160506480568,
-6.46487953164393));
#28744=CARTESIAN_POINT('Ctrl Pts',(97.5030883246456,-0.548218410019451,
-6.46202629314796));
#28745=CARTESIAN_POINT('Ctrl Pts',(97.5130909903189,-0.528758694738336,
-6.46064277683167));
#28746=CARTESIAN_POINT('Ctrl Pts',(97.5498478125473,-0.452067564998741,
-6.45531021791453));
#28747=CARTESIAN_POINT('Ctrl Pts',(97.5725228175004,-0.392999393906959,
-6.45145147319395));
#28748=CARTESIAN_POINT('Ctrl Pts',(97.6035632474028,-0.287487839187075,
-6.44459230214978));
#28749=CARTESIAN_POINT('Ctrl Pts',(97.6140845393863,-0.241835666300203,
-6.44163585950262));
#28750=CARTESIAN_POINT('Ctrl Pts',(97.6248372168816,-0.17801799557965,-6.43743474833347));
#28751=CARTESIAN_POINT('Ctrl Pts',(97.6274098763244,-0.160289577392258,
-6.43626082756384));
#28752=CARTESIAN_POINT('Ctrl Pts',(97.6304940943667,-0.134987882264762,
-6.43457247195045));
#28753=CARTESIAN_POINT('Ctrl Pts',(97.6313383982642,-0.127457121100252,
-6.4340683350963));
#28754=CARTESIAN_POINT('Ctrl Pts',(97.632674183451,-0.114406259897808,-6.43319162958434));
#28755=CARTESIAN_POINT('Ctrl Pts',(97.6331994912195,-0.108889807352842,
-6.43282012054389));
#28756=CARTESIAN_POINT('Ctrl Pts',(97.6341349203291,-0.0982730836760085,
-6.4321032435833));
#28757=CARTESIAN_POINT('Ctrl Pts',(97.6345507737163,-0.0931734332342861,
-6.43175806215189));
#28758=CARTESIAN_POINT('Ctrl Pts',(97.6355563586899,-0.0797637110079606,
-6.43084811551969));
#28759=CARTESIAN_POINT('Ctrl Pts',(97.6360911603116,-0.0714499330442044,
-6.43028166602089));
#28760=CARTESIAN_POINT('Ctrl Pts',(97.6376772222503,-0.0419036223203609,
-6.42826000418489));
#28761=CARTESIAN_POINT('Ctrl Pts',(97.6382417257713,-0.0206501988785537,
-6.42678999378801));
#28762=CARTESIAN_POINT('Ctrl Pts',(97.6382140000112,0.0332598275708147,
-6.42301894700937));
#28763=CARTESIAN_POINT('Ctrl Pts',(97.6368391832829,0.065896413955691,-6.42069626626272));
#28764=CARTESIAN_POINT('Ctrl Pts',(97.6298868297191,0.148791611277646,-6.41470261470262));
#28765=CARTESIAN_POINT('Ctrl Pts',(97.6224263379453,0.198825026263183,-6.41099429383886));
#28766=CARTESIAN_POINT('Ctrl Pts',(97.6110837334361,0.251434082744044,-6.4070450548286));
#28767=CARTESIAN_POINT('Ctrl Pts',(97.6103776089468,0.254643941617654,-6.4068039108287));
#28768=CARTESIAN_POINT('Ctrl Pts',(97.6049769058671,0.27871353615749,-6.40499438376585));
#28769=CARTESIAN_POINT('Ctrl Pts',(97.599728395594,0.299445359541044,-6.40342850915444));
#28770=CARTESIAN_POINT('Ctrl Pts',(97.5831333425461,0.358220641598347,-6.39898418391393));
#28771=CARTESIAN_POINT('Ctrl Pts',(97.57042310532,0.395852911075683,-6.39613195607784));
#28772=CARTESIAN_POINT('Ctrl Pts',(97.5535409305178,0.43858171554812,-6.39293680336859));
#28773=CARTESIAN_POINT('Ctrl Pts',(97.5512005187677,0.444370193353944,-6.39250491846749));
#28774=CARTESIAN_POINT('Ctrl Pts',(97.5473311181675,0.453725499701246,-6.39180878419786));
#28775=CARTESIAN_POINT('Ctrl Pts',(97.5458303760868,0.457303773767396,-6.3915429708514));
#28776=CARTESIAN_POINT('Ctrl Pts',(97.5431203141618,0.463676980146255,-6.39107041973514));
#28777=CARTESIAN_POINT('Ctrl Pts',(97.541917813519,0.466474699923981,-6.39086328978902));
#28778=CARTESIAN_POINT('Ctrl Pts',(97.5392628863272,0.472586166601736,-6.39041151453834));
#28779=CARTESIAN_POINT('Ctrl Pts',(97.5378060353482,0.475897901204183,-6.39016713702707));
#28780=CARTESIAN_POINT('Ctrl Pts',(97.5335875357173,0.485368806173461,-6.3894693658288));
#28781=CARTESIAN_POINT('Ctrl Pts',(97.5307881136972,0.491511142242594,-6.38901816654835));
#28782=CARTESIAN_POINT('Ctrl Pts',(97.5096267554015,0.536903968263261,-6.38569123003344));
#28783=CARTESIAN_POINT('Ctrl Pts',(97.4891616271496,0.575143260742656,-6.38292990678871));
#28784=CARTESIAN_POINT('Ctrl Pts',(97.4147699519221,0.697411795327552,-6.37395800888754));
#28785=CARTESIAN_POINT('Ctrl Pts',(97.3522885149229,0.775712726408799,-6.36794002487711));
#28786=CARTESIAN_POINT('Ctrl Pts',(97.2627906157386,0.862563547676247,-6.35992858924687));
#28787=CARTESIAN_POINT('Ctrl Pts',(97.2443526058202,0.879353034369116,-6.35830710163057));
#28788=CARTESIAN_POINT('Ctrl Pts',(97.218653605128,0.901303461059263,-6.35607605470773));
#28789=CARTESIAN_POINT('Ctrl Pts',(97.2118458023342,0.906986524420999,-6.35548769273213));
#28790=CARTESIAN_POINT('Ctrl Pts',(97.2009317177421,0.91589024760749,-6.35454825769523));
#28791=CARTESIAN_POINT('Ctrl Pts',(97.1968669970133,0.919161505610537,-6.35419920861212));
#28792=CARTESIAN_POINT('Ctrl Pts',(97.1884865346369,0.925814772599333,-6.35348115195328));
#28793=CARTESIAN_POINT('Ctrl Pts',(97.1841686497784,0.929193863450808,-6.35311204154711));
#28794=CARTESIAN_POINT('Ctrl Pts',(97.1741182418024,0.936946565517706,-6.35225476622127));
#28795=CARTESIAN_POINT('Ctrl Pts',(97.1683688851874,0.941297890205902,-6.35176575228866));
#28796=CARTESIAN_POINT('Ctrl Pts',(97.1499045966491,0.955007507601559,-6.35019942463083));
#28797=CARTESIAN_POINT('Ctrl Pts',(97.1370417562897,0.964162713264354,-6.34911445219719));
#28798=CARTESIAN_POINT('Ctrl Pts',(97.1063590465374,0.985084978912101,-6.34653948599908));
#28799=CARTESIAN_POINT('Ctrl Pts',(97.0883959686486,0.996631106529467,-6.34504197695392));
#28800=CARTESIAN_POINT('Ctrl Pts',(97.0192090762279,1.0384892691016,-6.33931090346108));
#28801=CARTESIAN_POINT('Ctrl Pts',(96.9660316459853,1.06538919758095,-6.33497436830918));
#28802=CARTESIAN_POINT('Ctrl Pts',(96.8462006986222,1.11500791331544,-6.32545956510982));
#28803=CARTESIAN_POINT('Ctrl Pts',(96.7790691923926,1.13601306406664,-6.3202870873618));
#28804=CARTESIAN_POINT('Ctrl Pts',(96.7008772836855,1.15299646752377,-6.31467876964369));
#28805=CARTESIAN_POINT('Ctrl Pts',(96.6912671254805,1.15495844436013,-6.31399663193341));
#28806=CARTESIAN_POINT('Ctrl Pts',(96.6777994931307,1.15753313023076,-6.31305168286904));
#28807=CARTESIAN_POINT('Ctrl Pts',(96.6739620997812,1.15824699289352,-6.31278367702705));
#28808=CARTESIAN_POINT('Ctrl Pts',(96.6673183216287,1.15944878152602,-6.31232190095664));
#28809=CARTESIAN_POINT('Ctrl Pts',(96.6645136143982,1.15994562268493,-6.31212764536109));
#28810=CARTESIAN_POINT('Ctrl Pts',(96.6585710386177,1.16097610212309,-6.31171754942728));
#28811=CARTESIAN_POINT('Ctrl Pts',(96.6554327538588,1.16150720513299,-6.31150185716318));
#28812=CARTESIAN_POINT('Ctrl Pts',(96.6476025712696,1.16279970509167,-6.31096580013974));
#28813=CARTESIAN_POINT('Ctrl Pts',(96.6429080831402,1.1635454431752,-6.31064629631608));
#28814=CARTESIAN_POINT('Ctrl Pts',(96.6249372747957,1.16628874031958,-6.30942996184777));
#28815=CARTESIAN_POINT('Ctrl Pts',(96.6116310703794,1.16808774814728,-6.30854340475372));
#28816=CARTESIAN_POINT('Ctrl Pts',(96.5771242340034,1.17215352552066,-6.30627382807899));
#28817=CARTESIAN_POINT('Ctrl Pts',(96.5558869972553,1.17407297024528,-6.30490569074452));
#28818=CARTESIAN_POINT('Ctrl Pts',(96.4372531592432,1.1815545770533,-6.29736534195314));
#28819=CARTESIAN_POINT('Ctrl Pts',(96.3395107043682,1.1755760214272,-6.29150426647801));
#28820=CARTESIAN_POINT('Ctrl Pts',(96.20736108397,1.1508198138611,-6.2829849723384));
#28821=CARTESIAN_POINT('Ctrl Pts',(96.171444548039,1.14232808364211,-6.28061083410622));
#28822=CARTESIAN_POINT('Ctrl Pts',(96.126190896751,1.12935782354046,-6.27751264577182));
#28823=CARTESIAN_POINT('Ctrl Pts',(96.1164307953046,1.12642283964321,-6.27683803425672));
#28824=CARTESIAN_POINT('Ctrl Pts',(96.1009071067815,1.12153409691083,-6.27575419847077));
#28825=CARTESIAN_POINT('Ctrl Pts',(96.0951182978829,1.1196616494983,-6.27534760455511));
#28826=CARTESIAN_POINT('Ctrl Pts',(96.0841733583678,1.11602748462523,-6.27457411431935));
#28827=CARTESIAN_POINT('Ctrl Pts',(96.0790144225876,1.11427466843559,-6.27420751617533));
#28828=CARTESIAN_POINT('Ctrl Pts',(96.0673113239119,1.11020758805205,-6.27337120888573));
#28829=CARTESIAN_POINT('Ctrl Pts',(96.0607751354811,1.10787115754674,-6.27290078496142));
#28830=CARTESIAN_POINT('Ctrl Pts',(96.0407986197154,1.10053054689853,-6.27145252376573));
#28831=CARTESIAN_POINT('Ctrl Pts',(96.0274291553537,1.09533869406666,-6.27046856689777));
#28832=CARTESIAN_POINT('Ctrl Pts',(95.9827623785651,1.07704736799627,-6.26713000623253));
#28833=CARTESIAN_POINT('Ctrl Pts',(95.9519486350283,1.06284486748073,-6.2647404968259));
#28834=CARTESIAN_POINT('Ctrl Pts',(95.9218016184021,1.04733931496196,-6.26231549050881));
#28835=CARTESIAN_POINT('',(97.6382310967021,0.000547024120039822,-6.32657975732822));
#28836=CARTESIAN_POINT('Ctrl Pts',(95.9218016730721,1.04733934308042,-6.16392795844921));
#28837=CARTESIAN_POINT('Ctrl Pts',(95.922563112493,1.04773097511363,-6.16398566787288));
#28838=CARTESIAN_POINT('Ctrl Pts',(95.9233249825432,1.04812177859259,-6.16404332757542));
#28839=CARTESIAN_POINT('Ctrl Pts',(95.9302824848695,1.05168107125754,-6.16456913886483));
#28840=CARTESIAN_POINT('Ctrl Pts',(95.936505840373,1.05479551493692,-6.16503407858795));
#28841=CARTESIAN_POINT('Ctrl Pts',(95.9896527061383,1.0808061053226,-6.16896211148023));
#28842=CARTESIAN_POINT('Ctrl Pts',(96.0380297290864,1.10061687438719,-6.17225861912953));
#28843=CARTESIAN_POINT('Ctrl Pts',(96.1665038556081,1.14350238451902,-6.18069540740678));
#28844=CARTESIAN_POINT('Ctrl Pts',(96.2480061203872,1.16141047430317,-6.18575941567));
#28845=CARTESIAN_POINT('Ctrl Pts',(96.3613081711256,1.17397073361564,-6.19303060148706));
#28846=CARTESIAN_POINT('Ctrl Pts',(96.3920204829251,1.17616131225994,-6.19502196731284));
#28847=CARTESIAN_POINT('Ctrl Pts',(96.4323459294853,1.17745278330718,-6.19768092560179));
#28848=CARTESIAN_POINT('Ctrl Pts',(96.4419135820801,1.17764250953152,-6.19831501275069));
#28849=CARTESIAN_POINT('Ctrl Pts',(96.4574301591676,1.1777610686296,-6.19934905617941));
#28850=CARTESIAN_POINT('Ctrl Pts',(96.4633782256095,1.17776145534552,-6.19974679874765));
#28851=CARTESIAN_POINT('Ctrl Pts',(96.4748079237645,1.1776756149533,-6.20051381549532));
#28852=CARTESIAN_POINT('Ctrl Pts',(96.4802894633657,1.17759616901684,-6.20088287026639));
#28853=CARTESIAN_POINT('Ctrl Pts',(96.4929759829276,1.17732369508064,-6.20173989376937));
#28854=CARTESIAN_POINT('Ctrl Pts',(96.5001800810567,1.17710279294289,-6.20222871024624));
#28855=CARTESIAN_POINT('Ctrl Pts',(96.5231426733327,1.17618764577807,-6.20379389131561));
#28856=CARTESIAN_POINT('Ctrl Pts',(96.5388888760486,1.17524296423839,-6.20487789939013));
#28857=CARTESIAN_POINT('Ctrl Pts',(96.5758697331021,1.17227784345375,-6.20745019712985));
#28858=CARTESIAN_POINT('Ctrl Pts',(96.5970772987344,1.16999626204206,-6.20894598144011));
#28859=CARTESIAN_POINT('Ctrl Pts',(96.6770743644979,1.15918533208471,-6.2146669342726));
#28860=CARTESIAN_POINT('Ctrl Pts',(96.7352462647189,1.14678940374526,-6.21899467502292));
#28861=CARTESIAN_POINT('Ctrl Pts',(96.8597490688461,1.11023957005936,-6.22851362957974));
#28862=CARTESIAN_POINT('Ctrl Pts',(96.9253628933871,1.08440467346871,-6.2336994955841));
#28863=CARTESIAN_POINT('Ctrl Pts',(96.9970705172817,1.04845760473146,-6.2393215817859));
#28864=CARTESIAN_POINT('Ctrl Pts',(97.0058040001702,1.04394180839303,-6.2400053243453));
#28865=CARTESIAN_POINT('Ctrl Pts',(97.0179121310306,1.0374876696322,-6.24095085073008));
#28866=CARTESIAN_POINT('Ctrl Pts',(97.0213349822347,1.03564131909707,-6.2412178688659));
#28867=CARTESIAN_POINT('Ctrl Pts',(97.0272455871402,1.03241512972441,-6.24167840302406));
#28868=CARTESIAN_POINT('Ctrl Pts',(97.0297375770687,1.03104318385395,-6.24187239849109));
#28869=CARTESIAN_POINT('Ctrl Pts',(97.0349546822618,1.02814626602596,-6.24227813774319));
#28870=CARTESIAN_POINT('Ctrl Pts',(97.0376787525753,1.02661945753236,-6.24248975956405));
#28871=CARTESIAN_POINT('Ctrl Pts',(97.0444083271762,1.0228123597931,-6.24301205897135));
#28872=CARTESIAN_POINT('Ctrl Pts',(97.048406628863,1.02051933007265,-6.2433219422143));
#28873=CARTESIAN_POINT('Ctrl Pts',(97.0570501933388,1.01549457826232,-6.24399113406132));
#28874=CARTESIAN_POINT('Ctrl Pts',(97.0616904004122,1.01275431369899,-6.24434992967829));
#28875=CARTESIAN_POINT('Ctrl Pts',(97.0748985415809,1.00483150247323,-6.24537041023857));
#28876=CARTESIAN_POINT('Ctrl Pts',(97.0834196253427,0.999571281453929,-6.24602777383116));
#28877=CARTESIAN_POINT('Ctrl Pts',(97.1125840214401,0.981049744280293,-6.24827797940317));
#28878=CARTESIAN_POINT('Ctrl Pts',(97.1328804702724,0.967251807148861,-6.24984455389308));
#28879=CARTESIAN_POINT('Ctrl Pts',(97.1957699914671,0.921561180436383,-6.25474975691232));
#28880=CARTESIAN_POINT('Ctrl Pts',(97.2366415940102,0.887412044365937,-6.25801736410874));
#28881=CARTESIAN_POINT('Ctrl Pts',(97.3283567274873,0.799581789929832,-6.26588334692849));
#28882=CARTESIAN_POINT('Ctrl Pts',(97.3767265850738,0.743660682474676,-6.27049781399808));
#28883=CARTESIAN_POINT('Ctrl Pts',(97.4255624071594,0.675144674849057,-6.2760201572786));
#28884=CARTESIAN_POINT('Ctrl Pts',(97.4314681037548,0.666623197197055,-6.27670458428418));
#28885=CARTESIAN_POINT('Ctrl Pts',(97.4410142309935,0.652452824303797,-6.27783945770471));
#28886=CARTESIAN_POINT('Ctrl Pts',(97.4447202628394,0.646848649218851,-6.27828745843873));
#28887=CARTESIAN_POINT('Ctrl Pts',(97.4513331977036,0.636660306721674,-6.2791006024171));
#28888=CARTESIAN_POINT('Ctrl Pts',(97.4542567652243,0.632087138235138,-6.27946511928141));
#28889=CARTESIAN_POINT('Ctrl Pts',(97.4604665555374,0.622223941011471,-6.28025037085191));
#28890=CARTESIAN_POINT('Ctrl Pts',(97.4637426277905,0.616927748892035,-6.28067146124422));
#28891=CARTESIAN_POINT('Ctrl Pts',(97.4726130712866,0.602330012569163,-6.28183071466693));
#28892=CARTESIAN_POINT('Ctrl Pts',(97.4781209830983,0.592976917207233,-6.28257195220699));
#28893=CARTESIAN_POINT('Ctrl Pts',(97.5101647293477,0.536801165153988,-6.28701620606528));
#28894=CARTESIAN_POINT('Ctrl Pts',(97.5335912196377,0.488287176819846,-6.29082716945488));
#28895=CARTESIAN_POINT('Ctrl Pts',(97.5851507511299,0.359709912925321,-6.30084307963857));
#28896=CARTESIAN_POINT('Ctrl Pts',(97.6081053575673,0.277904047255513,-6.30715021368868));
#28897=CARTESIAN_POINT('Ctrl Pts',(97.6260839112692,0.170446412269312,-6.31498837514428));
#28898=CARTESIAN_POINT('Ctrl Pts',(97.6293442998321,0.14642710755381,-6.31671076688734));
#28899=CARTESIAN_POINT('Ctrl Pts',(97.6326395923647,0.114870847708047,-6.31892135839255));
#28900=CARTESIAN_POINT('Ctrl Pts',(97.6333466432607,0.107411672180922,-6.319440080944));
#28901=CARTESIAN_POINT('Ctrl Pts',(97.6343067300385,0.0961389542123721,
-6.3202177571464));
#28902=CARTESIAN_POINT('Ctrl Pts',(97.6346124519052,0.0923302641037898,
-6.32047943412826));
#28903=CARTESIAN_POINT('Ctrl Pts',(97.6351141126204,0.0856746027480229,
-6.32093475840938));
#28904=CARTESIAN_POINT('Ctrl Pts',(97.6353182449771,0.082828347728783,-6.32112884702605));
#28905=CARTESIAN_POINT('Ctrl Pts',(97.6357079288444,0.0771033748498703,
-6.32151796995362));
#28906=CARTESIAN_POINT('Ctrl Pts',(97.6358932493507,0.074224720957689,-6.32171299255664));
#28907=CARTESIAN_POINT('Ctrl Pts',(97.6362833068183,0.0677975840028478,
-6.32214705208869));
#28908=CARTESIAN_POINT('Ctrl Pts',(97.6364825613619,0.0642487787548318,
-6.32238579392906));
#28909=CARTESIAN_POINT('Ctrl Pts',(97.6370764387331,0.0527410317584296,
-6.32315711372388));
#28910=CARTESIAN_POINT('Ctrl Pts',(97.6374063641442,0.0447787711189562,
-6.32368637478584));
#28911=CARTESIAN_POINT('Ctrl Pts',(97.6380333978018,0.0247283095537273,
-6.32500941512401));
#28912=CARTESIAN_POINT('Ctrl Pts',(97.6382252217385,0.0126375602041876,
-6.32579832911198));
#28913=CARTESIAN_POINT('Ctrl Pts',(97.6382308232104,0.000545579152858998,
-6.32658032579348));
#28914=CARTESIAN_POINT('Ctrl Pts',(97.638230822526,0.000547054579173728,
-6.32658023037662));
#28915=CARTESIAN_POINT('Ctrl Pts',(97.6382841975052,-0.114363554607446,
-6.33401158344397));
#28916=CARTESIAN_POINT('Ctrl Pts',(97.6215212050235,-0.228681168633696,
-6.3408298649339));
#28917=CARTESIAN_POINT('Ctrl Pts',(97.5782532072311,-0.37274396974925,-6.35038124470256));
#28918=CARTESIAN_POINT('Ctrl Pts',(97.5665233819034,-0.406229794622361,
-6.35266825828143));
#28919=CARTESIAN_POINT('Ctrl Pts',(97.5496903086269,-0.448120347660356,
-6.3556427710319));
#28920=CARTESIAN_POINT('Ctrl Pts',(97.5459683144041,-0.457062408679015,
-6.35628442907455));
#28921=CARTESIAN_POINT('Ctrl Pts',(97.5397732695014,-0.471443349841197,
-6.35732776507842));
#28922=CARTESIAN_POINT('Ctrl Pts',(97.5373683294266,-0.476911221145789,
-6.35772715364962));
#28923=CARTESIAN_POINT('Ctrl Pts',(97.532679841269,-0.48735466350336,-6.35849527059932));
#28924=CARTESIAN_POINT('Ctrl Pts',(97.5304029865321,-0.492333082868035,
-6.35886376436613));
#28925=CARTESIAN_POINT('Ctrl Pts',(97.525122173311,-0.503670111888112,-6.35970834484416));
#28926=CARTESIAN_POINT('Ctrl Pts',(97.522095828661,-0.510018001328114,-6.36018518509997));
#28927=CARTESIAN_POINT('Ctrl Pts',(97.5123344175467,-0.530029620593106,
-6.36170116777126));
#28928=CARTESIAN_POINT('Ctrl Pts',(97.5053912467714,-0.543589504999928,
-6.3627474028073));
#28929=CARTESIAN_POINT('Ctrl Pts',(97.4576207080709,-0.632585677250096,
-6.36974446189395));
#28930=CARTESIAN_POINT('Ctrl Pts',(97.4089266922658,-0.70348973500071,-6.37597722598481));
#28931=CARTESIAN_POINT('Ctrl Pts',(97.3205649228632,-0.806113269699055,
-6.3859155728305));
#28932=CARTESIAN_POINT('Ctrl Pts',(97.2857989419411,-0.841673204556276,
-6.38956512077702));
#28933=CARTESIAN_POINT('Ctrl Pts',(97.2373154659919,-0.885362029434795,
-6.39424050199586));
#28934=CARTESIAN_POINT('Ctrl Pts',(97.2255351438537,-0.895561230911203,
-6.39534708119846));
#28935=CARTESIAN_POINT('Ctrl Pts',(97.2079160242565,-0.910214078499494,
-6.39695551443686));
#28936=CARTESIAN_POINT('Ctrl Pts',(97.2022328558241,-0.914851340635053,
-6.39746741681967));
#28937=CARTESIAN_POINT('Ctrl Pts',(97.1931083269955,-0.922155700945378,
-6.39827788426448));
#28938=CARTESIAN_POINT('Ctrl Pts',(97.1896949613425,-0.924857252453686,
-6.39857856643817));
#28939=CARTESIAN_POINT('Ctrl Pts',(97.1832183978412,-0.929925063789778,
-6.39914425416295));
#28940=CARTESIAN_POINT('Ctrl Pts',(97.1801583700353,-0.932295261675217,
-6.39940951602619));
#28941=CARTESIAN_POINT('Ctrl Pts',(97.1770741684891,-0.934659949584272,
-6.3996748138989));
#28942=CARTESIAN_POINT('Ctrl Pts',(97.1770616775413,-0.93466952612027,-6.39967588831562));
#28943=CARTESIAN_POINT('Ctrl Pts',(97.1770365006298,-0.934688827905284,
-6.39967805385534));
#28944=CARTESIAN_POINT('Ctrl Pts',(97.1770238151556,-0.93469855276653,-6.39967914493518));
#28945=CARTESIAN_POINT('Ctrl Pts',(97.1769982440161,-0.934718155131924,
-6.3996813442431));
#28946=CARTESIAN_POINT('Ctrl Pts',(97.1769853579655,-0.934728032918421,
-6.39968245250321));
#28947=CARTESIAN_POINT('Ctrl Pts',(97.1769593795787,-0.934747945766344,
-6.39968468669242));
#28948=CARTESIAN_POINT('Ctrl Pts',(97.1769462879421,-0.934757980278049,
-6.39968581256022));
#28949=CARTESIAN_POINT('Ctrl Pts',(97.1769198932066,-0.93477821050335,-6.39968808240652));
#28950=CARTESIAN_POINT('Ctrl Pts',(97.1769065892131,-0.934788406888409,
-6.39968922646074));
#28951=CARTESIAN_POINT('Ctrl Pts',(97.1768797629196,-0.934808966062894,
-6.3996915332648));
#28952=CARTESIAN_POINT('Ctrl Pts',(97.1768662416346,-0.934819328059535,
-6.39969269592608));
#28953=CARTESIAN_POINT('Ctrl Pts',(97.1768389749724,-0.934840222846379,
-6.39969504043793));
#28954=CARTESIAN_POINT('Ctrl Pts',(97.1768252288227,-0.93485075621291,-6.39969622235359));
#28955=CARTESIAN_POINT('Ctrl Pts',(97.1767975058387,-0.934871998743925,
-6.39969860593701));
#28956=CARTESIAN_POINT('Ctrl Pts',(97.176783529133,-0.934882707793599,-6.39969980759232));
#28957=CARTESIAN_POINT('Ctrl Pts',(97.1767553380894,-0.934904306965047,
-6.39970223124818));
#28958=CARTESIAN_POINT('Ctrl Pts',(97.1767411235764,-0.934915197204015,
-6.39970345326234));
#28959=CARTESIAN_POINT('Ctrl Pts',(97.1767124495286,-0.934937164363926,
-6.39970591826676));
#28960=CARTESIAN_POINT('Ctrl Pts',(97.1766979903701,-0.934948240978808,
-6.39970716122316));
#28961=CARTESIAN_POINT('Ctrl Pts',(97.1766688198372,-0.934970586347813,
-6.39970966872592));
#28962=CARTESIAN_POINT('Ctrl Pts',(97.1766541082385,-0.934981855255116,
-6.39971093328997));
#28963=CARTESIAN_POINT('Ctrl Pts',(97.1766244253358,-0.935004590889115,
-6.39971348464696));
#28964=CARTESIAN_POINT('Ctrl Pts',(97.1766094537715,-0.935016057795706,
-6.39971477146062));
#28965=CARTESIAN_POINT('Ctrl Pts',(97.1765792424907,-0.935039195838656,
-6.39971736803779));
#28966=CARTESIAN_POINT('Ctrl Pts',(97.1765640031537,-0.935050866663774,
-6.39971867776693));
#28967=CARTESIAN_POINT('Ctrl Pts',(97.1765332480948,-0.935074418786677,
-6.39972132087734));
#28968=CARTESIAN_POINT('Ctrl Pts',(97.1765177322304,-0.935086300171969,
-6.39972265426901));
#28969=CARTESIAN_POINT('Ctrl Pts',(97.1764864154705,-0.935110279970557,
-6.3997253454419));
#28970=CARTESIAN_POINT('Ctrl Pts',(97.176470614582,-0.935122378355964,-6.3997267032206));
#28971=CARTESIAN_POINT('Ctrl Pts',(97.1764387189249,-0.935146798861671,
-6.39972944392213));
#28972=CARTESIAN_POINT('Ctrl Pts',(97.1764226237246,-0.935159121288783,
-6.39973082688002));
#28973=CARTESIAN_POINT('Ctrl Pts',(97.1763901295677,-0.935183997367168,
-6.39973361878238));
#28974=CARTESIAN_POINT('Ctrl Pts',(97.1763737309863,-0.935196550706058,
-6.39973502769248));
#28975=CARTESIAN_POINT('Ctrl Pts',(97.176340619982,-0.935221896252795,-6.39973787235927));
#28976=CARTESIAN_POINT('Ctrl Pts',(97.1763239078118,-0.935234688240603,
-6.399739308092));
#28977=CARTESIAN_POINT('Ctrl Pts',(97.1762901597669,-0.935260518554863,
-6.39974220724458));
#28978=CARTESIAN_POINT('Ctrl Pts',(97.1762731234986,-0.93527355715472,-6.39974367069588));
#28979=CARTESIAN_POINT('Ctrl Pts',(97.1762387164617,-0.935299888871347,
-6.39974662620581));
#28980=CARTESIAN_POINT('Ctrl Pts',(97.1762213456232,-0.935313182012339,
-6.39974811826794));
#28981=CARTESIAN_POINT('Ctrl Pts',(97.1761862580939,-0.935340031410167,
-6.39975113196709));
#28982=CARTESIAN_POINT('Ctrl Pts',(97.1761685412761,-0.935353587733377,
-6.39975265361238));
#28983=CARTESIAN_POINT('Ctrl Pts',(97.1761327497733,-0.935380972595524,
-6.39975572750177));
#28984=CARTESIAN_POINT('Ctrl Pts',(97.1761146753163,-0.935394800927575,
-6.39975727972353));
#28985=CARTESIAN_POINT('Ctrl Pts',(97.1760781562237,-0.935422739128583,
-6.39976041581479));
#28986=CARTESIAN_POINT('Ctrl Pts',(97.1760597115915,-0.935436848960471,
-6.39976199968107));
#28987=CARTESIAN_POINT('Ctrl Pts',(97.1760224395259,-0.935465359713352,
-6.3997652001364));
#28988=CARTESIAN_POINT('Ctrl Pts',(97.1760036117627,-0.935479760850346,
-6.39976681675068));
#28989=CARTESIAN_POINT('Ctrl Pts',(97.1759655597604,-0.935508864563288,
-6.39977008386683));
#28990=CARTESIAN_POINT('Ctrl Pts',(97.1759463355762,-0.935523567058997,
-6.39977173436072));
#28991=CARTESIAN_POINT('Ctrl Pts',(97.1759074762203,-0.935553284471883,
-6.39977507047207));
#28992=CARTESIAN_POINT('Ctrl Pts',(97.1758878414116,-0.935568299070985,
-6.39977675605493));
#28993=CARTESIAN_POINT('Ctrl Pts',(97.175848146239,-0.935598651707898,-6.39978016358431));
#28994=CARTESIAN_POINT('Ctrl Pts',(97.1758280856368,-0.935613989885082,
-6.39978188554764));
#28995=CARTESIAN_POINT('Ctrl Pts',(97.1757875228418,-0.935645001809037,
-6.39978536720339));
#28996=CARTESIAN_POINT('Ctrl Pts',(97.1757670213753,-0.935660674955053,
-6.39978712682958));
#28997=CARTESIAN_POINT('Ctrl Pts',(97.1757255610698,-0.935692368744376,
-6.39979068515381));
#28998=CARTESIAN_POINT('Ctrl Pts',(97.1757046015927,-0.935708389827328,
-6.39979248390251));
#28999=CARTESIAN_POINT('Ctrl Pts',(97.1756622083148,-0.935740792302029,
-6.3997961219141));
#29000=CARTESIAN_POINT('Ctrl Pts',(97.1756407741983,-0.935757173884042,
-6.39979796119972));
#29001=CARTESIAN_POINT('Ctrl Pts',(97.1755974129087,-0.935790311519394,
-6.39980168187941));
#29002=CARTESIAN_POINT('Ctrl Pts',(97.1755754862566,-0.935807067120386,
-6.39980356322415));
#29003=CARTESIAN_POINT('Ctrl Pts',(97.1755311209366,-0.935840967117804,
-6.3998073696348));
#29004=CARTESIAN_POINT('Ctrl Pts',(97.1755086823097,-0.935858111425278,
-6.39980929469228));
#29005=CARTESIAN_POINT('Ctrl Pts',(97.1754632737502,-0.935892803399708,
-6.3998131901684));
#29006=CARTESIAN_POINT('Ctrl Pts',(97.1754403030439,-0.935910351596695,
-6.39981516064821));
#29007=CARTESIAN_POINT('Ctrl Pts',(97.1753938086935,-0.935945867690039,
-6.39981914880877));
#29008=CARTESIAN_POINT('Ctrl Pts',(97.175370285554,-0.935963835136047,-6.3998211664407));
#29009=CARTESIAN_POINT('Ctrl Pts',(97.1753226644333,-0.936000206261072,
-6.39982525076739));
#29010=CARTESIAN_POINT('Ctrl Pts',(97.1752985659007,-0.936018610291878,
-6.39982731750352));
#29011=CARTESIAN_POINT('Ctrl Pts',(97.1752497704901,-0.936055872326055,
-6.39983150203635));
#29012=CARTESIAN_POINT('Ctrl Pts',(97.1752250737634,-0.93607473013996,-6.39983361981377));
#29013=CARTESIAN_POINT('Ctrl Pts',(97.1751750569551,-0.936112918612804,
-6.39983790855459));
#29014=CARTESIAN_POINT('Ctrl Pts',(97.1751497371715,-0.936132248965399,
-6.3998400794857));
#29015=CARTESIAN_POINT('Ctrl Pts',(97.1750984484514,-0.936171401971825,
-6.39984447672537));
#29016=CARTESIAN_POINT('Ctrl Pts',(97.1750724793537,-0.936191224664462,
-6.39984670304055));
#29017=CARTESIAN_POINT('Ctrl Pts',(97.1750198647355,-0.936231382911131,
-6.39985121336431));
#29018=CARTESIAN_POINT('Ctrl Pts',(97.1749932188897,-0.936251718623376,
-6.39985349739307));
#29019=CARTESIAN_POINT('Ctrl Pts',(97.1726272253054,-0.938057249818427,
-6.40005629199058));
#29020=CARTESIAN_POINT('Ctrl Pts',(97.1702812367697,-0.939833641971995,
-6.40025617973369));
#29021=CARTESIAN_POINT('Ctrl Pts',(97.1648112135038,-0.943943401375891,
-6.4007195121245));
#29022=CARTESIAN_POINT('Ctrl Pts',(97.1616822271723,-0.946270064555444,
-6.40098249706385));
#29023=CARTESIAN_POINT('Ctrl Pts',(97.1534614175341,-0.952319757004328,
-6.40166825470613));
#29024=CARTESIAN_POINT('Ctrl Pts',(97.1483510589329,-0.956017555007129,
-6.40208938309798));
#29025=CARTESIAN_POINT('Ctrl Pts',(97.1085855381425,-0.984307488837633,
-6.40532871813222));
#29026=CARTESIAN_POINT('Ctrl Pts',(97.0726478678027,-1.00705179393989,-6.40803731318252));
#29027=CARTESIAN_POINT('Ctrl Pts',(96.974726766229,-1.06184026835491,-6.41507365534411));
#29028=CARTESIAN_POINT('Ctrl Pts',(96.9109965698694,-1.09040800905937,-6.41932072037774));
#29029=CARTESIAN_POINT('Ctrl Pts',(96.7962659261205,-1.13005062010819,-6.42692029284604));
#29030=CARTESIAN_POINT('Ctrl Pts',(96.7463667607831,-1.1436932509894,-6.43020986564444));
#29031=CARTESIAN_POINT('Ctrl Pts',(96.6852005769809,-1.15616252520353,-6.43431330533018));
#29032=CARTESIAN_POINT('Ctrl Pts',(96.6746353788666,-1.1581660345286,-6.43502445352717));
#29033=CARTESIAN_POINT('Ctrl Pts',(96.6579321488437,-1.16109715261995,-6.43615315177178));
#29034=CARTESIAN_POINT('Ctrl Pts',(96.6518115094343,-1.16212141719024,-6.43656767040178));
#29035=CARTESIAN_POINT('Ctrl Pts',(96.6403206498091,-1.1639511288432,-6.43734774799026));
#29036=CARTESIAN_POINT('Ctrl Pts',(96.6349523784064,-1.16476790260801,-6.43771294208083));
#29037=CARTESIAN_POINT('Ctrl Pts',(96.6228995297434,-1.16651653138184,-6.43853466898798));
#29038=CARTESIAN_POINT('Ctrl Pts',(96.6162122498106,-1.16742810143477,-6.43899182158177));
#29039=CARTESIAN_POINT('Ctrl Pts',(96.5991338949827,-1.16960677140402,-6.44016263646328));
#29040=CARTESIAN_POINT('Ctrl Pts',(96.5887332699213,-1.1707928805093,-6.44087878075132));
#29041=CARTESIAN_POINT('Ctrl Pts',(96.5056709254437,-1.17914543877384,-6.44662444135765));
#29042=CARTESIAN_POINT('Ctrl Pts',(96.4325147777633,-1.17967811561584,-6.45186034899469));
#29043=CARTESIAN_POINT('Ctrl Pts',(96.3073637923528,-1.168939340988,-6.46104153441184));
#29044=CARTESIAN_POINT('Ctrl Pts',(96.255295850227,-1.16093203051648,-6.46492501050388));
#29045=CARTESIAN_POINT('Ctrl Pts',(96.1673718958634,-1.14130881234261,-6.47146845917004));
#29046=CARTESIAN_POINT('Ctrl Pts',(96.1312121400617,-1.13140681559021,-6.47415411926335));
#29047=CARTESIAN_POINT('Ctrl Pts',(96.0893553617421,-1.11776730841211,-6.47721236552547));
#29048=CARTESIAN_POINT('Ctrl Pts',(96.0831450520231,-1.11568614898265,-6.47766476742238));
#29049=CARTESIAN_POINT('Ctrl Pts',(96.0735720207166,-1.11238901676735,-6.47835969674646));
#29050=CARTESIAN_POINT('Ctrl Pts',(96.0701970517253,-1.11120939691399,-6.47860422285097));
#29051=CARTESIAN_POINT('Ctrl Pts',(96.0639536157802,-1.10899523609807,-6.47905563591088));
#29052=CARTESIAN_POINT('Ctrl Pts',(96.0610838014874,-1.10796492660114,-6.47926275121671));
#29053=CARTESIAN_POINT('Ctrl Pts',(96.0545176940618,-1.10557876132467,-6.47973579273178));
#29054=CARTESIAN_POINT('Ctrl Pts',(96.0508241706686,-1.10421550746967,-6.48000128349502));
#29055=CARTESIAN_POINT('Ctrl Pts',(96.0411117273122,-1.10057527154522,-6.4806980017482));
#29056=CARTESIAN_POINT('Ctrl Pts',(96.0351044146951,-1.09826739959844,-6.48112749848271));
#29057=CARTESIAN_POINT('Ctrl Pts',(95.9774134751159,-1.0755594834283,-6.48524106150865));
#29058=CARTESIAN_POINT('Ctrl Pts',(95.927208265915,-1.05157231623784,-6.48873639132756));
#29059=CARTESIAN_POINT('Ctrl Pts',(95.8338632344687,-0.998561590404792,
-6.49541014934479));
#29060=CARTESIAN_POINT('Ctrl Pts',(95.790582438158,-0.97005721240322,-6.49858717043135));
#29061=CARTESIAN_POINT('Ctrl Pts',(95.7196953881159,-0.916358448787677,
-6.5041389808654));
#29062=CARTESIAN_POINT('Ctrl Pts',(95.6911540623524,-0.892531158635892,
-6.50648334342522));
#29063=CARTESIAN_POINT('Ctrl Pts',(95.6520428067932,-0.856607943268382,
-6.5099022168641));
#29064=CARTESIAN_POINT('Ctrl Pts',(95.6405181628985,-0.845582870540394,
-6.51093722844887));
#29065=CARTESIAN_POINT('Ctrl Pts',(95.6203071008332,-0.825446127901601,
-6.51280592782262));
#29066=CARTESIAN_POINT('Ctrl Pts',(95.6115360733511,-0.816422674540213,
-6.51363590402667));
#29067=CARTESIAN_POINT('Ctrl Pts',(95.5983931846207,-0.802460717810089,
-6.51491011450978));
#29068=CARTESIAN_POINT('Ctrl Pts',(95.5939152535625,-0.797622974617202,
-6.515349843546));
#29069=CARTESIAN_POINT('Ctrl Pts',(95.5861832954868,-0.789127769847707,
-6.51611909496769));
#29070=CARTESIAN_POINT('Ctrl Pts',(95.5829109903501,-0.785487103980146,
-6.51644784319417));
#29071=CARTESIAN_POINT('Ctrl Pts',(95.5755882911183,-0.777237219476801,
-6.51719081003168));
#29072=CARTESIAN_POINT('Ctrl Pts',(95.5715510561389,-0.772616563651018,
-6.51760555752859));
#29073=CARTESIAN_POINT('Ctrl Pts',(95.5607483031821,-0.760055945659862,
-6.51872943611682));
#29074=CARTESIAN_POINT('Ctrl Pts',(95.554051997889,-0.752057457194885,-6.51944133570553));
#29075=CARTESIAN_POINT('Ctrl Pts',(95.5221794040186,-0.712942708511678,
-6.52290560649131));
#29076=CARTESIAN_POINT('Ctrl Pts',(95.4984968191547,-0.68064894314274,-6.52571556007509));
#29077=CARTESIAN_POINT('Ctrl Pts',(95.4304701434541,-0.577226604646416,
-6.53456693571664));
#29078=CARTESIAN_POINT('Ctrl Pts',(95.3920358304643,-0.502528974669699,
-6.54077664937646));
#29079=CARTESIAN_POINT('Ctrl Pts',(95.3517827984149,-0.398327278726985,
-6.54891112455067));
#29080=CARTESIAN_POINT('Ctrl Pts',(95.3426419881288,-0.371903851937086,
-6.55092928806967));
#29081=CARTESIAN_POINT('Ctrl Pts',(95.3312493144708,-0.334739007166689,
-6.55368602527304));
#29082=CARTESIAN_POINT('Ctrl Pts',(95.3281943239646,-0.324255000209573,
-6.55445478043008));
#29083=CARTESIAN_POINT('Ctrl Pts',(95.3231176488982,-0.305885619880339,
-6.55578454906964));
#29084=CARTESIAN_POINT('Ctrl Pts',(95.3210311172284,-0.298019091548349,
-6.55634856004119));
#29085=CARTESIAN_POINT('Ctrl Pts',(95.3180657794199,-0.286352653404706,
-6.55717635182223));
#29086=CARTESIAN_POINT('Ctrl Pts',(95.3171240869654,-0.282569193178977,
-6.55744346636159));
#29087=CARTESIAN_POINT('Ctrl Pts',(95.3155487410907,-0.276103056568104,
-6.55789761302853));
#29088=CARTESIAN_POINT('Ctrl Pts',(95.3149056974572,-0.273422753625324,
-6.55808516811796));
#29089=CARTESIAN_POINT('Ctrl Pts',(95.3134705907885,-0.267347067597208,
-6.55850872903258));
#29090=CARTESIAN_POINT('Ctrl Pts',(95.3126841898141,-0.263950405931354,
-6.55874441334441));
#29091=CARTESIAN_POINT('Ctrl Pts',(95.3105895415945,-0.254716693399316,
-6.5593822244395));
#29092=CARTESIAN_POINT('Ctrl Pts',(95.3093106396925,-0.248872990540468,
-6.55978274533025));
#29093=CARTESIAN_POINT('Ctrl Pts',(95.3031594006712,-0.219703675746438,
-6.56176757172747));
#29094=CARTESIAN_POINT('Ctrl Pts',(95.2989508532001,-0.196241923921446,
-6.5633182615217));
#29095=CARTESIAN_POINT('Ctrl Pts',(95.28055041391,-0.0720897623782146,-6.57136088446545));
#29096=CARTESIAN_POINT('Ctrl Pts',(95.2787294633223,0.0299997297889832,
-6.5774483670772));
#29097=CARTESIAN_POINT('Ctrl Pts',(95.2946345108674,0.172038832414202,-6.58647284917655));
#29098=CARTESIAN_POINT('Ctrl Pts',(95.3013713462114,0.212743129651664,-6.58911931492783));
#29099=CARTESIAN_POINT('Ctrl Pts',(95.3124049792911,0.26290557756243,-6.59249998636938));
#29100=CARTESIAN_POINT('Ctrl Pts',(95.3147097747432,0.272774963421777,-6.59317089344754));
#29101=CARTESIAN_POINT('Ctrl Pts',(95.3185984818661,0.288507112559284,-6.59425015523625));
#29102=CARTESIAN_POINT('Ctrl Pts',(95.320100900015,0.294389647052842,-6.59465591874002));
#29103=CARTESIAN_POINT('Ctrl Pts',(95.3230382809119,0.305530597296265,-6.59542871647041));
#29104=CARTESIAN_POINT('Ctrl Pts',(95.3244644001965,0.310791197117744,-6.59579545942917));
#29105=CARTESIAN_POINT('Ctrl Pts',(95.3277951677745,0.322748278822231,-6.59663333581609));
#29106=CARTESIAN_POINT('Ctrl Pts',(95.3297227672705,0.329438099385787,-6.59710519450473));
#29107=CARTESIAN_POINT('Ctrl Pts',(95.3358338968934,0.34996132691847,-6.59856248836821));
#29108=CARTESIAN_POINT('Ctrl Pts',(95.3402126930636,0.363734690005359,-6.59955415518562));
#29109=CARTESIAN_POINT('Ctrl Pts',(95.3754852987348,0.467998034780265,-6.60716887558589));
#29110=CARTESIAN_POINT('Ctrl Pts',(95.4170375677854,0.554487657150009,-6.61415289534093));
#29111=CARTESIAN_POINT('Ctrl Pts',(95.5010504861476,0.685724126710215,-6.62558519956806));
#29112=CARTESIAN_POINT('Ctrl Pts',(95.5373800074524,0.733900986044459,-6.62998846673897));
#29113=CARTESIAN_POINT('Ctrl Pts',(95.5826708531864,0.785246382824889,-6.6347665464085));
#29114=CARTESIAN_POINT('Ctrl Pts',(95.5881654461936,0.791345764529782,-6.6353355394489));
#29115=CARTESIAN_POINT('Ctrl Pts',(95.5963724363439,0.800266734892986,-6.63616919785251));
#29116=CARTESIAN_POINT('Ctrl Pts',(95.5990356998227,0.803132898344301,-6.63643726346569));
#29117=CARTESIAN_POINT('Ctrl Pts',(95.6037985737718,0.808207680542341,-6.63691221283939));
#29118=CARTESIAN_POINT('Ctrl Pts',(95.6058925230498,0.810421476686974,-6.6371195057559));
#29119=CARTESIAN_POINT('Ctrl Pts',(95.6104741235883,0.815227800589587,-6.63756977142483));
#29120=CARTESIAN_POINT('Ctrl Pts',(95.6129650577297,0.817817085301619,-6.63781249003034));
#29121=CARTESIAN_POINT('Ctrl Pts',(95.6199604459838,0.825022388779438,-6.63848847279569));
#29122=CARTESIAN_POINT('Ctrl Pts',(95.6244911085802,0.829612951522574,-6.63891979614913));
#29123=CARTESIAN_POINT('Ctrl Pts',(95.6510059526397,0.856040554960753,-6.64140838579666));
#29124=CARTESIAN_POINT('Ctrl Pts',(95.6738094448802,0.877042485824854,-6.64340815425057));
#29125=CARTESIAN_POINT('Ctrl Pts',(95.756649359032,0.947503505260597,-6.65030947190125));
#29126=CARTESIAN_POINT('Ctrl Pts',(95.8207282619404,0.991897012846869,-6.65502945493974));
#29127=CARTESIAN_POINT('Ctrl Pts',(95.8996533305313,1.03572384359127,-6.66066653919875));
#29128=CARTESIAN_POINT('Ctrl Pts',(95.9106824222252,1.04162036581191,-6.66145022930411));
#29129=CARTESIAN_POINT('Ctrl Pts',(95.9218016806086,1.0473393469567,-6.66223764680097));
#29130=CARTESIAN_POINT('Origin',(96.460480949577,-7.19464945638997E-16,
0.924367114736168));
#29131=CARTESIAN_POINT('',(95.9218016730718,1.04733934308027,-7.26047246820102));
#29132=CARTESIAN_POINT('',(95.921801726504,1.0473393705621,-7.16216478479583));
#29133=CARTESIAN_POINT('',(95.9218016730721,1.04733934308042,0.924367114736168));
#29134=CARTESIAN_POINT('',(97.6382304460792,-0.00103044978340366,-6.92454726424663));
#29135=CARTESIAN_POINT('Ctrl Pts',(95.9218016730718,1.04733934308028,-7.26047246820102));
#29136=CARTESIAN_POINT('Ctrl Pts',(95.9208597180712,1.04685486625662,-7.26040005122408));
#29137=CARTESIAN_POINT('Ctrl Pts',(95.9199184113506,1.04636911593881,-7.26032771122568));
#29138=CARTESIAN_POINT('Ctrl Pts',(95.9162760713822,1.04448330229007,-7.26004790400432));
#29139=CARTESIAN_POINT('Ctrl Pts',(95.9135798251374,1.04307405247191,-7.25984101423793));
#29140=CARTESIAN_POINT('Ctrl Pts',(95.9076501070122,1.03994544687482,-7.25938653821152));
#29141=CARTESIAN_POINT('Ctrl Pts',(95.9044191777612,1.03822145027119,-7.25913924365669));
#29142=CARTESIAN_POINT('Ctrl Pts',(95.8950714447966,1.03317742467046,-7.25842459306972));
#29143=CARTESIAN_POINT('Ctrl Pts',(95.8889758342753,1.02981814312404,-7.25795959984589));
#29144=CARTESIAN_POINT('Ctrl Pts',(95.8373899156303,1.00079010748118,-7.25403012205844));
#29145=CARTESIAN_POINT('Ctrl Pts',(95.7936176456544,0.972171835076872,-7.25073235653692));
#29146=CARTESIAN_POINT('Ctrl Pts',(95.6853708012808,0.890636646085197,-7.2422909419277));
#29147=CARTESIAN_POINT('Ctrl Pts',(95.6243603345841,0.833625394649087,-7.23722359809865));
#29148=CARTESIAN_POINT('Ctrl Pts',(95.549773628956,0.747429416561308,-7.22995249652568));
#29149=CARTESIAN_POINT('Ctrl Pts',(95.530592372067,0.723426247829695,-7.22796519482068));
#29150=CARTESIAN_POINT('Ctrl Pts',(95.5066989546608,0.691003923233239,-7.22531086301413));
#29151=CARTESIAN_POINT('Ctrl Pts',(95.5011197343357,0.683236829786034,-7.22467718615597));
#29152=CARTESIAN_POINT('Ctrl Pts',(95.4922254070386,0.670530859955909,-7.22364362359592));
#29153=CARTESIAN_POINT('Ctrl Pts',(95.4888519686875,0.665633195619573,-7.22324594737691));
#29154=CARTESIAN_POINT('Ctrl Pts',(95.4824398263498,0.656171234003264,-7.22247892896844));
#29155=CARTESIAN_POINT('Ctrl Pts',(95.4793956141347,0.651610842368795,-7.22210980528191));
#29156=CARTESIAN_POINT('Ctrl Pts',(95.4724214973662,0.641003579469308,-7.22125242868399));
#29157=CARTESIAN_POINT('Ctrl Pts',(95.468515102082,0.634941590538616,-7.22076332611468));
#29158=CARTESIAN_POINT('Ctrl Pts',(95.4562314263832,0.615489580921559,-7.21919642095604));
#29159=CARTESIAN_POINT('Ctrl Pts',(95.4480680248331,0.601967239079183,-7.21811095169418));
#29160=CARTESIAN_POINT('Ctrl Pts',(95.4295082222155,0.569777765867103,-7.21553459434246));
#29161=CARTESIAN_POINT('Ctrl Pts',(95.4193432675725,0.550984297282275,-7.21403617994727));
#29162=CARTESIAN_POINT('Ctrl Pts',(95.3827879980073,0.478771694850923,-7.2082997182316));
#29163=CARTESIAN_POINT('Ctrl Pts',(95.3599552648316,0.42365813462929,-7.20395848604041));
#29164=CARTESIAN_POINT('Ctrl Pts',(95.3195427015775,0.300448730435618,-7.19444577167821));
#29165=CARTESIAN_POINT('Ctrl Pts',(95.3036831961164,0.232013488983423,-7.18928031076791));
#29166=CARTESIAN_POINT('Ctrl Pts',(95.2926462473488,0.1528203160044,-7.18367589446421));
#29167=CARTESIAN_POINT('Ctrl Pts',(95.2914098320819,0.143054810241082,-7.18299132878215));
#29168=CARTESIAN_POINT('Ctrl Pts',(95.2898554532965,0.129406963909059,-7.1820447388615));
#29169=CARTESIAN_POINT('Ctrl Pts',(95.2894341343718,0.125537136038314,-7.18177746831511));
#29170=CARTESIAN_POINT('Ctrl Pts',(95.2887380323313,0.118834744115188,-7.18131660860916));
#29171=CARTESIAN_POINT('Ctrl Pts',(95.2884543179673,0.116003171342957,-7.18112253853675));
#29172=CARTESIAN_POINT('Ctrl Pts',(95.2878747106748,0.10999919222908,-7.18071241289187));
#29173=CARTESIAN_POINT('Ctrl Pts',(95.2875814222413,0.10682655609912,-7.18049650762431));
#29174=CARTESIAN_POINT('Ctrl Pts',(95.2868813143617,0.0989024760366053,
-7.17995920056615));
#29175=CARTESIAN_POINT('Ctrl Pts',(95.2864904661398,0.0941496165057984,
-7.179638668394));
#29176=CARTESIAN_POINT('Ctrl Pts',(95.2851006452773,0.0758918809506207,
-7.17841361194429));
#29177=CARTESIAN_POINT('Ctrl Pts',(95.284305698751,0.0623719110757795,-7.1775195511536));
#29178=CARTESIAN_POINT('Ctrl Pts',(95.2828493126887,0.0272825526794893,
-7.17522610452706));
#29179=CARTESIAN_POINT('Ctrl Pts',(95.282547079335,0.00570270419554888,
-7.17384199628592));
#29180=CARTESIAN_POINT('Ctrl Pts',(95.2842025494585,-0.117107522713611,
-7.16605448070247));
#29181=CARTESIAN_POINT('Ctrl Pts',(95.2986139016332,-0.217743232586888,
-7.15998149464462));
#29182=CARTESIAN_POINT('Ctrl Pts',(95.3346706671793,-0.347511047007553,
-7.15141632201767));
#29183=CARTESIAN_POINT('Ctrl Pts',(95.3449874073226,-0.379323814872747,
-7.1492584789627));
#29184=CARTESIAN_POINT('Ctrl Pts',(95.3600810426165,-0.419895658609567,
-7.14640748089808));
#29185=CARTESIAN_POINT('Ctrl Pts',(95.3636355121046,-0.429094856590577,
-7.14575434176744));
#29186=CARTESIAN_POINT('Ctrl Pts',(95.3695421689451,-0.443828554419652,
-7.14469688489526));
#29187=CARTESIAN_POINT('Ctrl Pts',(95.3718220003918,-0.449391698741871,
-7.14429497306278));
#29188=CARTESIAN_POINT('Ctrl Pts',(95.3762550846813,-0.459977387230508,
-7.14352503560608));
#29189=CARTESIAN_POINT('Ctrl Pts',(95.3784009005822,-0.465002891080957,
-7.14315726713749));
#29190=CARTESIAN_POINT('Ctrl Pts',(95.3834047900295,-0.476499795760483,
-7.1423106600264));
#29191=CARTESIAN_POINT('Ctrl Pts',(95.3862863311969,-0.48296068876288,-7.14183104041683));
#29192=CARTESIAN_POINT('Ctrl Pts',(95.3954780030865,-0.503080680124973,
-7.14032511902933));
#29193=CARTESIAN_POINT('Ctrl Pts',(95.4019915724351,-0.516644606023258,
-7.13929196806175));
#29194=CARTESIAN_POINT('Ctrl Pts',(95.4177902270503,-0.547990336991621,
-7.13686109665307));
#29195=CARTESIAN_POINT('Ctrl Pts',(95.4272730842841,-0.565666666295478,
-7.13545695361596));
#29196=CARTESIAN_POINT('Ctrl Pts',(95.4636608857215,-0.629524349062002,
-7.1302599023813));
#29197=CARTESIAN_POINT('Ctrl Pts',(95.4932465663937,-0.674097670688097,
-7.12638399706332));
#29198=CARTESIAN_POINT('Ctrl Pts',(95.5740446875582,-0.779504297028057,
-7.11665735681072));
#29199=CARTESIAN_POINT('Ctrl Pts',(95.62858543295,-0.837465206029179,-7.11077792168826));
#29200=CARTESIAN_POINT('Ctrl Pts',(95.6957594850679,-0.895760769046088,
-7.10455068856831));
#29201=CARTESIAN_POINT('Ctrl Pts',(95.7030486728573,-0.901932721639979,
-7.10388709292501));
#29202=CARTESIAN_POINT('Ctrl Pts',(95.7133007831966,-0.910401503095874,
-7.10297142093866));
#29203=CARTESIAN_POINT('Ctrl Pts',(95.7162005663911,-0.912773690484297,
-7.10271435786222));
#29204=CARTESIAN_POINT('Ctrl Pts',(95.7215130223108,-0.917077431853546,
-7.10224700266729));
#29205=CARTESIAN_POINT('Ctrl Pts',(95.7239220718261,-0.919013402527863,
-7.10203640413542));
#29206=CARTESIAN_POINT('Ctrl Pts',(95.728930227221,-0.923005734727604,-7.10160139161262));
#29207=CARTESIAN_POINT('Ctrl Pts',(95.7315304268305,-0.925060636820044,
-7.10137707799624));
#29208=CARTESIAN_POINT('Ctrl Pts',(95.7383558275954,-0.930408008604561,
-7.10079218272046));
#29209=CARTESIAN_POINT('Ctrl Pts',(95.7425949361117,-0.93368272376813,-7.10043281518524));
#29210=CARTESIAN_POINT('Ctrl Pts',(95.7617024237202,-0.948236207503202,
-7.09882963138234));
#29211=CARTESIAN_POINT('Ctrl Pts',(95.7768161991651,-0.959190250880203,
-7.09760633348266));
#29212=CARTESIAN_POINT('Ctrl Pts',(95.8206129299226,-0.989371472369909,
-7.09416694190529));
#29213=CARTESIAN_POINT('Ctrl Pts',(95.8498907613682,-1.00770380980554,-7.09199202535038));
#29214=CARTESIAN_POINT('Ctrl Pts',(95.9479093735551,-1.06323525555173,-7.08496662368879));
#29215=CARTESIAN_POINT('Ctrl Pts',(96.0195458572858,-1.09488582035073,-7.08021051329017));
#29216=CARTESIAN_POINT('Ctrl Pts',(96.1285784333299,-1.13060870515844,-7.07293827403741));
#29217=CARTESIAN_POINT('Ctrl Pts',(96.1638778151523,-1.14037778623842,-7.07058161408795));
#29218=CARTESIAN_POINT('Ctrl Pts',(96.2094865454845,-1.15073899573484,-7.06750332380953));
#29219=CARTESIAN_POINT('Ctrl Pts',(96.2194292591178,-1.15286274079395,-7.06683032951213));
#29220=CARTESIAN_POINT('Ctrl Pts',(96.2353585167992,-1.15605013012008,-7.06574848073897));
#29221=CARTESIAN_POINT('Ctrl Pts',(96.2413281094346,-1.15719663126365,-7.0653422394339));
#29222=CARTESIAN_POINT('Ctrl Pts',(96.2526658383167,-1.15928324431396,-7.06456902719351));
#29223=CARTESIAN_POINT('Ctrl Pts',(96.2580321629237,-1.16023241123785,-7.06420235139753));
#29224=CARTESIAN_POINT('Ctrl Pts',(96.2702574620156,-1.16230735991896,-7.06336531956014));
#29225=CARTESIAN_POINT('Ctrl Pts',(96.2771201501804,-1.1634097248192,-7.06289424406003));
#29226=CARTESIAN_POINT('Ctrl Pts',(96.2982203883794,-1.16660776114289,-7.06144194293551));
#29227=CARTESIAN_POINT('Ctrl Pts',(96.3124864635607,-1.16850321283646,-7.06045454795605));
#29228=CARTESIAN_POINT('Ctrl Pts',(96.3822301989317,-1.17647201107858,-7.05559866299609));
#29229=CARTESIAN_POINT('Ctrl Pts',(96.4380493536092,-1.17885740816322,-7.05161896937105));
#29230=CARTESIAN_POINT('Ctrl Pts',(96.5113505659212,-1.17678158475051,-7.04629107032982));
#29231=CARTESIAN_POINT('Ctrl Pts',(96.5288670947054,-1.17589367120393,-7.04501069102188));
#29232=CARTESIAN_POINT('Ctrl Pts',(96.626849917006,-1.1687301596835,-7.03781801478963));
#29233=CARTESIAN_POINT('Ctrl Pts',(96.706530149574,-1.15458674167189,-7.03183599012591));
#29234=CARTESIAN_POINT('Ctrl Pts',(96.7932187250978,-1.12980960832299,-7.02552511159158));
#29235=CARTESIAN_POINT('Ctrl Pts',(96.8022642197074,-1.12710620113606,-7.02486930687755));
#29236=CARTESIAN_POINT('Ctrl Pts',(96.8148362527548,-1.12318354976671,-7.02396252156958));
#29237=CARTESIAN_POINT('Ctrl Pts',(96.8183906922109,-1.12205596314794,-7.02370667720276));
#29238=CARTESIAN_POINT('Ctrl Pts',(96.8248770695408,-1.11996430974583,-7.0232408359018));
#29239=CARTESIAN_POINT('Ctrl Pts',(96.8278106868398,-1.11900556404084,-7.02303053969552));
#29240=CARTESIAN_POINT('Ctrl Pts',(96.8338945017082,-1.1169907876808,-7.02259527837974));
#29241=CARTESIAN_POINT('Ctrl Pts',(96.8370440404602,-1.11593294599405,-7.02237041927322));
#29242=CARTESIAN_POINT('Ctrl Pts',(96.8452950034731,-1.11312276982819,-7.02178248311324));
#29243=CARTESIAN_POINT('Ctrl Pts',(96.8503890120951,-1.11134866821537,-7.02142064343985));
#29244=CARTESIAN_POINT('Ctrl Pts',(96.8731326856828,-1.10325204894939,-7.01980946886404));
#29245=CARTESIAN_POINT('Ctrl Pts',(96.8906431706415,-1.09654324968982,-7.0185808125437));
#29246=CARTESIAN_POINT('Ctrl Pts',(96.9402778032874,-1.07615457341026,-7.01511183557275));
#29247=CARTESIAN_POINT('Ctrl Pts',(96.9719652400314,-1.06146025342563,-7.01291371710492));
#29248=CARTESIAN_POINT('Ctrl Pts',(97.0965942161623,-0.996787044247089,
-7.00416046050713));
#29249=CARTESIAN_POINT('Ctrl Pts',(97.183271811658,-0.935840105926767,-6.9977733110124));
#29250=CARTESIAN_POINT('Ctrl Pts',(97.2720171310125,-0.853664476248166,
-6.98989117853153));
#29251=CARTESIAN_POINT('Ctrl Pts',(97.2831510134443,-0.842940058212227,
-6.98887530735476));
#29252=CARTESIAN_POINT('Ctrl Pts',(97.2990671687752,-0.826993500780641,
-6.9873809816462));
#29253=CARTESIAN_POINT('Ctrl Pts',(97.3040188384712,-0.821942165673621,
-6.98690991780984));
#29254=CARTESIAN_POINT('Ctrl Pts',(97.3127258588277,-0.81289834267137,-6.98607036457632));
#29255=CARTESIAN_POINT('Ctrl Pts',(97.3164994383877,-0.808923634186177,
-6.98570267085466));
#29256=CARTESIAN_POINT('Ctrl Pts',(97.3243146759316,-0.800575925509163,
-6.98493300926392));
#29257=CARTESIAN_POINT('Ctrl Pts',(97.3283511774271,-0.796198332489722,
-6.98453083874448));
#29258=CARTESIAN_POINT('Ctrl Pts',(97.3382321643194,-0.785317967227464,
-6.98353467796098));
#29259=CARTESIAN_POINT('Ctrl Pts',(97.3440376853467,-0.778780451835088,
-6.98293909623894));
#29260=CARTESIAN_POINT('Ctrl Pts',(97.3692275591161,-0.749770246965699,
-6.98030856743592));
#29261=CARTESIAN_POINT('Ctrl Pts',(97.3878297739134,-0.726635885885746,
-6.97824255253814));
#29262=CARTESIAN_POINT('Ctrl Pts',(97.4367249598435,-0.660888833648281,
-6.9724516504901));
#29263=CARTESIAN_POINT('Ctrl Pts',(97.4650834474865,-0.616927201653601,
-6.96866492238197));
#29264=CARTESIAN_POINT('Ctrl Pts',(97.5298625280332,-0.500128977485876,
-6.95888825038202));
#29265=CARTESIAN_POINT('Ctrl Pts',(97.5618318478151,-0.425128321206344,
-6.95285989921297));
#29266=CARTESIAN_POINT('Ctrl Pts',(97.5885532574293,-0.338576064939547,
-6.94652023167593));
#29267=CARTESIAN_POINT('Ctrl Pts',(97.5911816327146,-0.329692071386415,
-6.94587666624319));
#29268=CARTESIAN_POINT('Ctrl Pts',(97.5947295362783,-0.317158250401129,
-6.94497960275223));
#29269=CARTESIAN_POINT('Ctrl Pts',(97.5957367391065,-0.313533898560549,
-6.94472147644937));
#29270=CARTESIAN_POINT('Ctrl Pts',(97.5975407703799,-0.306919534514355,
-6.94425279702013));
#29271=CARTESIAN_POINT('Ctrl Pts',(97.5983432127486,-0.303931090332096,
-6.94404193126013));
#29272=CARTESIAN_POINT('Ctrl Pts',(97.5999789103354,-0.297742164598787,
-6.94360711950385));
#29273=CARTESIAN_POINT('Ctrl Pts',(97.6008104754472,-0.29454129127137,-6.94338326905021));
#29274=CARTESIAN_POINT('Ctrl Pts',(97.6029457055444,-0.286177734656938,
-6.94280095745395));
#29275=CARTESIAN_POINT('Ctrl Pts',(97.6042278798425,-0.281009566781523,
-6.94244369080399));
#29276=CARTESIAN_POINT('Ctrl Pts',(97.6069648810169,-0.269648153308233,
-6.94166355937552));
#29277=CARTESIAN_POINT('Ctrl Pts',(97.6084046780018,-0.263451417752321,
-6.94124147792089));
#29278=CARTESIAN_POINT('Ctrl Pts',(97.6125689502187,-0.244846245399837,
-6.9399836009899));
#29279=CARTESIAN_POINT('Ctrl Pts',(97.6151430339537,-0.232404699287403,
-6.93915490476511));
#29280=CARTESIAN_POINT('Ctrl Pts',(97.6312300440705,-0.147769664749213,
-6.93358689565391));
#29281=CARTESIAN_POINT('Ctrl Pts',(97.6381662002851,-0.0744864016200065,
-6.92909825428085));
#29282=CARTESIAN_POINT('Ctrl Pts',(97.6382304983754,-0.00103092444165349,
-6.92454738504961));
#29283=CARTESIAN_POINT('Ctrl Pts',(97.6382304987957,-0.00103044418824775,
-6.92454735529594));
#29284=CARTESIAN_POINT('Ctrl Pts',(97.6382908279616,0.0679229729281441,
-6.92027540704751));
#29285=CARTESIAN_POINT('Ctrl Pts',(97.63229585996,0.136742120609072,-6.9159638278707));
#29286=CARTESIAN_POINT('Ctrl Pts',(97.6186126308913,0.2142946587171,-6.91081892651751));
#29287=CARTESIAN_POINT('Ctrl Pts',(97.6167885836402,0.223928198828335,-6.91017491059771));
#29288=CARTESIAN_POINT('Ctrl Pts',(97.6135643146035,0.23986558290601,-6.90910069828434));
#29289=CARTESIAN_POINT('Ctrl Pts',(97.6122321235123,0.246182808429343,-6.9086726053109));
#29290=CARTESIAN_POINT('Ctrl Pts',(97.60973585836,0.257556077200189,-6.90789757002909));
#29291=CARTESIAN_POINT('Ctrl Pts',(97.6085901788517,0.262616020965674,-6.90755121101665));
#29292=CARTESIAN_POINT('Ctrl Pts',(97.6061790235561,0.272947570031992,-6.90684075135015));
#29293=CARTESIAN_POINT('Ctrl Pts',(97.6049105068863,0.278218330422606,-6.90647656218959));
#29294=CARTESIAN_POINT('Ctrl Pts',(97.6020831862839,0.289619414271739,-6.90568492548757));
#29295=CARTESIAN_POINT('Ctrl Pts',(97.6005113012784,0.295746287350625,-6.90525707139467));
#29296=CARTESIAN_POINT('Ctrl Pts',(97.5960696016152,0.312497331416325,-6.90408047169089));
#29297=CARTESIAN_POINT('Ctrl Pts',(97.593100172343,0.323094182481593,-6.90332857222809));
#29298=CARTESIAN_POINT('Ctrl Pts',(97.5751801613336,0.383759049595454,-6.89897913368304));
#29299=CARTESIAN_POINT('Ctrl Pts',(97.5570613007104,0.432822701760297,-6.89528048534449));
#29300=CARTESIAN_POINT('Ctrl Pts',(97.5161816469907,0.524300522489095,-6.88804133905029));
#29301=CARTESIAN_POINT('Ctrl Pts',(97.493959980958,0.566847112124095,-6.88451999508911));
#29302=CARTESIAN_POINT('Ctrl Pts',(97.4390221108619,0.658006278284554,-6.8767106198991));
#29303=CARTESIAN_POINT('Ctrl Pts',(97.4051441630644,0.705781753812096,-6.87243344213195));
#29304=CARTESIAN_POINT('Ctrl Pts',(97.3615984580203,0.758405275480429,-6.86764703812046));
#29305=CARTESIAN_POINT('Ctrl Pts',(97.3552489701487,0.765886108325646,-6.86696480929489));
#29306=CARTESIAN_POINT('Ctrl Pts',(97.3460017082658,0.776509044806948,-6.86599446395726));
#29307=CARTESIAN_POINT('Ctrl Pts',(97.3431793688538,0.779715853866698,-6.86570133129326));
#29308=CARTESIAN_POINT('Ctrl Pts',(97.3382841975529,0.785217218807283,-6.86519819959786));
#29309=CARTESIAN_POINT('Ctrl Pts',(97.3362196815034,0.787519077352361,-6.86498760543505));
#29310=CARTESIAN_POINT('Ctrl Pts',(97.3318730469432,0.792327182174312,-6.86454759450497));
#29311=CARTESIAN_POINT('Ctrl Pts',(97.3295891534876,0.794831731620892,-6.86431831231389));
#29312=CARTESIAN_POINT('Ctrl Pts',(97.3234375702759,0.801519425845047,-6.8637057506998));
#29313=CARTESIAN_POINT('Ctrl Pts',(97.3195502276695,0.80568449029458,-6.86332390311782));
#29314=CARTESIAN_POINT('Ctrl Pts',(97.301937772174,0.824282818984372,-6.86161635946472));
#29315=CARTESIAN_POINT('Ctrl Pts',(97.2878772024976,0.838395672404941,-6.86031385341831));
#29316=CARTESIAN_POINT('Ctrl Pts',(97.2153743632653,0.907566458257483,-6.85385215574387));
#29317=CARTESIAN_POINT('Ctrl Pts',(97.1517641694078,0.956907005852332,-6.84897337898678));
#29318=CARTESIAN_POINT('Ctrl Pts',(97.0467493897519,1.02238574811196,-6.84128454079765));
#29319=CARTESIAN_POINT('Ctrl Pts',(97.0086346080747,1.04331702700504,-6.8385611434389));
#29320=CARTESIAN_POINT('Ctrl Pts',(96.9535335695033,1.06972229523379,-6.83464100862845));
#29321=CARTESIAN_POINT('Ctrl Pts',(96.9374456875861,1.07699176643994,-6.83349861422961));
#29322=CARTESIAN_POINT('Ctrl Pts',(96.9087728354542,1.08917942379276,-6.83146183117773));
#29323=CARTESIAN_POINT('Ctrl Pts',(96.8962550494031,1.09424784293197,-6.8305723976577));
#29324=CARTESIAN_POINT('Ctrl Pts',(96.8775143074176,1.10146335148661,-6.82923911201458));
#29325=CARTESIAN_POINT('Ctrl Pts',(96.8713557408925,1.1037754477876,-6.8288007043033));
#29326=CARTESIAN_POINT('Ctrl Pts',(96.8600571879523,1.10790957590403,-6.82799575732531));
#29327=CARTESIAN_POINT('Ctrl Pts',(96.8549232674718,1.1097477437695,-6.82762975969184));
#29328=CARTESIAN_POINT('Ctrl Pts',(96.8440559650715,1.11355377636021,-6.82685443256345));
#29329=CARTESIAN_POINT('Ctrl Pts',(96.838319802003,1.11551315751356,-6.82644483811882));
#29330=CARTESIAN_POINT('Ctrl Pts',(96.8229971940445,1.12061537122909,-6.82534965653715));
#29331=CARTESIAN_POINT('Ctrl Pts',(96.8133852387631,1.12367939797443,-6.82466153947367));
#29332=CARTESIAN_POINT('Ctrl Pts',(96.7698718858962,1.13693689131066,-6.82154066108701));
#29333=CARTESIAN_POINT('Ctrl Pts',(96.7355638628342,1.14572125106972,-6.81906352414358));
#29334=CARTESIAN_POINT('Ctrl Pts',(96.6146572635333,1.17093498950523,-6.81027280933388));
#29335=CARTESIAN_POINT('Ctrl Pts',(96.5266586168271,1.17918458829314,-6.80374218019794));
#29336=CARTESIAN_POINT('Ctrl Pts',(96.3964666135989,1.17676305530942,-6.79425476426406));
#29337=CARTESIAN_POINT('Ctrl Pts',(96.3544215765119,1.17372115108118,-6.79122345119864));
#29338=CARTESIAN_POINT('Ctrl Pts',(96.3059657839785,1.16758947867422,-6.78782876884236));
#29339=CARTESIAN_POINT('Ctrl Pts',(96.2993130064042,1.16668977302475,-6.78736489481905));
#29340=CARTESIAN_POINT('Ctrl Pts',(96.2890948011554,1.16521881363432,-6.7866561715524));
#29341=CARTESIAN_POINT('Ctrl Pts',(96.285523832206,1.16468798546192,-6.78640920021549));
#29342=CARTESIAN_POINT('Ctrl Pts',(96.2789446103847,1.16367903542043,-6.78595554919555));
#29343=CARTESIAN_POINT('Ctrl Pts',(96.2759357714203,1.1632056643294,-6.78574862185241));
#29344=CARTESIAN_POINT('Ctrl Pts',(96.2690880848778,1.16210110054651,-6.78527888548373));
#29345=CARTESIAN_POINT('Ctrl Pts',(96.2652505025404,1.16146255651345,-6.78501648778175));
#29346=CARTESIAN_POINT('Ctrl Pts',(96.2552291311031,1.15974400521432,-6.78433333055051));
#29347=CARTESIAN_POINT('Ctrl Pts',(96.2490505916633,1.1586335376587,-6.7839141949466));
#29348=CARTESIAN_POINT('Ctrl Pts',(96.202964169312,1.14996949597904,-6.78080118937489));
#29349=CARTESIAN_POINT('Ctrl Pts',(96.1634573741443,1.14040453132776,-6.77820730946662));
#29350=CARTESIAN_POINT('Ctrl Pts',(96.0558335471731,1.10837323839852,-6.77115437793228));
#29351=CARTESIAN_POINT('Ctrl Pts',(95.9891556431021,1.08170410353104,-6.76679192197993));
#29352=CARTESIAN_POINT('Ctrl Pts',(95.9241423110083,1.04854072782659,-6.76222263069734));
#29353=CARTESIAN_POINT('Ctrl Pts',(95.9229714708682,1.04794100655766,-6.76214023561899));
#29354=CARTESIAN_POINT('Ctrl Pts',(95.9218016727113,1.04733934289486,-6.7620578065779));
#29355=CARTESIAN_POINT('Ctrl Pts',(95.9218016806086,1.0473393469567,-6.66223764680097));
#29356=CARTESIAN_POINT('Ctrl Pts',(95.9435181322099,1.05850879486024,-6.66377551141126));
#29357=CARTESIAN_POINT('Ctrl Pts',(95.9655785064204,1.06900103023623,-6.66532772277226));
#29358=CARTESIAN_POINT('Ctrl Pts',(96.0025003733893,1.08517332476905,-6.66792309340538));
#29359=CARTESIAN_POINT('Ctrl Pts',(96.0171764254609,1.09125084906102,-6.66895404657819));
#29360=CARTESIAN_POINT('Ctrl Pts',(96.0436542399985,1.10159334498987,-6.67081606135641));
#29361=CARTESIAN_POINT('Ctrl Pts',(96.0554098791637,1.10597007727781,-6.67164345074486));
#29362=CARTESIAN_POINT('Ctrl Pts',(96.0734388694618,1.11235643499293,-6.67291450491019));
#29363=CARTESIAN_POINT('Ctrl Pts',(96.0796631318412,1.11450266800341,-6.67335369934532));
#29364=CARTESIAN_POINT('Ctrl Pts',(96.0905451866241,1.11815318654723,-6.67412236561389));
#29365=CARTESIAN_POINT('Ctrl Pts',(96.0951950129957,1.11968084765166,-6.67445106721583));
#29366=CARTESIAN_POINT('Ctrl Pts',(96.1057009934111,1.12306009070981,-6.67519439221232));
#29367=CARTESIAN_POINT('Ctrl Pts',(96.11156234348,1.12489492331328,-6.67560954763513));
#29368=CARTESIAN_POINT('Ctrl Pts',(96.1274426587684,1.12973002900543,-6.67673569446181));
#29369=CARTESIAN_POINT('Ctrl Pts',(96.1374874767613,1.13264277063171,-6.67744947357175));
#29370=CARTESIAN_POINT('Ctrl Pts',(96.1865509212101,1.14616419647763,-6.68094390453352));
#29371=CARTESIAN_POINT('Ctrl Pts',(96.2260552812149,1.15489132280347,-6.68378339203293));
#29372=CARTESIAN_POINT('Ctrl Pts',(96.3481913215893,1.17534823930417,-6.69264163076331));
#29373=CARTESIAN_POINT('Ctrl Pts',(96.4316832959287,1.1803477172002,-6.69882464684398));
#29374=CARTESIAN_POINT('Ctrl Pts',(96.5428427901678,1.17519743417564,-6.70692750980104));
#29375=CARTESIAN_POINT('Ctrl Pts',(96.5706424745308,1.17291820978649,-6.70894070607248));
#29376=CARTESIAN_POINT('Ctrl Pts',(96.6091636745739,1.16837808984237,-6.71169136754974));
#29377=CARTESIAN_POINT('Ctrl Pts',(96.6199728173294,1.16695170278519,-6.71245888418601));
#29378=CARTESIAN_POINT('Ctrl Pts',(96.638803733818,1.16420020334963,-6.71378672745948));
#29379=CARTESIAN_POINT('Ctrl Pts',(96.64683435382,1.16294176412217,-6.71435004032614));
#29380=CARTESIAN_POINT('Ctrl Pts',(96.658695020026,1.16095711826751,-6.71517700961791));
#29381=CARTESIAN_POINT('Ctrl Pts',(96.6625353194276,1.16029491117584,-6.71544399049936));
#29382=CARTESIAN_POINT('Ctrl Pts',(96.6690859883181,1.15913182874012,-6.71589798717931));
#29383=CARTESIAN_POINT('Ctrl Pts',(96.6717979657275,1.15864048689156,-6.7160855249842));
#29384=CARTESIAN_POINT('Ctrl Pts',(96.6779378797579,1.15750581418434,-6.71650915109689));
#29385=CARTESIAN_POINT('Ctrl Pts',(96.6813647029323,1.15685677361167,-6.71674491719432));
#29386=CARTESIAN_POINT('Ctrl Pts',(96.6906662181432,1.15505222856155,-6.71738316899787));
#29387=CARTESIAN_POINT('Ctrl Pts',(96.696535161133,1.15386711605725,-6.71778404510473));
#29388=CARTESIAN_POINT('Ctrl Pts',(96.7257802248937,1.14772920002724,-6.71977358708758));
#29389=CARTESIAN_POINT('Ctrl Pts',(96.7490126445444,1.14211018263302,-6.72132844618114));
#29390=CARTESIAN_POINT('Ctrl Pts',(96.8548577064927,1.11307387229661,-6.72836092387237));
#29391=CARTESIAN_POINT('Ctrl Pts',(96.9349295810044,1.0813729462213,-6.73355220565791));
#29392=CARTESIAN_POINT('Ctrl Pts',(97.04341469029,1.02403134812153,-6.74121499626182));
#29393=CARTESIAN_POINT('Ctrl Pts',(97.0751534725957,1.00530061053149,-6.74353963409945));
#29394=CARTESIAN_POINT('Ctrl Pts',(97.1192229152418,0.976424846598278,-6.74693223892321));
#29395=CARTESIAN_POINT('Ctrl Pts',(97.1323076918178,0.967468475297618,-6.74796141245266));
#29396=CARTESIAN_POINT('Ctrl Pts',(97.1553987839183,0.950968542118187,-6.74982049522431));
#29397=CARTESIAN_POINT('Ctrl Pts',(97.1654731798984,0.943524191648493,-6.7506467494412));
#29398=CARTESIAN_POINT('Ctrl Pts',(97.1806557828157,0.931926269874227,-6.75191641833662));
#29399=CARTESIAN_POINT('Ctrl Pts',(97.1858512832153,0.927888053073119,-6.75235537794897));
#29400=CARTESIAN_POINT('Ctrl Pts',(97.1948513662871,0.920770929697331,-6.75312378748024));
#29401=CARTESIAN_POINT('Ctrl Pts',(97.198671139769,0.917711422934184,-6.7534524688929));
#29402=CARTESIAN_POINT('Ctrl Pts',(97.2072433927009,0.910757196069246,-6.75419595276506));
#29403=CARTESIAN_POINT('Ctrl Pts',(97.2119846543876,0.906848937717653,-6.75461128864135));
#29404=CARTESIAN_POINT('Ctrl Pts',(97.2247220388007,0.896180924856015,-6.75573843912593));
#29405=CARTESIAN_POINT('Ctrl Pts',(97.2326587947664,0.889351480380417,-6.75645304995754));
#29406=CARTESIAN_POINT('Ctrl Pts',(97.2709354598514,0.85551641057501,-6.75996094438057));
#29407=CARTESIAN_POINT('Ctrl Pts',(97.2999522443008,0.827062340072261,-6.76281362781111));
#29408=CARTESIAN_POINT('Ctrl Pts',(97.3837875392097,0.735887642268726,-6.77167497483926));
#29409=CARTESIAN_POINT('Ctrl Pts',(97.4334767086992,0.668806815210093,-6.77784611622798));
#29410=CARTESIAN_POINT('Ctrl Pts',(97.4897927612263,0.573051478831407,-6.78593488741303));
#29411=CARTESIAN_POINT('Ctrl Pts',(97.5030572716375,0.548548650099507,-6.78794584345695));
#29412=CARTESIAN_POINT('Ctrl Pts',(97.5202844854446,0.513838700140383,-6.79069376422158));
#29413=CARTESIAN_POINT('Ctrl Pts',(97.5249922963517,0.504013249753029,-6.79146072178625));
#29414=CARTESIAN_POINT('Ctrl Pts',(97.5329715401187,0.486749411169764,-6.79278769582341));
#29415=CARTESIAN_POINT('Ctrl Pts',(97.5363035368953,0.479339989808475,-6.79335069344924));
#29416=CARTESIAN_POINT('Ctrl Pts',(97.5411197535718,0.468326826836095,-6.79417729129723));
#29417=CARTESIAN_POINT('Ctrl Pts',(97.5426631004528,0.464749432334438,-6.79444421179172));
#29418=CARTESIAN_POINT('Ctrl Pts',(97.5452678423514,0.458628450132566,-6.79489814072942));
#29419=CARTESIAN_POINT('Ctrl Pts',(97.5463380932441,0.456088721791253,-6.79508567074725));
#29420=CARTESIAN_POINT('Ctrl Pts',(97.5487427527305,0.450325968673833,-6.79550932642587));
#29421=CARTESIAN_POINT('Ctrl Pts',(97.5500717656045,0.447100754514082,-6.79574512956077));
#29422=CARTESIAN_POINT('Ctrl Pts',(97.5536438077036,0.438321689429858,-6.79638358096444));
#29423=CARTESIAN_POINT('Ctrl Pts',(97.555858868204,0.432756463779058,-6.79678461795352));
#29424=CARTESIAN_POINT('Ctrl Pts',(97.5667090232984,0.404878875773957,-6.79877630092245));
#29425=CARTESIAN_POINT('Ctrl Pts',(97.5747059531034,0.382322224684695,-6.80033305317518));
#29426=CARTESIAN_POINT('Ctrl Pts',(97.5880346056005,0.34074505937641,-6.8031304835891));
#29427=CARTESIAN_POINT('Ctrl Pts',(97.5935855444375,0.32180504350194,-6.80437825465699));
#29428=CARTESIAN_POINT('Ctrl Pts',(97.6149555492005,0.241460998635152,-6.8095936509178));
#29429=CARTESIAN_POINT('Ctrl Pts',(97.6262788359309,0.178971290107049,-6.81346639847084));
#29430=CARTESIAN_POINT('Ctrl Pts',(97.6363068845378,0.0775388148548756,
-6.8198220078009));
#29431=CARTESIAN_POINT('Ctrl Pts',(97.6382135311509,0.0390449728083933,
-6.82224853635611));
#29432=CARTESIAN_POINT('Ctrl Pts',(97.6382415568925,-0.0233515149004739,
-6.82626240700895));
#29433=CARTESIAN_POINT('Ctrl Pts',(97.6375259693824,-0.047225378884949,
-6.82781704811608));
#29434=CARTESIAN_POINT('Ctrl Pts',(97.6355589528823,-0.0797674762297623,
-6.82996991716587));
#29435=CARTESIAN_POINT('Ctrl Pts',(97.6349358924056,-0.0884688906534224,
-6.83054885818288));
#29436=CARTESIAN_POINT('Ctrl Pts',(97.6337880983953,-0.102334403040144,
-6.83147697959983));
#29437=CARTESIAN_POINT('Ctrl Pts',(97.6333257819149,-0.107503457206415,
-6.83182422397345));
#29438=CARTESIAN_POINT('Ctrl Pts',(97.6323036044168,-0.118139442363736,
-6.83254136180633));
#29439=CARTESIAN_POINT('Ctrl Pts',(97.6317396131446,-0.123605839259553,
-6.83291137491555));
#29440=CARTESIAN_POINT('Ctrl Pts',(97.6303376454547,-0.136321790378976,
-6.83377554624475));
#29441=CARTESIAN_POINT('Ctrl Pts',(97.6294705098105,-0.143567835317118,
-6.83427059767699));
#29442=CARTESIAN_POINT('Ctrl Pts',(97.6264517634534,-0.166949402410066,
-6.83587674086363));
#29443=CARTESIAN_POINT('Ctrl Pts',(97.6240330375774,-0.183047901922865,
-6.83699605107244));
#29444=CARTESIAN_POINT('Ctrl Pts',(97.6175248743006,-0.220993873722818,
-6.83966763660328));
#29445=CARTESIAN_POINT('Ctrl Pts',(97.6131492148192,-0.242785288354996,
-6.84122821531472));
#29446=CARTESIAN_POINT('Ctrl Pts',(97.583305604925,-0.372308247967736,-6.85066255182494));
#29447=CARTESIAN_POINT('Ctrl Pts',(97.5433741580206,-0.476114472347658,
-6.85895734332145));
#29448=CARTESIAN_POINT('Ctrl Pts',(97.4779679255668,-0.593617984458168,
-6.86860234599094));
#29449=CARTESIAN_POINT('Ctrl Pts',(97.4657575551305,-0.614069369081318,
-6.87028837375453));
#29450=CARTESIAN_POINT('Ctrl Pts',(97.4497143378922,-0.639177701303956,
-6.87235509738748));
#29451=CARTESIAN_POINT('Ctrl Pts',(97.4464557519938,-0.644192923876767,
-6.87276774073831));
#29452=CARTESIAN_POINT('Ctrl Pts',(97.441237418681,-0.652091990600966,-6.873417123019));
#29453=CARTESIAN_POINT('Ctrl Pts',(97.4393028815496,-0.654992245893617,
-6.87365543678758));
#29454=CARTESIAN_POINT('Ctrl Pts',(97.435815738999,-0.660170212101329,-6.87408064063689));
#29455=CARTESIAN_POINT('Ctrl Pts',(97.4342680208881,-0.662451055070377,
-6.87426783858703));
#29456=CARTESIAN_POINT('Ctrl Pts',(97.4305115351465,-0.667945304155838,
-6.87471856099046));
#29457=CARTESIAN_POINT('Ctrl Pts',(97.4282947996807,-0.671153200783884,
-6.87498155102142));
#29458=CARTESIAN_POINT('Ctrl Pts',(97.421401291663,-0.68102380326286,-6.87579043316972));
#29459=CARTESIAN_POINT('Ctrl Pts',(97.4166712259537,-0.687649248432255,
-6.87633291141048));
#29460=CARTESIAN_POINT('Ctrl Pts',(97.389859097989,-0.72439356673599,-6.87934209876629));
#29461=CARTESIAN_POINT('Ctrl Pts',(97.3664206127203,-0.753500961981441,
-6.88172853690735));
#29462=CARTESIAN_POINT('Ctrl Pts',(97.2894128843905,-0.84033432027858,-6.88902722800703));
#29463=CARTESIAN_POINT('Ctrl Pts',(97.2314181341364,-0.893838065211288,
-6.89380392673516));
#29464=CARTESIAN_POINT('Ctrl Pts',(97.131849080621,-0.968744305876814,-6.90163532587682));
#29465=CARTESIAN_POINT('Ctrl Pts',(97.0936029867845,-0.994161175202824,
-6.90456739568809));
#29466=CARTESIAN_POINT('Ctrl Pts',(97.0447424233536,-1.02266702537903,-6.90828539177868));
#29467=CARTESIAN_POINT('Ctrl Pts',(97.0354372748858,-1.0279272961891,-6.90899216104235));
#29468=CARTESIAN_POINT('Ctrl Pts',(97.0205768317845,-1.03606311167467,-6.91011951414726));
#29469=CARTESIAN_POINT('Ctrl Pts',(97.0150678610423,-1.03902238846291,-6.91053714497291));
#29470=CARTESIAN_POINT('Ctrl Pts',(97.0047358233251,-1.04446691228128,-6.9113199951797));
#29471=CARTESIAN_POINT('Ctrl Pts',(96.9999186237999,-1.04696298520599,-6.91168482436119));
#29472=CARTESIAN_POINT('Ctrl Pts',(96.9891288141714,-1.05245958198956,-6.91250170902271));
#29473=CARTESIAN_POINT('Ctrl Pts',(96.983147600216,-1.05544270597129,-6.91295435191427));
#29474=CARTESIAN_POINT('Ctrl Pts',(96.9654278318999,-1.06409285969387,-6.91429497601245));
#29475=CARTESIAN_POINT('Ctrl Pts',(96.9536205458373,-1.06961595115866,-6.91518782593623));
#29476=CARTESIAN_POINT('Ctrl Pts',(96.9265004072677,-1.08175743667071,-6.91723835317986));
#29477=CARTESIAN_POINT('Ctrl Pts',(96.9111340115599,-1.08824861882579,-6.91840002367127));
#29478=CARTESIAN_POINT('Ctrl Pts',(96.8586552625048,-1.10911497610921,-6.92236761226475));
#29479=CARTESIAN_POINT('Ctrl Pts',(96.8209569187169,-1.12193375296381,-6.92521935593456));
#29480=CARTESIAN_POINT('Ctrl Pts',(96.6996653053471,-1.15643236359103,-6.934373677303));
#29481=CARTESIAN_POINT('Ctrl Pts',(96.6143037399726,-1.17084730419555,-6.94080517792564));
#29482=CARTESIAN_POINT('Ctrl Pts',(96.5086020925552,-1.17692913051396,-6.94835612972556));
#29483=CARTESIAN_POINT('Ctrl Pts',(96.4890437388933,-1.1775661759021,-6.94973497666021));
#29484=CARTESIAN_POINT('Ctrl Pts',(96.4638165574998,-1.17775888098992,-6.95148258865477));
#29485=CARTESIAN_POINT('Ctrl Pts',(96.4581554637986,-1.17776131001634,-6.95187275376299));
#29486=CARTESIAN_POINT('Ctrl Pts',(96.4491132359276,-1.177699991763,-6.95249251379603));
#29487=CARTESIAN_POINT('Ctrl Pts',(96.4457321001787,-1.17766250160362,-6.95272349189297));
#29488=CARTESIAN_POINT('Ctrl Pts',(96.4392567417308,-1.17756281061463,-6.95316431953868));
#29489=CARTESIAN_POINT('Ctrl Pts',(96.4361625658402,-1.17750297509937,-6.95337428823693));
#29490=CARTESIAN_POINT('Ctrl Pts',(96.4287800408916,-1.17733109906063,-6.95387371125276));
#29491=CARTESIAN_POINT('Ctrl Pts',(96.4244919502068,-1.17720782268296,-6.95416255302269));
#29492=CARTESIAN_POINT('Ctrl Pts',(96.4098881010507,-1.17670811156251,-6.95514230554123));
#29493=CARTESIAN_POINT('Ctrl Pts',(96.3995763092994,-1.17621947730991,-6.95582739638931));
#29494=CARTESIAN_POINT('Ctrl Pts',(96.3743905260724,-1.17469390385401,-6.95748717316768));
#29495=CARTESIAN_POINT('Ctrl Pts',(96.3595269261624,-1.17350997325286,-6.95845517505391));
#29496=CARTESIAN_POINT('Ctrl Pts',(96.2988995579458,-1.16752030555357,-6.96237090055341));
#29497=CARTESIAN_POINT('Ctrl Pts',(96.2534107677746,-1.16031668294897,-6.96523362639875));
#29498=CARTESIAN_POINT('Ctrl Pts',(96.1194400056407,-1.13096881069579,-6.97372832373236));
#29499=CARTESIAN_POINT('Ctrl Pts',(96.0329974962076,-1.10120622183265,-6.97931971926822));
#29500=CARTESIAN_POINT('Ctrl Pts',(95.9376018579259,-1.05541867101454,-6.98622221068482));
#29501=CARTESIAN_POINT('Ctrl Pts',(95.9244712063652,-1.04881106005287,-6.98718874841855));
#29502=CARTESIAN_POINT('Ctrl Pts',(95.905243918589,-1.03868012300822,-6.98863036919659));
#29503=CARTESIAN_POINT('Ctrl Pts',(95.8990493543302,-1.03534492744148,-6.98909893745356));
#29504=CARTESIAN_POINT('Ctrl Pts',(95.8880880824478,-1.02931600670457,-6.98993560726436));
#29505=CARTESIAN_POINT('Ctrl Pts',(95.8833095377571,-1.02664414265652,-6.99030293174996));
#29506=CARTESIAN_POINT('Ctrl Pts',(95.8733578288444,-1.02098832895136,-6.99107342155238));
#29507=CARTESIAN_POINT('Ctrl Pts',(95.8681883969793,-1.0179981614062,-6.99147680020582));
#29508=CARTESIAN_POINT('Ctrl Pts',(95.8547007603713,-1.01005896281564,-6.99253767135532));
#29509=CARTESIAN_POINT('Ctrl Pts',(95.8464205764423,-1.00504656332294,-6.99319742075052));
#29510=CARTESIAN_POINT('Ctrl Pts',(95.8081570389825,-0.981234419937012,
-6.99628667569865));
#29511=CARTESIAN_POINT('Ctrl Pts',(95.7789718237791,-0.961193180207256,
-6.99876091674393));
#29512=CARTESIAN_POINT('Ctrl Pts',(95.7014389129711,-0.90264400448064,-7.00567105559041));
#29513=CARTESIAN_POINT('Ctrl Pts',(95.6551523152623,-0.861600454694597,
-7.0101881889309));
#29514=CARTESIAN_POINT('Ctrl Pts',(95.5680027667561,-0.771138540234212,
-7.0194071278191));
#29515=CARTESIAN_POINT('Ctrl Pts',(95.5275117015609,-0.721624500413595,
-7.02409439104554));
#29516=CARTESIAN_POINT('Ctrl Pts',(95.4855573550991,-0.660847048678829,
-7.02927284511133));
#29517=CARTESIAN_POINT('Ctrl Pts',(95.4799874441898,-0.652554472178123,
-7.02996779402803));
#29518=CARTESIAN_POINT('Ctrl Pts',(95.4723718619117,-0.640898562664305,
-7.03092748358191));
#29519=CARTESIAN_POINT('Ctrl Pts',(95.4702367091495,-0.637594606440704,
-7.03119762595653));
#29520=CARTESIAN_POINT('Ctrl Pts',(95.4665800815491,-0.631873628964075,
-7.0316620587793));
#29521=CARTESIAN_POINT('Ctrl Pts',(95.4650507871649,-0.629461683227001,
-7.03185684763986));
#29522=CARTESIAN_POINT('Ctrl Pts',(95.4618407354994,-0.624357954664768,
-7.03226684868743));
#29523=CARTESIAN_POINT('Ctrl Pts',(95.4601620561173,-0.621664897318871,
-7.03248191930135));
#29524=CARTESIAN_POINT('Ctrl Pts',(95.4560197870403,-0.614959351634867,
-7.03301436434572));
#29525=CARTESIAN_POINT('Ctrl Pts',(95.4535693019478,-0.610938758757568,
-7.03333090265751));
#29526=CARTESIAN_POINT('Ctrl Pts',(95.4443936450504,-0.595678772052536,
-7.03452252106524));
#29527=CARTESIAN_POINT('Ctrl Pts',(95.4378317123981,-0.584341666096217,
-7.03538785524774));
#29528=CARTESIAN_POINT('Ctrl Pts',(95.4214407765628,-0.554900735563526,
-7.03759042591352));
#29529=CARTESIAN_POINT('Ctrl Pts',(95.4118948154764,-0.536643762463493,
-7.03891385874727));
#29530=CARTESIAN_POINT('Ctrl Pts',(95.3774462232762,-0.466326513788181,
-7.04388728208573));
#29531=CARTESIAN_POINT('Ctrl Pts',(95.3559013267196,-0.412709686764973,
-7.04743038984246));
#29532=CARTESIAN_POINT('Ctrl Pts',(95.3154698778587,-0.285885369046476,
-7.05567274513202));
#29533=CARTESIAN_POINT('Ctrl Pts',(95.2995219671884,-0.21202083607617,-7.06038223187065));
#29534=CARTESIAN_POINT('Ctrl Pts',(95.2895334610219,-0.126826518984517,
-7.06601187704241));
#29535=CARTESIAN_POINT('Ctrl Pts',(95.2884603447734,-0.116493251282683,
-7.06669766382515));
#29536=CARTESIAN_POINT('Ctrl Pts',(95.2869179760793,-0.0994496693158102,
-7.06783432644692));
#29537=CARTESIAN_POINT('Ctrl Pts',(95.2863692502246,-0.0927469880201546,
-7.06828274301734));
#29538=CARTESIAN_POINT('Ctrl Pts',(95.2854814066951,-0.0806263165939802,
-7.06909633092116));
#29539=CARTESIAN_POINT('Ctrl Pts',(95.2851222846926,-0.0752099454617208,
-7.06946087270627));
#29540=CARTESIAN_POINT('Ctrl Pts',(95.2844318644319,-0.063579372613031,
-7.07024583139685));
#29541=CARTESIAN_POINT('Ctrl Pts',(95.2841123508418,-0.0573646636602585,
-7.0706666015377));
#29542=CARTESIAN_POINT('Ctrl Pts',(95.2833716588476,-0.0403252856444004,
-7.07182406284828));
#29543=CARTESIAN_POINT('Ctrl Pts',(95.2830505617619,-0.0294971056563918,
-7.07256381269156));
#29544=CARTESIAN_POINT('Ctrl Pts',(95.2820333170437,0.0346777292341549,
-7.07697423523189));
#29545=CARTESIAN_POINT('Ctrl Pts',(95.284813404224,0.0880097582886529,-7.08075089277713));
#29546=CARTESIAN_POINT('Ctrl Pts',(95.2969371898862,0.188575961179659,-7.08807211695678));
#29547=CARTESIAN_POINT('Ctrl Pts',(95.3055796823814,0.235791440587897,-7.09159417919729));
#29548=CARTESIAN_POINT('Ctrl Pts',(95.3238379460088,0.309731218146189,-7.09718199086497));
#29549=CARTESIAN_POINT('Ctrl Pts',(95.3315821718537,0.33686553528854,-7.09924791973965));
#29550=CARTESIAN_POINT('Ctrl Pts',(95.3509929565848,0.396650905548326,-7.10380531659571));
#29551=CARTESIAN_POINT('Ctrl Pts',(95.3631426573753,0.429120863504874,-7.10628431940859));
#29552=CARTESIAN_POINT('Ctrl Pts',(95.379081138831,0.466590047760546,-7.10911446708953));
#29553=CARTESIAN_POINT('Ctrl Pts',(95.3814975393095,0.472151064371352,-7.10953368278558));
#29554=CARTESIAN_POINT('Ctrl Pts',(95.3855085750354,0.481190287892778,-7.11021347052416));
#29555=CARTESIAN_POINT('Ctrl Pts',(95.3870773675656,0.484679739987771,-7.11047549234275));
#29556=CARTESIAN_POINT('Ctrl Pts',(95.389924052472,0.490929981392766,-7.11094402181338));
#29557=CARTESIAN_POINT('Ctrl Pts',(95.3911956586952,0.493693512123373,-7.11115089321832));
#29558=CARTESIAN_POINT('Ctrl Pts',(95.3940214942159,0.499772648695421,-7.11160532652717));
#29559=CARTESIAN_POINT('Ctrl Pts',(95.3955804853054,0.503085949335144,-7.11185259679593));
#29560=CARTESIAN_POINT('Ctrl Pts',(95.400146981531,0.51267471541555,-7.11256716902181));
#29561=CARTESIAN_POINT('Ctrl Pts',(95.4031947464796,0.518930995542927,-7.11303210874049));
#29562=CARTESIAN_POINT('Ctrl Pts',(95.4295789089374,0.571893394205202,-7.11696014137991));
#29563=CARTESIAN_POINT('Ctrl Pts',(95.4559451144396,0.617033462149801,-7.12025664880505));
#29564=CARTESIAN_POINT('Ctrl Pts',(95.5318781515408,0.729189328667322,-7.12869343626242));
#29565=CARTESIAN_POINT('Ctrl Pts',(95.585701710694,0.792957202164231,-7.13375744393606));
#29566=CARTESIAN_POINT('Ctrl Pts',(95.6680247354002,0.871811718591976,-7.1410286297561));
#29567=CARTESIAN_POINT('Ctrl Pts',(95.6910777997151,0.892222540414428,-7.14301999628774));
#29568=CARTESIAN_POINT('Ctrl Pts',(95.7223100699347,0.917763797904444,-7.14567895538587));
#29569=CARTESIAN_POINT('Ctrl Pts',(95.7297912070994,0.923731090551799,-7.14631304261169));
#29570=CARTESIAN_POINT('Ctrl Pts',(95.7420389099312,0.933258526762123,-7.14734708613484));
#29571=CARTESIAN_POINT('Ctrl Pts',(95.7467612931565,0.936874960679396,-7.14774482871979));
#29572=CARTESIAN_POINT('Ctrl Pts',(95.755888378535,0.943755490090837,-7.14851184547839));
#29573=CARTESIAN_POINT('Ctrl Pts',(95.7602888849372,0.947024913672375,-7.1488809002435));
#29574=CARTESIAN_POINT('Ctrl Pts',(95.7705273187116,0.954521344673939,-7.14973792370096));
#29575=CARTESIAN_POINT('Ctrl Pts',(95.7763814920068,0.958725684613716,-7.15022674013802));
#29576=CARTESIAN_POINT('Ctrl Pts',(95.7951695847861,0.971959185091832,-7.15179192094793));
#29577=CARTESIAN_POINT('Ctrl Pts',(95.8082459979776,0.980782032735578,-7.1528759287993));
#29578=CARTESIAN_POINT('Ctrl Pts',(95.8394105242881,1.00091030577544,-7.15544822591452));
#29579=CARTESIAN_POINT('Ctrl Pts',(95.8576358909193,1.01199192230355,-7.15694400981839));
#29580=CARTESIAN_POINT('Ctrl Pts',(95.891188954041,1.03116519760778,-7.15968278018666));
#29581=CARTESIAN_POINT('Ctrl Pts',(95.9064096505938,1.03942274704365,-7.16091977633442));
#29582=CARTESIAN_POINT('Ctrl Pts',(95.921801726504,1.04733937056209,-7.16216478479583));
#29583=CARTESIAN_POINT('Origin',(96.460480949577,-7.19464945638997E-16,
0.924367114736168));
#29584=CARTESIAN_POINT('',(95.9218015552897,1.04733928250124,-7.7622548478038));
#29585=CARTESIAN_POINT('',(95.9218016730721,1.04733934308043,-7.66392541087522));
#29586=CARTESIAN_POINT('',(95.9218016730721,1.04733934308042,0.924367114736168));
#29587=CARTESIAN_POINT('Ctrl Pts',(95.9218015552896,1.04733928250123,-7.76225484780379));
#29588=CARTESIAN_POINT('Ctrl Pts',(95.8623558116904,1.01676447480516,-7.75745389936112));
#29589=CARTESIAN_POINT('Ctrl Pts',(95.8056001884861,0.98117324913246,-7.75252362611853));
#29590=CARTESIAN_POINT('Ctrl Pts',(95.7104284735965,0.909529753051495,-7.74380334359668));
#29591=CARTESIAN_POINT('Ctrl Pts',(95.6708304283255,0.87537217593098,-7.74001378553606));
#29592=CARTESIAN_POINT('Ctrl Pts',(95.6286713472776,0.833808301570045,-7.7358960785663));
#29593=CARTESIAN_POINT('Ctrl Pts',(95.6237585763514,0.828878262619539,-7.7354149034486));
#29594=CARTESIAN_POINT('Ctrl Pts',(95.6163278537723,0.821288027268597,-7.7346854488181));
#29595=CARTESIAN_POINT('Ctrl Pts',(95.6137782317822,0.818659258475165,-7.73443485500648));
#29596=CARTESIAN_POINT('Ctrl Pts',(95.6091329451359,0.813824854424591,-7.73397779754325));
#29597=CARTESIAN_POINT('Ctrl Pts',(95.6070335569774,0.811622983199139,-7.73377105779751));
#29598=CARTESIAN_POINT('Ctrl Pts',(95.6023131234428,0.806633549989927,-7.73330578623913));
#29599=CARTESIAN_POINT('Ctrl Pts',(95.5996971140449,0.803841334655844,-7.73304763261966));
#29600=CARTESIAN_POINT('Ctrl Pts',(95.5929705930079,0.796591244776481,-7.73238289354525));
#29601=CARTESIAN_POINT('Ctrl Pts',(95.5888807564069,0.792114219726847,-7.73197779223504));
#29602=CARTESIAN_POINT('Ctrl Pts',(95.5616517694671,0.761841192206451,-7.72927282621328));
#29603=CARTESIAN_POINT('Ctrl Pts',(95.5396238510393,0.735063675310923,-7.72704554617816));
#29604=CARTESIAN_POINT('Ctrl Pts',(95.5018766974373,0.68481207866792,-7.72307426380063));
#29605=CARTESIAN_POINT('Ctrl Pts',(95.4857603702686,0.661671828179948,-7.7213189995572));
#29606=CARTESIAN_POINT('Ctrl Pts',(95.4445239084751,0.597682230029865,-7.71659903347338));
#29607=CARTESIAN_POINT('Ctrl Pts',(95.4210429206934,0.555842828153083,-7.7136512878776));
#29608=CARTESIAN_POINT('Ctrl Pts',(95.3769402612776,0.464633175988972,-7.70731590496983));
#29609=CARTESIAN_POINT('Ctrl Pts',(95.357000226675,0.415058573191055,-7.70392275662391));
#29610=CARTESIAN_POINT('Ctrl Pts',(95.3371404041336,0.354003493066166,-7.69970304477885));
#29611=CARTESIAN_POINT('Ctrl Pts',(95.3339313870623,0.343654658855028,-7.69898659985602));
#29612=CARTESIAN_POINT('Ctrl Pts',(95.3291045948915,0.327293967159561,-7.69785137481006));
#29613=CARTESIAN_POINT('Ctrl Pts',(95.3273908735627,0.32131086818038,-7.69743568607001));
#29614=CARTESIAN_POINT('Ctrl Pts',(95.3242712661299,0.31008400299646,-7.69665453956417));
#29615=CARTESIAN_POINT('Ctrl Pts',(95.3228540544881,0.304843532904559,-7.69628945600205));
#29616=CARTESIAN_POINT('Ctrl Pts',(95.3197623509039,0.293089358644882,-7.69546946736407));
#29617=CARTESIAN_POINT('Ctrl Pts',(95.3181073326422,0.286570775895503,-7.69501395445715));
#29618=CARTESIAN_POINT('Ctrl Pts',(95.3140381142473,0.269947794253929,-7.69385024094827));
#29619=CARTESIAN_POINT('Ctrl Pts',(95.311701655163,0.259825147057946,-7.69313960999478));
#29620=CARTESIAN_POINT('Ctrl Pts',(95.293502274304,0.175926871196835,-7.6872319712601));
#29621=CARTESIAN_POINT('Ctrl Pts',(95.284632574587,0.100827628796701,-7.68181333533136));
#29622=CARTESIAN_POINT('Ctrl Pts',(95.2817578858941,-0.0323856236665279,
-7.67206625033741));
#29623=CARTESIAN_POINT('Ctrl Pts',(95.2847675297353,-0.0901947604395963,
-7.66779664176533));
#29624=CARTESIAN_POINT('Ctrl Pts',(95.2945782898097,-0.167887660780126,
-7.66214169867262));
#29625=CARTESIAN_POINT('Ctrl Pts',(95.2976771504118,-0.18815606035501,-7.66067478824316));
#29626=CARTESIAN_POINT('Ctrl Pts',(95.3036126679399,-0.221181417611749,
-7.65830834490023));
#29627=CARTESIAN_POINT('Ctrl Pts',(95.3061351554409,-0.233989879058172,
-7.65739647204719));
#29628=CARTESIAN_POINT('Ctrl Pts',(95.3098554244798,-0.251352494807781,
-7.65617078305995));
#29629=CARTESIAN_POINT('Ctrl Pts',(95.3108682041788,-0.255944746293492,
-7.65584759672723));
#29630=CARTESIAN_POINT('Ctrl Pts',(95.3126102332335,-0.263624628277087,
-7.65530892385985));
#29631=CARTESIAN_POINT('Ctrl Pts',(95.3133244929625,-0.266715561787505,
-7.65509261604539));
#29632=CARTESIAN_POINT('Ctrl Pts',(95.3147058025516,-0.272584920650193,
-7.65468285522255));
#29633=CARTESIAN_POINT('Ctrl Pts',(95.3153704858758,-0.275363855420494,
-7.65448926651578));
#29634=CARTESIAN_POINT('Ctrl Pts',(95.3169754459565,-0.281967619849792,
-7.65403016537959));
#29635=CARTESIAN_POINT('Ctrl Pts',(95.3179248164491,-0.285790236380545,
-7.65376516146224));
#29636=CARTESIAN_POINT('Ctrl Pts',(95.3213565728594,-0.299317657425676,
-7.65282979058452));
#29637=CARTESIAN_POINT('Ctrl Pts',(95.3239436580247,-0.308995804033067,
-7.65216500767871));
#29638=CARTESIAN_POINT('Ctrl Pts',(95.3440546483653,-0.380557351833379,
-7.64727437673847));
#29639=CARTESIAN_POINT('Ctrl Pts',(95.3665003643921,-0.44095381115291,-7.64328185087216));
#29640=CARTESIAN_POINT('Ctrl Pts',(95.4197954966609,-0.55483219002027,-7.63549953789965));
#29641=CARTESIAN_POINT('Ctrl Pts',(95.4501286307923,-0.608319489865074,
-7.63171932980393));
#29642=CARTESIAN_POINT('Ctrl Pts',(95.5042328763501,-0.688424765656717,
-7.625580045225));
#29643=CARTESIAN_POINT('Ctrl Pts',(95.5252750434112,-0.716748613827844,
-7.62330529138456));
#29644=CARTESIAN_POINT('Ctrl Pts',(95.553663635546,-0.751578949035402,-7.62034464378981));
#29645=CARTESIAN_POINT('Ctrl Pts',(95.5598644549051,-0.758998338619742,
-7.61970404976792));
#29646=CARTESIAN_POINT('Ctrl Pts',(95.5700404585016,-0.77087381413286,-7.61866199740248));
#29647=CARTESIAN_POINT('Ctrl Pts',(95.5739594936044,-0.775377592752606,
-7.61826281759666));
#29648=CARTESIAN_POINT('Ctrl Pts',(95.5815384749185,-0.783954829693693,
-7.61749479895331));
#29649=CARTESIAN_POINT('Ctrl Pts',(95.585192929818,-0.78803294949385,-7.61712619253361));
#29650=CARTESIAN_POINT('Ctrl Pts',(95.5936108264012,-0.797295945090009,
-7.61628092628429));
#29651=CARTESIAN_POINT('Ctrl Pts',(95.5983925512732,-0.802463846099366,
-7.6158035089931));
#29652=CARTESIAN_POINT('Ctrl Pts',(95.6133168484535,-0.818306090214565,
-7.61432156713335));
#29653=CARTESIAN_POINT('Ctrl Pts',(95.6236131450621,-0.828832983937494,
-7.61331054777798));
#29654=CARTESIAN_POINT('Ctrl Pts',(95.698816421333,-0.902890379633603,-7.60600292835653));
#29655=CARTESIAN_POINT('Ctrl Pts',(95.7706717911202,-0.958906205808967,
-7.5993852895564));
#29656=CARTESIAN_POINT('Ctrl Pts',(95.8877120106867,-1.03012958227682,-7.58933030368828));
#29657=CARTESIAN_POINT('Ctrl Pts',(95.9285770109048,-1.05181267972917,-7.58594205587981));
#29658=CARTESIAN_POINT('Ctrl Pts',(95.9842059676899,-1.07725606654963,-7.58156511302202));
#29659=CARTESIAN_POINT('Ctrl Pts',(95.9979169860043,-1.08321425176453,-7.58050457575498));
#29660=CARTESIAN_POINT('Ctrl Pts',(96.0213010971731,-1.09285090271834,-7.57873062670749));
#29661=CARTESIAN_POINT('Ctrl Pts',(96.0309157350125,-1.0966657572051,-7.57801101814121));
#29662=CARTESIAN_POINT('Ctrl Pts',(96.0445909927128,-1.10188431295254,-7.57700246069502));
#29663=CARTESIAN_POINT('Ctrl Pts',(96.0486106222244,-1.10339309869505,-7.57670782434119));
#29664=CARTESIAN_POINT('Ctrl Pts',(96.0555424544591,-1.10595183426817,-7.57620294810431));
#29665=CARTESIAN_POINT('Ctrl Pts',(96.0584506853503,-1.10701233602849,-7.57599210192367));
#29666=CARTESIAN_POINT('Ctrl Pts',(96.064543367787,-1.10920688772061,-7.57555245416719));
#29667=CARTESIAN_POINT('Ctrl Pts',(96.0677285515537,-1.11033870643756,-7.57532378126615));
#29668=CARTESIAN_POINT('Ctrl Pts',(96.076255595299,-1.11332741011944,-7.57471461227414));
#29669=CARTESIAN_POINT('Ctrl Pts',(96.0816061128963,-1.11515958781862,-7.574335520574));
#29670=CARTESIAN_POINT('Ctrl Pts',(96.1054700193082,-1.12313972185915,-7.57265782571121));
#29671=CARTESIAN_POINT('Ctrl Pts',(96.1241224446603,-1.12886609399666,-7.57138143487332));
#29672=CARTESIAN_POINT('Ctrl Pts',(96.2252861281093,-1.15719332151939,-7.56460230885184));
#29673=CARTESIAN_POINT('Ctrl Pts',(96.3099381244624,-1.17121853105755,-7.55942288639653));
#29674=CARTESIAN_POINT('Ctrl Pts',(96.4505528376814,-1.17900424556005,-7.55065428444415));
#29675=CARTESIAN_POINT('Ctrl Pts',(96.5058763561995,-1.17817136094729,-7.5471660186304));
#29676=CARTESIAN_POINT('Ctrl Pts',(96.5752032635571,-1.17223674596182,-7.54262278544775));
#29677=CARTESIAN_POINT('Ctrl Pts',(96.5894496208711,-1.17075499180739,-7.54168023680153));
#29678=CARTESIAN_POINT('Ctrl Pts',(96.610551054602,-1.16817043113566,-7.54026924194545));
#29679=CARTESIAN_POINT('Ctrl Pts',(96.6174294667427,-1.16726618734159,-7.53980694331343));
#29680=CARTESIAN_POINT('Ctrl Pts',(96.6296945976675,-1.16554342973198,-7.53897820654938));
#29681=CARTESIAN_POINT('Ctrl Pts',(96.6350844258278,-1.16474820011479,-7.5386125034827));
#29682=CARTESIAN_POINT('Ctrl Pts',(96.6464831928538,-1.16298549864059,-7.53783577770189));
#29683=CARTESIAN_POINT('Ctrl Pts',(96.6524905198881,-1.16200878958067,-7.53742447621294));
#29684=CARTESIAN_POINT('Ctrl Pts',(96.6685460471911,-1.15927047969631,-7.53631983284869));
#29685=CARTESIAN_POINT('Ctrl Pts',(96.6785791909015,-1.15742484668191,-7.53562388348187));
#29686=CARTESIAN_POINT('Ctrl Pts',(96.7249969849779,-1.14826116216898,-7.53237696637806));
#29687=CARTESIAN_POINT('Ctrl Pts',(96.7610432099318,-1.13935694086453,-7.52977691457013));
#29688=CARTESIAN_POINT('Ctrl Pts',(96.879467093729,-1.10409260668574,-7.52096718048058));
#29689=CARTESIAN_POINT('Ctrl Pts',(96.9593542506177,-1.07037018027013,-7.514559087871));
#29690=CARTESIAN_POINT('Ctrl Pts',(97.0596107332953,-1.01436923821392,-7.50619341250719));
#29691=CARTESIAN_POINT('Ctrl Pts',(97.083895044422,-0.999628196070767,-7.50414192887341));
#29692=CARTESIAN_POINT('Ctrl Pts',(97.1213250061091,-0.975012356557827,
-7.5009639365712));
#29693=CARTESIAN_POINT('Ctrl Pts',(97.1348370543568,-0.965716249038768,
-7.49981329221704));
#29694=CARTESIAN_POINT('Ctrl Pts',(97.152306662886,-0.953151846782232,-7.49832550858258));
#29695=CARTESIAN_POINT('Ctrl Pts',(97.1564425446897,-0.950136159273038,
-7.49797327203306));
#29696=CARTESIAN_POINT('Ctrl Pts',(97.1631815834963,-0.945154759713182,
-7.49739949555798));
#29697=CARTESIAN_POINT('Ctrl Pts',(97.1657964137941,-0.943205066416705,
-7.49717690324461));
#29698=CARTESIAN_POINT('Ctrl Pts',(97.1708984402366,-0.93936776615128,-7.49674271662857));
#29699=CARTESIAN_POINT('Ctrl Pts',(97.1733862777433,-0.937481095572839,
-7.4965310656016));
#29700=CARTESIAN_POINT('Ctrl Pts',(97.1789410007957,-0.933233730354478,
-7.49605857756015));
#29701=CARTESIAN_POINT('Ctrl Pts',(97.1820038409129,-0.930867745169545,
-7.49579810251875));
#29702=CARTESIAN_POINT('Ctrl Pts',(97.192631930154,-0.922573778070909,-7.49489421371316));
#29703=CARTESIAN_POINT('Ctrl Pts',(97.200136480555,-0.916568134041856,-7.49425590606996));
#29704=CARTESIAN_POINT('Ctrl Pts',(97.2651823877418,-0.863194787566515,
-7.48871434044085));
#29705=CARTESIAN_POINT('Ctrl Pts',(97.3181887822631,-0.810549255170093,
-7.48412905434578));
#29706=CARTESIAN_POINT('Ctrl Pts',(97.4176337646367,-0.691017228400199,
-7.47451097721846));
#29707=CARTESIAN_POINT('Ctrl Pts',(97.4628407987864,-0.623633540421259,
-7.46949080904351));
#29708=CARTESIAN_POINT('Ctrl Pts',(97.5069490201436,-0.540530077820964,
-7.46333495666381));
#29709=CARTESIAN_POINT('Ctrl Pts',(97.5129222043343,-0.528805796551455,
-7.46246777314942));
#29710=CARTESIAN_POINT('Ctrl Pts',(97.5216424792608,-0.51095624115618,-7.46114820672977));
#29711=CARTESIAN_POINT('Ctrl Pts',(97.5245358199176,-0.504903260273835,
-7.4607008449404));
#29712=CARTESIAN_POINT('Ctrl Pts',(97.5296760441138,-0.493909274013369,
-7.45988835217087));
#29713=CARTESIAN_POINT('Ctrl Pts',(97.5319408014373,-0.488976794239848,
-7.4595238425127));
#29714=CARTESIAN_POINT('Ctrl Pts',(97.5367340954343,-0.478344136362578,
-7.45873803717769));
#29715=CARTESIAN_POINT('Ctrl Pts',(97.5392516068777,-0.472639199734736,
-7.45831638172234));
#29716=CARTESIAN_POINT('Ctrl Pts',(97.5459296304045,-0.457174779250553,
-7.45717316120706));
#29717=CARTESIAN_POINT('Ctrl Pts',(97.5500036851413,-0.447378825397032,
-7.45644873094879));
#29718=CARTESIAN_POINT('Ctrl Pts',(97.5704997607619,-0.396155492114108,
-7.45265828528396));
#29719=CARTESIAN_POINT('Ctrl Pts',(97.5846911894789,-0.353880478620545,
-7.44951994158513));
#29720=CARTESIAN_POINT('Ctrl Pts',(97.6159489981286,-0.239672984383178,
-7.44101802352181));
#29721=CARTESIAN_POINT('Ctrl Pts',(97.628700611264,-0.166765739178536,-7.43555749908482));
#29722=CARTESIAN_POINT('Ctrl Pts',(97.6370103902116,-0.0620330255118681,
-7.42788722945364));
#29723=CARTESIAN_POINT('Ctrl Pts',(97.6382414144787,-0.0308248451714677,
-7.4256255119171));
#29724=CARTESIAN_POINT('Ctrl Pts',(97.6382250963924,0.0175510471689629,
-7.42218790599012));
#29725=CARTESIAN_POINT('Ctrl Pts',(97.637844546256,0.0347037554939205,-7.42098240564126));
#29726=CARTESIAN_POINT('Ctrl Pts',(97.6368518540831,0.0572334709682163,
-7.41942162953615));
#29727=CARTESIAN_POINT('Ctrl Pts',(97.6365773004606,0.0626222916618255,
-7.41905001739357));
#29728=CARTESIAN_POINT('Ctrl Pts',(97.6360738433497,0.071326371668827,-7.41845274298954));
#29729=CARTESIAN_POINT('Ctrl Pts',(97.6358679307473,0.0746428052391939,
-7.41822586351453));
#29730=CARTESIAN_POINT('Ctrl Pts',(97.6354413540386,0.0810731456158617,
-7.41778736350986));
#29731=CARTESIAN_POINT('Ctrl Pts',(97.6352223426724,0.0841870927961977,
-7.41757566117703));
#29732=CARTESIAN_POINT('Ctrl Pts',(97.6346616197167,0.0917308899732993,
-7.41706428573184));
#29733=CARTESIAN_POINT('Ctrl Pts',(97.634307212413,0.0961598074494911,-7.41676530517044));
#29734=CARTESIAN_POINT('Ctrl Pts',(97.6329645891463,0.111822881555163,-7.41571201637014));
#29735=CARTESIAN_POINT('Ctrl Pts',(97.6318400550919,0.123045157626982,-7.41496476956478));
#29736=CARTESIAN_POINT('Ctrl Pts',(97.6286412735856,0.150924547474556,-7.4131229993358));
#29737=CARTESIAN_POINT('Ctrl Pts',(97.6263717794734,0.167557135799995,-7.41203723029747));
#29738=CARTESIAN_POINT('Ctrl Pts',(97.6148547453488,0.240315055069447,-7.40732273760123));
#29739=CARTESIAN_POINT('Ctrl Pts',(97.601903446648,0.29578006646135,-7.40381818630191));
#29740=CARTESIAN_POINT('Ctrl Pts',(97.5623822618168,0.422722802698419,-7.39559371656221));
#29741=CARTESIAN_POINT('Ctrl Pts',(97.5327915116385,0.492979955074924,-7.3908732136551));
#29742=CARTESIAN_POINT('Ctrl Pts',(97.4892561064338,0.57354839906996,-7.38490577819364));
#29743=CARTESIAN_POINT('Ctrl Pts',(97.4816066152015,0.587059134952063,-7.38388558091821));
#29744=CARTESIAN_POINT('Ctrl Pts',(97.4700803449232,0.60650995837164,-7.38238606427812));
#29745=CARTESIAN_POINT('Ctrl Pts',(97.4664132370991,0.612572851128108,-7.38191420993432));
#29746=CARTESIAN_POINT('Ctrl Pts',(97.4598120728653,0.623267540035415,-7.381073749374));
#29747=CARTESIAN_POINT('Ctrl Pts',(97.4568999359014,0.62791267099355,-7.38070594478892));
#29748=CARTESIAN_POINT('Ctrl Pts',(97.4507605105384,0.637555364912286,-7.37993656028917));
#29749=CARTESIAN_POINT('Ctrl Pts',(97.4475275839824,0.642549135441851,-7.37953478112472));
#29750=CARTESIAN_POINT('Ctrl Pts',(97.4389945306226,0.655513426905098,-7.37848287006844));
#29751=CARTESIAN_POINT('Ctrl Pts',(97.4336349135633,0.663444070094435,-7.37783055100202));
#29752=CARTESIAN_POINT('Ctrl Pts',(97.4087065304904,0.699378612347029,-7.374833415328));
#29753=CARTESIAN_POINT('Ctrl Pts',(97.3880234667278,0.726585621774624,-7.37244707601841));
#29754=CARTESIAN_POINT('Ctrl Pts',(97.3238210633379,0.803823310700079,-7.36531297918666));
#29755=CARTESIAN_POINT('Ctrl Pts',(97.2772302581138,0.851120930213523,-7.36046011495299));
#29756=CARTESIAN_POINT('Ctrl Pts',(97.1807822938679,0.933784072745702,-7.35113798834233));
#29757=CARTESIAN_POINT('Ctrl Pts',(97.1316537720359,0.969698527499502,-7.3466863313735));
#29758=CARTESIAN_POINT('Ctrl Pts',(97.071458208579,1.0069269986169,-7.34172323075003));
#29759=CARTESIAN_POINT('Ctrl Pts',(97.0628807414419,1.01208186371204,-7.34102702647592));
#29760=CARTESIAN_POINT('Ctrl Pts',(97.0508383092989,1.01911174525446,-7.3400658826868));
#29761=CARTESIAN_POINT('Ctrl Pts',(97.0474283576277,1.02107947917315,-7.33979552101594));
#29762=CARTESIAN_POINT('Ctrl Pts',(97.0415270179989,1.02444555263128,-7.33933080287894));
#29763=CARTESIAN_POINT('Ctrl Pts',(97.039040317828,1.0258519784978,-7.33913594672454));
#29764=CARTESIAN_POINT('Ctrl Pts',(97.033781089707,1.02880128246279,-7.33872591184219));
#29765=CARTESIAN_POINT('Ctrl Pts',(97.0310073992268,1.03034203066807,-7.33851087413949));
#29766=CARTESIAN_POINT('Ctrl Pts',(97.024105312229,1.03413963116142,-7.33797869070289));
#29767=CARTESIAN_POINT('Ctrl Pts',(97.0199694987162,1.03638302001118,-7.33766237910681));
#29768=CARTESIAN_POINT('Ctrl Pts',(97.0042937001302,1.04476485493732,-7.33647276251103));
#29769=CARTESIAN_POINT('Ctrl Pts',(96.9926647399576,1.05073610291761,-7.33560916077351));
#29770=CARTESIAN_POINT('Ctrl Pts',(96.9625140858283,1.06558885834615,-7.33341206362287));
#29771=CARTESIAN_POINT('Ctrl Pts',(96.9438546017547,1.0741819666713,-7.33209228504785));
#29772=CARTESIAN_POINT('Ctrl Pts',(96.8718965799324,1.10506515197573,-7.32711812537154));
#29773=CARTESIAN_POINT('Ctrl Pts',(96.8172070537007,1.12391240568597,-7.32357120277021));
#29774=CARTESIAN_POINT('Ctrl Pts',(96.6884212599415,1.15794153465484,-7.31532316964458));
#29775=CARTESIAN_POINT('Ctrl Pts',(96.6138178078214,1.17015852961668,-7.31061190277869));
#29776=CARTESIAN_POINT('Ctrl Pts',(96.528197767502,1.17584753754396,-7.30498023216329));
#29777=CARTESIAN_POINT('Ctrl Pts',(96.5178229966456,1.17639911485073,-7.30429440758684));
#29778=CARTESIAN_POINT('Ctrl Pts',(96.5007223101016,1.17708153028367,-7.30315767469362));
#29779=CARTESIAN_POINT('Ctrl Pts',(96.4940000170793,1.17729213239372,-7.30270922586411));
#29780=CARTESIAN_POINT('Ctrl Pts',(96.4818490600108,1.17756865518606,-7.30189557389904));
#29781=CARTESIAN_POINT('Ctrl Pts',(96.476421005871,1.17765463814315,-7.30153100037028));
#29782=CARTESIAN_POINT('Ctrl Pts',(96.4647693167382,1.17775863617915,-7.30074596679458));
#29783=CARTESIAN_POINT('Ctrl Pts',(96.4585457684928,1.17776485246227,-7.30032515340624));
#29784=CARTESIAN_POINT('Ctrl Pts',(96.4414887046712,1.17764669374707,-7.29916755468797));
#29785=CARTESIAN_POINT('Ctrl Pts',(96.4306567219911,1.1774221598528,-7.29842770984083));
#29786=CARTESIAN_POINT('Ctrl Pts',(96.3664943826372,1.17520620965132,-7.29401605913285));
#29787=CARTESIAN_POINT('Ctrl Pts',(96.3133538030027,1.16974152643362,-7.29023820108482));
#29788=CARTESIAN_POINT('Ctrl Pts',(96.2135222039986,1.15256461326035,-7.28291658145488));
#29789=CARTESIAN_POINT('Ctrl Pts',(96.1668139085357,1.14155728981306,-7.27939540057324));
#29790=CARTESIAN_POINT('Ctrl Pts',(96.0939102860484,1.11960530312535,-7.27380934040356));
#29791=CARTESIAN_POINT('Ctrl Pts',(96.0672113503834,1.11050853330485,-7.27174427099868));
#29792=CARTESIAN_POINT('Ctrl Pts',(96.0084857835527,1.08811589690994,-7.2671874028214));
#29793=CARTESIAN_POINT('Ctrl Pts',(95.9766647592157,1.07434548673394,-7.26470809197181));
#29794=CARTESIAN_POINT('Ctrl Pts',(95.9400412828461,1.05653886952192,-7.26187761570583));
#29795=CARTESIAN_POINT('Ctrl Pts',(95.9346085123334,1.05384534592833,-7.26145836432119));
#29796=CARTESIAN_POINT('Ctrl Pts',(95.9267272622495,1.04986176209182,-7.26085132993787));
#29797=CARTESIAN_POINT('Ctrl Pts',(95.9242622558478,1.0486048975143,-7.26066163643734));
#29798=CARTESIAN_POINT('Ctrl Pts',(95.9218016730718,1.04733934308028,-7.26047246820102));
#29799=CARTESIAN_POINT('',(97.6382304121186,-0.00105003317618258,-7.32539498110769));
#29800=CARTESIAN_POINT('Ctrl Pts',(95.921801726504,1.04733937056209,-7.16216478479583));
#29801=CARTESIAN_POINT('Ctrl Pts',(95.9591974350094,1.06657314690066,-7.16518958624442));
#29802=CARTESIAN_POINT('Ctrl Pts',(95.9976046480664,1.08379451576264,-7.16826302779609));
#29803=CARTESIAN_POINT('Ctrl Pts',(96.1025184098093,1.12423731727004,-7.17651154264819));
#29804=CARTESIAN_POINT('Ctrl Pts',(96.17031902097,1.14361469209607,-7.18169729887447));
#29805=CARTESIAN_POINT('Ctrl Pts',(96.2491066072225,1.15866846873086,-7.18731936563644));
#29806=CARTESIAN_POINT('Ctrl Pts',(96.2587871500516,1.16039276109642,-7.18800317998797));
#29807=CARTESIAN_POINT('Ctrl Pts',(96.2723256823316,1.16262968461514,-7.18894878999018));
#29808=CARTESIAN_POINT('Ctrl Pts',(96.2761660133341,1.16324468341463,-7.18921582109563));
#29809=CARTESIAN_POINT('Ctrl Pts',(96.282820477877,1.16427656144637,-7.18967637140375));
#29810=CARTESIAN_POINT('Ctrl Pts',(96.2856331761037,1.16470228440079,-7.18987037012976));
#29811=CARTESIAN_POINT('Ctrl Pts',(96.2916000298121,1.16558331020396,-7.19028046845593));
#29812=CARTESIAN_POINT('Ctrl Pts',(96.2947545482123,1.16603601080375,-7.19049641712659));
#29813=CARTESIAN_POINT('Ctrl Pts',(96.3026380899499,1.16713472850511,-7.19103404198624));
#29814=CARTESIAN_POINT('Ctrl Pts',(96.307369336814,1.16776482170248,-7.19135484617066));
#29815=CARTESIAN_POINT('Ctrl Pts',(96.3255705739285,1.17007628634915,-7.19258234695495));
#29816=CARTESIAN_POINT('Ctrl Pts',(96.3390660376483,1.17155357682746,-7.19347852595174));
#29817=CARTESIAN_POINT('Ctrl Pts',(96.3741438293579,1.17478069999937,-7.1957787605492));
#29818=CARTESIAN_POINT('Ctrl Pts',(96.3957548727367,1.17616939298684,-7.19716742438219));
#29819=CARTESIAN_POINT('Ctrl Pts',(96.5196859976844,1.18070642880199,-7.20502956792278));
#29820=CARTESIAN_POINT('Ctrl Pts',(96.6220314712868,1.17110053595687,-7.21116672083788));
#29821=CARTESIAN_POINT('Ctrl Pts',(96.7534657819626,1.14118633580097,-7.21974864204908));
#29822=CARTESIAN_POINT('Ctrl Pts',(96.7847679230462,1.13268884921638,-7.22184330644841));
#29823=CARTESIAN_POINT('Ctrl Pts',(96.824970971947,1.11997191619762,-7.22462111372228));
#29824=CARTESIAN_POINT('Ctrl Pts',(96.8342271881816,1.11691710042995,-7.22526677972755));
#29825=CARTESIAN_POINT('Ctrl Pts',(96.8491056710481,1.1118011199322,-7.22631503660085));
#29826=CARTESIAN_POINT('Ctrl Pts',(96.8547521274066,1.1098113085187,-7.22671529761028));
#29827=CARTESIAN_POINT('Ctrl Pts',(96.8655286333175,1.1059210475786,-7.22748401734929));
#29828=CARTESIAN_POINT('Ctrl Pts',(96.8706611054725,1.10402772952428,-7.2278522335152));
#29829=CARTESIAN_POINT('Ctrl Pts',(96.8820576079503,1.09973323403487,-7.22867462880464));
#29830=CARTESIAN_POINT('Ctrl Pts',(96.8883146478405,1.09731417029696,-7.22912938893054));
#29831=CARTESIAN_POINT('Ctrl Pts',(96.9077542326644,1.08960699927538,-7.23055258095497));
#29832=CARTESIAN_POINT('Ctrl Pts',(96.9208615922565,1.08413395663274,-7.23152710457075));
#29833=CARTESIAN_POINT('Ctrl Pts',(96.9510925451723,1.07086378541808,-7.23381063586987));
#29834=CARTESIAN_POINT('Ctrl Pts',(96.9681342656382,1.06289088205631,-7.23512522789101));
#29835=CARTESIAN_POINT('Ctrl Pts',(97.0280365758891,1.03309655741813,-7.23984508616663));
#29836=CARTESIAN_POINT('Ctrl Pts',(97.0697395585445,1.00906439763026,-7.2433175154822));
#29837=CARTESIAN_POINT('Ctrl Pts',(97.1709907925111,0.942147163313296,-7.2521827165742));
#29838=CARTESIAN_POINT('Ctrl Pts',(97.22822477813,0.896122516800112,-7.2576160465742));
#29839=CARTESIAN_POINT('Ctrl Pts',(97.2951699905241,0.831137604939691,-7.26427421868002));
#29840=CARTESIAN_POINT('Ctrl Pts',(97.3091722573297,0.816834556961828,-7.26568529166555));
#29841=CARTESIAN_POINT('Ctrl Pts',(97.3266907615216,0.798002622476429,-7.26746729384109));
#29842=CARTESIAN_POINT('Ctrl Pts',(97.3305470454988,0.793796331445133,-7.26786063360503));
#29843=CARTESIAN_POINT('Ctrl Pts',(97.3366462279603,0.787045721925327,-7.26848424106066));
#29844=CARTESIAN_POINT('Ctrl Pts',(97.3389089112597,0.784519521946573,-7.26871592110936));
#29845=CARTESIAN_POINT('Ctrl Pts',(97.3432129821596,0.779672222969465,-7.26915720298308));
#29846=CARTESIAN_POINT('Ctrl Pts',(97.345256168005,0.777352834745229,-7.26936693010767));
#29847=CARTESIAN_POINT('Ctrl Pts',(97.350097796024,0.771812886475229,-7.26986455851786));
#29848=CARTESIAN_POINT('Ctrl Pts',(97.35288794527,0.768585077048926,-7.27015185927811));
#29849=CARTESIAN_POINT('Ctrl Pts',(97.362016261522,0.757908175426811,-7.27109381882598));
#29850=CARTESIAN_POINT('Ctrl Pts',(97.3682793829589,0.750395056415769,-7.27174336064407));
#29851=CARTESIAN_POINT('Ctrl Pts',(97.4154394840695,0.692367945131401,-7.27666721329326));
#29852=CARTESIAN_POINT('Ctrl Pts',(97.4521910511448,0.63861767252533,-7.28070108974733));
#29853=CARTESIAN_POINT('Ctrl Pts',(97.5068147296403,0.54254182391545,-7.28754150059198));
#29854=CARTESIAN_POINT('Ctrl Pts',(97.526994660201,0.501711418860703,-7.29034667458858));
#29855=CARTESIAN_POINT('Ctrl Pts',(97.563711822864,0.415129839834728,-7.29624541427028));
#29856=CARTESIAN_POINT('Ctrl Pts',(97.5798798595034,0.369318792195161,-7.29934051304164));
#29857=CARTESIAN_POINT('Ctrl Pts',(97.5961430672416,0.312224297856886,-7.30324119576074));
#29858=CARTESIAN_POINT('Ctrl Pts',(97.5989672688397,0.301763725041129,-7.30395745700501));
#29859=CARTESIAN_POINT('Ctrl Pts',(97.6032013897438,0.285174647001968,-7.30509656698941));
#29860=CARTESIAN_POINT('Ctrl Pts',(97.6047072851678,0.279071091346675,-7.30551635624563));
#29861=CARTESIAN_POINT('Ctrl Pts',(97.6074210590021,0.267680512804017,-7.30630117707449));
#29862=CARTESIAN_POINT('Ctrl Pts',(97.6086414290489,0.262396614380233,-7.30666580107502));
#29863=CARTESIAN_POINT('Ctrl Pts',(97.6109602119369,0.252030870645167,-7.30738227873806));
#29864=CARTESIAN_POINT('Ctrl Pts',(97.6120615531454,0.246949802320305,-7.30773403034554));
#29865=CARTESIAN_POINT('Ctrl Pts',(97.6144636450787,0.235502072818314,-7.30852783677025));
#29866=CARTESIAN_POINT('Ctrl Pts',(97.6157454101175,0.229131645776193,-7.30897047856181));
#29867=CARTESIAN_POINT('Ctrl Pts',(97.6188481042354,0.213022875997737,-7.31009218523653));
#29868=CARTESIAN_POINT('Ctrl Pts',(97.620598965071,0.203271715843115,-7.31077340664094));
#29869=CARTESIAN_POINT('Ctrl Pts',(97.6329375460311,0.129192640195376,-7.31596632696674));
#29870=CARTESIAN_POINT('Ctrl Pts',(97.6382886189501,0.0641194517159614,
-7.32063848889019));
#29871=CARTESIAN_POINT('Ctrl Pts',(97.6382304809295,-0.00105066599438048,
-7.32539490694684));
#29872=CARTESIAN_POINT('Ctrl Pts',(97.638230481486,-0.00105004197394352,
-7.32539486140295));
#29873=CARTESIAN_POINT('Ctrl Pts',(97.638157620742,-0.0827722104236852,
-7.33135932450499));
#29874=CARTESIAN_POINT('Ctrl Pts',(97.6295793538412,-0.164269445791813,
-7.33743351708362));
#29875=CARTESIAN_POINT('Ctrl Pts',(97.610523462441,-0.254166306561867,-7.34393779875387));
#29876=CARTESIAN_POINT('Ctrl Pts',(97.6082879512948,-0.264078388432546,
-7.34465193898493));
#29877=CARTESIAN_POINT('Ctrl Pts',(97.6046581051944,-0.279254958818313,
-7.34573949217641));
#29878=CARTESIAN_POINT('Ctrl Pts',(97.6033551261193,-0.284540532751324,
-7.34611715363922));
#29879=CARTESIAN_POINT('Ctrl Pts',(97.6008571483418,-0.294379596564185,
-7.34681787358606));
#29880=CARTESIAN_POINT('Ctrl Pts',(97.5996714113404,-0.298935302869374,
-7.34714140085036));
#29881=CARTESIAN_POINT('Ctrl Pts',(97.5976407119398,-0.306549842746858,
-7.347680469905));
#29882=CARTESIAN_POINT('Ctrl Pts',(97.5968106548838,-0.309612552776908,
-7.34789683566885));
#29883=CARTESIAN_POINT('Ctrl Pts',(97.5952099831903,-0.315425490058207,
-7.34830657298591));
#29884=CARTESIAN_POINT('Ctrl Pts',(97.5944417290941,-0.318176319770466,
-7.34850008106393));
#29885=CARTESIAN_POINT('Ctrl Pts',(97.5925913664677,-0.32470994203855,-7.34895882277975));
#29886=CARTESIAN_POINT('Ctrl Pts',(97.5915002855447,-0.3284901905073,-7.34922354965856));
#29887=CARTESIAN_POINT('Ctrl Pts',(97.5875710231533,-0.341852147389928,
-7.35015704847638));
#29888=CARTESIAN_POINT('Ctrl Pts',(97.5846297642654,-0.351403448008432,
-7.35082026511642));
#29889=CARTESIAN_POINT('Ctrl Pts',(97.5620452483513,-0.421555926547498,
-7.35566937701087));
#29890=CARTESIAN_POINT('Ctrl Pts',(97.5376327908623,-0.480519891455983,
-7.35962630864354));
#29891=CARTESIAN_POINT('Ctrl Pts',(97.4836892790883,-0.585759495725363,
-7.36694691844554));
#29892=CARTESIAN_POINT('Ctrl Pts',(97.4554713634781,-0.632505505260704,
-7.37030526359025));
#29893=CARTESIAN_POINT('Ctrl Pts',(97.4001217422688,-0.711275037832558,
-7.3763807779452));
#29894=CARTESIAN_POINT('Ctrl Pts',(97.3743302486744,-0.74412087238454,-7.37905823658713));
#29895=CARTESIAN_POINT('Ctrl Pts',(97.3404058631544,-0.782894019470938,
-7.38244875230918));
#29896=CARTESIAN_POINT('Ctrl Pts',(97.3338681322983,-0.790180814025435,
-7.38309658342121));
#29897=CARTESIAN_POINT('Ctrl Pts',(97.3237278757249,-0.801203297629566,
-7.38409348163802));
#29898=CARTESIAN_POINT('Ctrl Pts',(97.3201901267464,-0.804998204268755,
-7.38443984738119));
#29899=CARTESIAN_POINT('Ctrl Pts',(97.313265587889,-0.812328376056222,-7.38511511266905));
#29900=CARTESIAN_POINT('Ctrl Pts',(97.30988159626,-0.81586614715012,-7.38544388964002));
#29901=CARTESIAN_POINT('Ctrl Pts',(97.3022092642363,-0.823787662643767,
-7.38618664145084));
#29902=CARTESIAN_POINT('Ctrl Pts',(97.2979085713053,-0.82815919045536,-7.38660114328146));
#29903=CARTESIAN_POINT('Ctrl Pts',(97.2862120990038,-0.839864039181051,
-7.38772365624678));
#29904=CARTESIAN_POINT('Ctrl Pts',(97.2787530072162,-0.847133025592625,
-7.38843442434006));
#29905=CARTESIAN_POINT('Ctrl Pts',(97.2423415226478,-0.881686894131928,
-7.39188079997064));
#29906=CARTESIAN_POINT('Ctrl Pts',(97.212118608622,-0.907589075905287,-7.39467325356153));
#29907=CARTESIAN_POINT('Ctrl Pts',(97.1057980421773,-0.989751887259648,
-7.40427882677055));
#29908=CARTESIAN_POINT('Ctrl Pts',(97.024255105031,-1.0383633716278,-7.41132757327188));
#29909=CARTESIAN_POINT('Ctrl Pts',(96.9185086385123,-1.08524223256013,-7.41968734711519));
#29910=CARTESIAN_POINT('Ctrl Pts',(96.8989961616024,-1.09327241939852,-7.42119812811534));
#29911=CARTESIAN_POINT('Ctrl Pts',(96.8669058572911,-1.10548137299237,-7.42362080027618));
#29912=CARTESIAN_POINT('Ctrl Pts',(96.8544551886515,-1.10997955266591,-7.42454592111846));
#29913=CARTESIAN_POINT('Ctrl Pts',(96.8374090132999,-1.11581501108063,-7.42578999034491));
#29914=CARTESIAN_POINT('Ctrl Pts',(96.8328778510732,-1.11733542587152,-7.42611854108084));
#29915=CARTESIAN_POINT('Ctrl Pts',(96.8253088424273,-1.1198240197441,-7.426663652408));
#29916=CARTESIAN_POINT('Ctrl Pts',(96.822276139186,-1.12080750715113,-7.42688107565991));
#29917=CARTESIAN_POINT('Ctrl Pts',(96.8165309419425,-1.12264489115577,-7.42729104866585));
#29918=CARTESIAN_POINT('Ctrl Pts',(96.8138192926112,-1.1235012970534,-7.42748374621271));
#29919=CARTESIAN_POINT('Ctrl Pts',(96.8073957968243,-1.12550443961412,-7.42793837752827));
#29920=CARTESIAN_POINT('Ctrl Pts',(96.803681297167,-1.12664265732642,-7.4281998259278));
#29921=CARTESIAN_POINT('Ctrl Pts',(96.7905723515356,-1.13058872553943,-7.42911763244383));
#29922=CARTESIAN_POINT('Ctrl Pts',(96.7811482311819,-1.13329771456478,-7.42976864605399));
#29923=CARTESIAN_POINT('Ctrl Pts',(96.7031736702421,-1.15466113281394,-7.43509117624486));
#29924=CARTESIAN_POINT('Ctrl Pts',(96.6330883105678,-1.16719818577864,-7.43947526903408));
#29925=CARTESIAN_POINT('Ctrl Pts',(96.5035800790976,-1.17843564929446,-7.44751619979219));
#29926=CARTESIAN_POINT('Ctrl Pts',(96.44457251753,-1.17911593092873,-7.45115801567501));
#29927=CARTESIAN_POINT('Ctrl Pts',(96.3645746375355,-1.17403060157308,-7.45626716080015));
#29928=CARTESIAN_POINT('Ctrl Pts',(96.3434264095497,-1.1721109282954,-7.45763366360753));
#29929=CARTESIAN_POINT('Ctrl Pts',(96.3067312214503,-1.16777703170361,-7.46004064338165));
#29930=CARTESIAN_POINT('Ctrl Pts',(96.2911590356336,-1.16562096166176,-7.46107340279646));
#29931=CARTESIAN_POINT('Ctrl Pts',(96.268526703433,-1.16202428432297,-7.46259309967684));
#29932=CARTESIAN_POINT('Ctrl Pts',(96.2614288063174,-1.16082949238368,-7.46307239636197));
#29933=CARTESIAN_POINT('Ctrl Pts',(96.2489462960017,-1.15861045713583,-7.46392025091268));
#29934=CARTESIAN_POINT('Ctrl Pts',(96.2435569969662,-1.15761353572798,-7.46428794331594));
#29935=CARTESIAN_POINT('Ctrl Pts',(96.2323294911441,-1.15545549720831,-7.46505745802665));
#29936=CARTESIAN_POINT('Ctrl Pts',(96.2264927493763,-1.15428766515915,-7.46545948198795));
#29937=CARTESIAN_POINT('Ctrl Pts',(96.2112766513671,-1.15112303333598,-7.46651285182607));
#29938=CARTESIAN_POINT('Ctrl Pts',(96.2019125478508,-1.14905586997392,-7.4671663964536));
#29939=CARTESIAN_POINT('Ctrl Pts',(96.1624157983958,-1.13982956473642,-7.46994609190785));
#29940=CARTESIAN_POINT('Ctrl Pts',(96.1325489171274,-1.1315982267196,-7.47210568749937));
#29941=CARTESIAN_POINT('Ctrl Pts',(96.0239005324763,-1.09699208501677,-7.4801811728874));
#29942=CARTESIAN_POINT('Ctrl Pts',(95.947654416635,-1.06348469239176,-7.48630334749115));
#29943=CARTESIAN_POINT('Ctrl Pts',(95.8303154980595,-0.996346338643619,
-7.49619936972193));
#29944=CARTESIAN_POINT('Ctrl Pts',(95.7868168949102,-0.967467086651361,
-7.49998273243608));
#29945=CARTESIAN_POINT('Ctrl Pts',(95.739843511886,-0.93157133641251,-7.5040945736259));
#29946=CARTESIAN_POINT('Ctrl Pts',(95.7343525980531,-0.92729773772543,-7.50457561350047));
#29947=CARTESIAN_POINT('Ctrl Pts',(95.726030341534,-0.920701239751516,-7.50530489311694));
#29948=CARTESIAN_POINT('Ctrl Pts',(95.7231715390142,-0.918413470364259,
-7.50555544572017));
#29949=CARTESIAN_POINT('Ctrl Pts',(95.7179571203013,-0.914200568654421,
-7.5060124443317));
#29950=CARTESIAN_POINT('Ctrl Pts',(95.71559828447,-0.91227963500244,-7.50621916624076));
#29951=CARTESIAN_POINT('Ctrl Pts',(95.7102894388488,-0.907922022309581,
-7.50668441614867));
#29952=CARTESIAN_POINT('Ctrl Pts',(95.7073438423781,-0.905480093738512,
-7.5069425658723));
#29953=CARTESIAN_POINT('Ctrl Pts',(95.6997606455557,-0.899130943647556,
-7.5076073271905));
#29954=CARTESIAN_POINT('Ctrl Pts',(95.6951411585998,-0.89520212407097,-7.5080124543006));
#29955=CARTESIAN_POINT('Ctrl Pts',(95.6643153242603,-0.868572080151798,
-7.51071865403968));
#29956=CARTESIAN_POINT('Ctrl Pts',(95.6390893606961,-0.84475648876388,-7.51294706388831));
#29957=CARTESIAN_POINT('Ctrl Pts',(95.5952711707043,-0.799566222936112,
-7.51692435876652));
#29958=CARTESIAN_POINT('Ctrl Pts',(95.5763297994118,-0.778569824341681,
-7.51868439317666));
#29959=CARTESIAN_POINT('Ctrl Pts',(95.5272295965055,-0.720037140619252,
-7.52342119575347));
#29960=CARTESIAN_POINT('Ctrl Pts',(95.4985875214946,-0.681302068870754,
-7.52638096158948));
#29961=CARTESIAN_POINT('Ctrl Pts',(95.4434939262649,-0.596366595909807,
-7.53271290005684));
#29962=CARTESIAN_POINT('Ctrl Pts',(95.4176422416363,-0.549910972917084,
-7.53608964263101));
#29963=CARTESIAN_POINT('Ctrl Pts',(95.3904034647755,-0.492083678644121,
-7.54029090448739));
#29964=CARTESIAN_POINT('Ctrl Pts',(95.3859273309835,-0.482230938757396,
-7.54100649707373));
#29965=CARTESIAN_POINT('Ctrl Pts',(95.3790930756971,-0.466619784912922,
-7.5421406529871));
#29966=CARTESIAN_POINT('Ctrl Pts',(95.3766436574041,-0.460901810625772,
-7.54255613447892));
#29967=CARTESIAN_POINT('Ctrl Pts',(95.3721417316361,-0.450158058904509,
-7.54333706074196));
#29968=CARTESIAN_POINT('Ctrl Pts',(95.3700784450415,-0.445136953889366,
-7.54370213276935));
#29969=CARTESIAN_POINT('Ctrl Pts',(95.365535696516,-0.433860838211755,-7.54452231733685));
#29970=CARTESIAN_POINT('Ctrl Pts',(95.3630749933896,-0.427598524565747,
-7.54497803939264));
#29971=CARTESIAN_POINT('Ctrl Pts',(95.3569478850125,-0.411604166266832,
-7.54614271775527));
#29972=CARTESIAN_POINT('Ctrl Pts',(95.3533565415494,-0.401844182991244,
-7.54685411167661));
#29973=CARTESIAN_POINT('Ctrl Pts',(95.3249289675635,-0.321313089346457,
-7.55273104885834));
#29974=CARTESIAN_POINT('Ctrl Pts',(95.3067804238525,-0.248378113446867,
-7.55811532245824));
#29975=CARTESIAN_POINT('Ctrl Pts',(95.2872919586694,-0.118087669317124,
-7.56775092128684));
#29976=CARTESIAN_POINT('Ctrl Pts',(95.2829642828051,-0.0614150673103769,
-7.57194274071615));
#29977=CARTESIAN_POINT('Ctrl Pts',(95.2826555066454,0.0167799672035462,
-7.57759659982393));
#29978=CARTESIAN_POINT('Ctrl Pts',(95.2831558334285,0.0382102534638454,
-7.57913210938997));
#29979=CARTESIAN_POINT('Ctrl Pts',(95.2849228949759,0.0730747710711165,
-7.58159604245247));
#29980=CARTESIAN_POINT('Ctrl Pts',(95.2858360048942,0.0865214109962014,
-7.58253802065525));
#29981=CARTESIAN_POINT('Ctrl Pts',(95.2873836960152,0.10469265036322,-7.58379715924895));
#29982=CARTESIAN_POINT('Ctrl Pts',(95.2878163849017,0.109432801584641,-7.58412434257435));
#29983=CARTESIAN_POINT('Ctrl Pts',(95.2885864635311,0.117339311282526,-7.58466780720895));
#29984=CARTESIAN_POINT('Ctrl Pts',(95.2889079742152,0.120507114021598,-7.58488494061709));
#29985=CARTESIAN_POINT('Ctrl Pts',(95.2895412808636,0.126504780577694,-7.58529483964327));
#29986=CARTESIAN_POINT('Ctrl Pts',(95.2898504964252,0.129334874909668,-7.58548775002663));
#29987=CARTESIAN_POINT('Ctrl Pts',(95.2906074015932,0.136037270219565,-7.58594346932322));
#29988=CARTESIAN_POINT('Ctrl Pts',(95.2910640630389,0.139908554822893,-7.58620578721081));
#29989=CARTESIAN_POINT('Ctrl Pts',(95.2927368306378,0.15350849710487,-7.58712436331314));
#29990=CARTESIAN_POINT('Ctrl Pts',(95.2940552266629,0.163224490437702,-7.58777528712605));
#29991=CARTESIAN_POINT('Ctrl Pts',(95.3058338955376,0.242577520562612,-7.59305630224015));
#29992=CARTESIAN_POINT('Ctrl Pts',(95.3224005554039,0.311174301414529,-7.59740421450017));
#29993=CARTESIAN_POINT('Ctrl Pts',(95.3640468312999,0.434109420209981,-7.60543313266074));
#29994=CARTESIAN_POINT('Ctrl Pts',(95.3873149324483,0.488807534187662,-7.60910009493874));
#29995=CARTESIAN_POINT('Ctrl Pts',(95.4244084299881,0.560449221728249,-7.61424133277476));
#29996=CARTESIAN_POINT('Ctrl Pts',(95.4347228311029,0.579111212913541,-7.61561328863156));
#29997=CARTESIAN_POINT('Ctrl Pts',(95.4535375380097,0.611071766647473,-7.61802900246984));
#29998=CARTESIAN_POINT('Ctrl Pts',(95.4618093112538,0.62449872592867,-7.61906496358505));
#29999=CARTESIAN_POINT('Ctrl Pts',(95.4742503221216,0.643813753243735,-7.62058850518528));
#30000=CARTESIAN_POINT('Ctrl Pts',(95.4782082387301,0.6498363771467,-7.621068388979));
#30001=CARTESIAN_POINT('Ctrl Pts',(95.485273734165,0.660375652247995,-7.62191691462782));
#30002=CARTESIAN_POINT('Ctrl Pts',(95.4883580718981,0.664907680836141,-7.62228468649131));
#30003=CARTESIAN_POINT('Ctrl Pts',(95.4948548926377,0.674312067393965,-7.6230540034452));
#30004=CARTESIAN_POINT('Ctrl Pts',(95.4982728665639,0.679180424349913,-7.62345574775843));
#30005=CARTESIAN_POINT('Ctrl Pts',(95.5072862127381,0.691813890705781,-7.62450756864363));
#30006=CARTESIAN_POINT('Ctrl Pts',(95.5129395254003,0.699536922402434,-7.62515983203001));
#30007=CARTESIAN_POINT('Ctrl Pts',(95.5371777233368,0.731815952960126,-7.62792612289781));
#30008=CARTESIAN_POINT('Ctrl Pts',(95.5566263823996,0.755705006370475,-7.63007319188216));
#30009=CARTESIAN_POINT('Ctrl Pts',(95.6320125178234,0.841224955868691,-7.63814539601335));
#30010=CARTESIAN_POINT('Ctrl Pts',(95.6934930493862,0.897633303007338,-7.64427850865171));
#30011=CARTESIAN_POINT('Ctrl Pts',(95.8023740553451,0.978118584368847,-7.65419014178745));
#30012=CARTESIAN_POINT('Ctrl Pts',(95.8463786458702,1.00633012099548,-7.6579779348895));
#30013=CARTESIAN_POINT('Ctrl Pts',(95.8982099163185,1.0348887725285,-7.66209394762261));
#30014=CARTESIAN_POINT('Ctrl Pts',(95.9043345337815,1.03819297647297,-7.66257506274894));
#30015=CARTESIAN_POINT('Ctrl Pts',(95.9137261276896,1.04315273805798,-7.66330443239969));
#30016=CARTESIAN_POINT('Ctrl Pts',(95.9169720073122,1.04484759691054,-7.66355500063715));
#30017=CARTESIAN_POINT('Ctrl Pts',(95.9207508843772,1.04679838957602,-7.66384491542143));
#30018=CARTESIAN_POINT('Ctrl Pts',(95.9212761773124,1.04706906422808,-7.66388517556795));
#30019=CARTESIAN_POINT('Ctrl Pts',(95.9218016730721,1.04733934308044,-7.66392541087522));
#30020=CARTESIAN_POINT('Origin',(96.460480949577,-7.19464945638997E-16,
0.924367114736168));
#30021=CARTESIAN_POINT('',(95.9218015205746,1.0473392646462,-8.26212858994183));
#30022=CARTESIAN_POINT('',(95.9218018246468,1.04733942104002,-8.16230712347375));
#30023=CARTESIAN_POINT('',(95.9218016730721,1.04733934308042,0.924367114736168));
#30024=CARTESIAN_POINT('',(97.6382307576569,0.000672359933839044,-7.92526064390542));
#30025=CARTESIAN_POINT('Ctrl Pts',(95.9218015205746,1.04733926464621,-8.26212858994183));
#30026=CARTESIAN_POINT('Ctrl Pts',(95.882681846614,1.02721878951153,-8.25936245837624));
#30027=CARTESIAN_POINT('Ctrl Pts',(95.8447008289881,1.00491246711868,-8.25655020994838));
#30028=CARTESIAN_POINT('Ctrl Pts',(95.7993899953988,0.974762406621344,-8.25297826354386));
#30029=CARTESIAN_POINT('Ctrl Pts',(95.7908173484039,0.968893001898539,-8.25229243871632));
#30030=CARTESIAN_POINT('Ctrl Pts',(95.7768249461735,0.959038458591712,-8.25115570549246));
#30031=CARTESIAN_POINT('Ctrl Pts',(95.7713595746905,0.955118853113391,-8.25070725658608));
#30032=CARTESIAN_POINT('Ctrl Pts',(95.7615439012237,0.94795123095032,-8.24989360453923));
#30033=CARTESIAN_POINT('Ctrl Pts',(95.7571818866182,0.94471951402355,-8.24952903100594));
#30034=CARTESIAN_POINT('Ctrl Pts',(95.7478675076307,0.937718442569192,-8.2487439974839));
#30035=CARTESIAN_POINT('Ctrl Pts',(95.7429223851959,0.933939772840843,-8.24832318415447));
#30036=CARTESIAN_POINT('Ctrl Pts',(95.729451335272,0.923476119660658,-8.24716558576631));
#30037=CARTESIAN_POINT('Ctrl Pts',(95.7209875163982,0.916712544510815,-8.24642574119306));
#30038=CARTESIAN_POINT('Ctrl Pts',(95.6713914557111,0.875945701237547,-8.24201409666496));
#30039=CARTESIAN_POINT('Ctrl Pts',(95.6325214570363,0.839300128391896,-8.23823624487958));
#30040=CARTESIAN_POINT('Ctrl Pts',(95.5637003315537,0.76496950178014,-8.23091462754437));
#30041=CARTESIAN_POINT('Ctrl Pts',(95.5333069540389,0.727833610568228,-8.2273934423024));
#30042=CARTESIAN_POINT('Ctrl Pts',(95.4887689216743,0.666082444684675,-8.22180737492187));
#30043=CARTESIAN_POINT('Ctrl Pts',(95.473100983738,0.64262818596326,-8.21974230271395));
#30044=CARTESIAN_POINT('Ctrl Pts',(95.4400879169729,0.589146750712411,-8.21518543217378));
#30045=CARTESIAN_POINT('Ctrl Pts',(95.423194530971,0.55886779862607,-8.21270612170247));
#30046=CARTESIAN_POINT('Ctrl Pts',(95.4049419280051,0.522464547557197,-8.20987564580925));
#30047=CARTESIAN_POINT('Ctrl Pts',(95.4022659697706,0.51702310383408,-8.20945639443925));
#30048=CARTESIAN_POINT('Ctrl Pts',(95.3979701946385,0.508114748190687,-8.208776548753));
#30049=CARTESIAN_POINT('Ctrl Pts',(95.3963250765105,0.504660262500222,-8.20851450443043));
#30050=CARTESIAN_POINT('Ctrl Pts',(95.3934021177061,0.498444665722067,-8.20804593414983));
#30051=CARTESIAN_POINT('Ctrl Pts',(95.3921181180113,0.495686573332658,-8.2078390443837));
#30052=CARTESIAN_POINT('Ctrl Pts',(95.3893121035893,0.48959756571323,-8.20738456835387));
#30053=CARTESIAN_POINT('Ctrl Pts',(95.3877949290369,0.486264511574047,-8.2071372737954));
#30054=CARTESIAN_POINT('Ctrl Pts',(95.3834395744818,0.476576725492688,-8.20642262318772));
#30055=CARTESIAN_POINT('Ctrl Pts',(95.38064208494,0.470203712391128,-8.20595762994692));
#30056=CARTESIAN_POINT('Ctrl Pts',(95.3573317243991,0.415794497655136,-8.20202815120875));
#30057=CARTESIAN_POINT('Ctrl Pts',(95.3399760945923,0.366460931705132,-8.1987303848441));
#30058=CARTESIAN_POINT('Ctrl Pts',(95.3036000738901,0.23591528754517,-8.19028896714968));
#30059=CARTESIAN_POINT('Ctrl Pts',(95.2898192555901,0.153558411476834,-8.18522162110159));
#30060=CARTESIAN_POINT('Ctrl Pts',(95.2830021057068,0.0397759502831907,
-8.17795051953922));
#30061=CARTESIAN_POINT('Ctrl Pts',(95.2823653890387,0.00905682395242783,
-8.17596322049056));
#30062=CARTESIAN_POINT('Ctrl Pts',(95.2831057553097,-0.0312116579043044,
-8.17330889172885));
#30063=CARTESIAN_POINT('Ctrl Pts',(95.2833979960099,-0.0407704209231531,
-8.17267521516017));
#30064=CARTESIAN_POINT('Ctrl Pts',(95.284060713067,-0.0562659482092893,
-8.17164165295492));
#30065=CARTESIAN_POINT('Ctrl Pts',(95.2843598209786,-0.0622054536819052,
-8.17124397679849));
#30066=CARTESIAN_POINT('Ctrl Pts',(95.2850211371898,-0.0736162789259981,
-8.17047695843129));
#30067=CARTESIAN_POINT('Ctrl Pts',(95.2853765976744,-0.0790878464458857,
-8.17010783472231));
#30068=CARTESIAN_POINT('Ctrl Pts',(95.2862880061383,-0.0917496681503411,
-8.16925045795215));
#30069=CARTESIAN_POINT('Ctrl Pts',(95.286871810717,-0.0989376329198813,
-8.16876135523244));
#30070=CARTESIAN_POINT('Ctrl Pts',(95.2889447249378,-0.121849923252953,
-8.16719444909374));
#30071=CARTESIAN_POINT('Ctrl Pts',(95.2906840942086,-0.137549280856266,
-8.16610897898886));
#30072=CARTESIAN_POINT('Ctrl Pts',(95.2955176631305,-0.174390393026171,
-8.16353261927663));
#30073=CARTESIAN_POINT('Ctrl Pts',(95.2988724329037,-0.195491748269196,
-8.16203420334519));
#30074=CARTESIAN_POINT('Ctrl Pts',(95.3137501292293,-0.275050671341572,
-8.1562977324833));
#30075=CARTESIAN_POINT('Ctrl Pts',(95.329127828755,-0.332690736736164,-8.1519564923183));
#30076=CARTESIAN_POINT('Ctrl Pts',(95.3719464291284,-0.455084718884924,
-8.14244378150568));
#30077=CARTESIAN_POINT('Ctrl Pts',(95.4009595206696,-0.519062251917712,
-8.13727833250891));
#30078=CARTESIAN_POINT('Ctrl Pts',(95.4403418686973,-0.588649468377628,
-8.13167392612265));
#30079=CARTESIAN_POINT('Ctrl Pts',(95.4452971304245,-0.597154728753573,
-8.13098935956052));
#30080=CARTESIAN_POINT('Ctrl Pts',(95.4523602057575,-0.608935777177968,
-8.13004276880873));
#30081=CARTESIAN_POINT('Ctrl Pts',(95.4543783503521,-0.612264465534613,
-8.12977549829468));
#30082=CARTESIAN_POINT('Ctrl Pts',(95.4579003810507,-0.618009194217589,
-8.12931463862833));
#30083=CARTESIAN_POINT('Ctrl Pts',(95.4593965733118,-0.620429877231171,
-8.12912056856425));
#30084=CARTESIAN_POINT('Ctrl Pts',(95.4625864982447,-0.625549260893683,
-8.12871044291798));
#30085=CARTESIAN_POINT('Ctrl Pts',(95.4642824385231,-0.628246560585122,
-8.12849453764082));
#30086=CARTESIAN_POINT('Ctrl Pts',(95.468544014674,-0.634963716069903,-8.12795723052745));
#30087=CARTESIAN_POINT('Ctrl Pts',(95.4711231919266,-0.638974986108999,
-8.12763669830973));
#30088=CARTESIAN_POINT('Ctrl Pts',(95.4811195011341,-0.65431612449475,-8.12641164147063));
#30089=CARTESIAN_POINT('Ctrl Pts',(95.4887078012383,-0.665533939221011,
-8.12551758034506));
#30090=CARTESIAN_POINT('Ctrl Pts',(95.5088840504445,-0.694279448018501,
-8.12322413265107));
#30091=CARTESIAN_POINT('Ctrl Pts',(95.5217635598996,-0.711597067387305,
-8.12184002369523));
#30092=CARTESIAN_POINT('Ctrl Pts',(95.5977405522421,-0.808099058412,-8.11405249659541));
#30093=CARTESIAN_POINT('Ctrl Pts',(95.6703644292126,-0.879240053469003,
-8.10797950064297));
#30094=CARTESIAN_POINT('Ctrl Pts',(95.7778849940188,-0.960351742938887,
-8.09941432605921));
#30095=CARTESIAN_POINT('Ctrl Pts',(95.805416671247,-0.979338133418017,-8.09725649336949));
#30096=CARTESIAN_POINT('Ctrl Pts',(95.8420661468472,-1.00237490534565,-8.09440550694393));
#30097=CARTESIAN_POINT('Ctrl Pts',(95.8504809491419,-1.00751789506175,-8.09375236865836));
#30098=CARTESIAN_POINT('Ctrl Pts',(95.8641280266139,-1.01562512771406,-8.09269491282443));
#30099=CARTESIAN_POINT('Ctrl Pts',(95.8693202675426,-1.01865610218649,-8.09229300117623));
#30100=CARTESIAN_POINT('Ctrl Pts',(95.8792755942964,-1.02436578324012,-8.09152306385312));
#30101=CARTESIAN_POINT('Ctrl Pts',(95.8840345747372,-1.02705136097872,-8.09115529533236));
#30102=CARTESIAN_POINT('Ctrl Pts',(95.8949970879321,-1.03313750833258,-8.09030868778497));
#30103=CARTESIAN_POINT('Ctrl Pts',(95.901212865204,-1.03651546777072,-8.08982906778885));
#30104=CARTESIAN_POINT('Ctrl Pts',(95.9207428057527,-1.04690218442485,-8.0883231439486));
#30105=CARTESIAN_POINT('Ctrl Pts',(95.9341606346707,-1.05371169561501,-8.08728999088254));
#30106=CARTESIAN_POINT('Ctrl Pts',(95.9657610881423,-1.0689946740104,-8.08485911367879));
#30107=CARTESIAN_POINT('Ctrl Pts',(95.9840366153707,-1.07726415922205,-8.08345496690317));
#30108=CARTESIAN_POINT('Ctrl Pts',(96.0517501768846,-1.10584371683332,-8.07825789507965));
#30109=CARTESIAN_POINT('Ctrl Pts',(96.1023390567273,-1.12324727066319,-8.07438197218799));
#30110=CARTESIAN_POINT('Ctrl Pts',(96.2305726227726,-1.15781617635916,-8.06465534113248));
#30111=CARTESIAN_POINT('Ctrl Pts',(96.3091135989226,-1.17067757658251,-8.0587759345803));
#30112=CARTESIAN_POINT('Ctrl Pts',(96.3978885825564,-1.17612434281129,-8.05254872506534));
#30113=CARTESIAN_POINT('Ctrl Pts',(96.4074282834039,-1.17659326163005,-8.05188512750123));
#30114=CARTESIAN_POINT('Ctrl Pts',(96.4207168330286,-1.17708449694094,-8.05096945332527));
#30115=CARTESIAN_POINT('Ctrl Pts',(96.4244613648939,-1.17720503243364,-8.05071238994967));
#30116=CARTESIAN_POINT('Ctrl Pts',(96.4312957886264,-1.17739238995755,-8.05024503438272));
#30117=CARTESIAN_POINT('Ctrl Pts',(96.4343854888847,-1.17746492149759,-8.05003443577605));
#30118=CARTESIAN_POINT('Ctrl Pts',(96.4407889780288,-1.17759002711593,-8.04959942331176));
#30119=CARTESIAN_POINT('Ctrl Pts',(96.4441027480469,-1.17764077753261,-8.04937510982734));
#30120=CARTESIAN_POINT('Ctrl Pts',(96.4527728713507,-1.17773695692433,-8.04879021528799));
#30121=CARTESIAN_POINT('Ctrl Pts',(96.4581294728761,-1.17775983436876,-8.0484308483514));
#30122=CARTESIAN_POINT('Ctrl Pts',(96.4821480357246,-1.17769854689708,-8.04682767123812));
#30123=CARTESIAN_POINT('Ctrl Pts',(96.5008074190952,-1.17720737372872,-8.04560437921946));
#30124=CARTESIAN_POINT('Ctrl Pts',(96.5539292613146,-1.17454433195946,-8.0421650100875));
#30125=CARTESIAN_POINT('Ctrl Pts',(96.5883200204505,-1.17130034575865,-8.03999010945456));
#30126=CARTESIAN_POINT('Ctrl Pts',(96.7001935469232,-1.15576052322287,-8.03294652260264));
#30127=CARTESIAN_POINT('Ctrl Pts',(96.7765919773321,-1.1372414935333,-8.02817300690954));
#30128=CARTESIAN_POINT('Ctrl Pts',(96.8848907960461,-1.0992240030229,-8.02089624246755));
#30129=CARTESIAN_POINT('Ctrl Pts',(96.9186193751852,-1.08559933091248,-8.018555153531));
#30130=CARTESIAN_POINT('Ctrl Pts',(96.9608821034556,-1.06620667203889,-8.01549456926928));
#30131=CARTESIAN_POINT('Ctrl Pts',(96.9700473755437,-1.06185687796953,-8.01482300070829));
#30132=CARTESIAN_POINT('Ctrl Pts',(96.9846082800733,-1.05471441465971,-8.01374290367239));
#30133=CARTESIAN_POINT('Ctrl Pts',(96.9900406150765,-1.05199739229978,-8.01333697325192));
#30134=CARTESIAN_POINT('Ctrl Pts',(97.0002107789363,-1.04681197529418,-8.01257128177804));
#30135=CARTESIAN_POINT('Ctrl Pts',(97.004953318899,-1.04435311928142,-8.01221185882702));
#30136=CARTESIAN_POINT('Ctrl Pts',(97.0137129758967,-1.03973563142965,-8.0115435174496));
#30137=CARTESIAN_POINT('Ctrl Pts',(97.0177346168637,-1.03758575910388,-8.0112349108547));
#30138=CARTESIAN_POINT('Ctrl Pts',(97.0274203983783,-1.03233541970745,-8.01048733093199));
#30139=CARTESIAN_POINT('Ctrl Pts',(97.033071671341,-1.02921164969092,-8.01004754452365));
#30140=CARTESIAN_POINT('Ctrl Pts',(97.0472406054713,-1.02122688259445,-8.00893566694788));
#30141=CARTESIAN_POINT('Ctrl Pts',(97.0557236336438,-1.01630574953466,-8.00826147434284));
#30142=CARTESIAN_POINT('Ctrl Pts',(97.0798381379711,-1.0019110772545,-8.00632008186966));
#30143=CARTESIAN_POINT('Ctrl Pts',(97.0953112850696,-0.99217917532878,-8.00504393221268));
#30144=CARTESIAN_POINT('Ctrl Pts',(97.1488365689114,-0.956749502199679,
-8.00052014805598));
#30145=CARTESIAN_POINT('Ctrl Pts',(97.1856036031758,-0.929192889135423,
-7.99721133302771));
#30146=CARTESIAN_POINT('Ctrl Pts',(97.2724299281134,-0.855819507330814,
-7.98891915041526));
#30147=CARTESIAN_POINT('Ctrl Pts',(97.3203218699485,-0.80768925115512,-7.98389915104469));
#30148=CARTESIAN_POINT('Ctrl Pts',(97.3815158761386,-0.734541518744345,
-7.97702980782797));
#30149=CARTESIAN_POINT('Ctrl Pts',(97.3984749759291,-0.712758066103191,
-7.97506838108668));
#30150=CARTESIAN_POINT('Ctrl Pts',(97.4183180867831,-0.685333598737634,
-7.97271843286279));
#30151=CARTESIAN_POINT('Ctrl Pts',(97.4219414803578,-0.680240968336361,
-7.97228692665625));
#30152=CARTESIAN_POINT('Ctrl Pts',(97.4275579999866,-0.672212487577854,
-7.9716145560675));
#30153=CARTESIAN_POINT('Ctrl Pts',(97.4295786270648,-0.669296154336314,
-7.97137193213941));
#30154=CARTESIAN_POINT('Ctrl Pts',(97.4332970930069,-0.663877216469327,
-7.97092415019197));
#30155=CARTESIAN_POINT('Ctrl Pts',(97.4349984661246,-0.661377212879593,
-7.97071876641029));
#30156=CARTESIAN_POINT('Ctrl Pts',(97.4389061118847,-0.655587486987043,
-7.97024584804853));
#30157=CARTESIAN_POINT('Ctrl Pts',(97.4411054357761,-0.652293162265798,
-7.96997877282884));
#30158=CARTESIAN_POINT('Ctrl Pts',(97.4479511871981,-0.641926165725371,
-7.96914438775376));
#30159=CARTESIAN_POINT('Ctrl Pts',(97.4525381589471,-0.634814284570565,
-7.96858080896662));
#30160=CARTESIAN_POINT('Ctrl Pts',(97.4631690587488,-0.617934891994223,
-7.96726230295342));
#30161=CARTESIAN_POINT('Ctrl Pts',(97.4691476438505,-0.608127039652732,
-7.96651099676791));
#30162=CARTESIAN_POINT('Ctrl Pts',(97.4903188745895,-0.572224239362974,
-7.96380812365564));
#30163=CARTESIAN_POINT('Ctrl Pts',(97.5046509938826,-0.545633493795853,
-7.96189557052363));
#30164=CARTESIAN_POINT('Ctrl Pts',(97.5558766097704,-0.441164320400889,
-7.95460803341234));
#30165=CARTESIAN_POINT('Ctrl Pts',(97.5852041854912,-0.359882674271186,
-7.94938736772712));
#30166=CARTESIAN_POINT('Ctrl Pts',(97.6134975550974,-0.242568601285419,
-7.94172654504229));
#30167=CARTESIAN_POINT('Ctrl Pts',(97.6201112343303,-0.208672169309545,
-7.93950201758299));
#30168=CARTESIAN_POINT('Ctrl Pts',(97.62675719429,-0.164321264077293,-7.93655143866693));
#30169=CARTESIAN_POINT('Ctrl Pts',(97.6281534480907,-0.154086605225606,
-7.93586787151051));
#30170=CARTESIAN_POINT('Ctrl Pts',(97.6301615643288,-0.137766846607678,
-7.93477303215731));
#30171=CARTESIAN_POINT('Ctrl Pts',(97.6308609824075,-0.131692903840552,
-7.93436448635546));
#30172=CARTESIAN_POINT('Ctrl Pts',(97.6320815070449,-0.120314595326233,
-7.93359704290566));
#30173=CARTESIAN_POINT('Ctrl Pts',(97.6326139634476,-0.115011583338101,
-7.93323850777708));
#30174=CARTESIAN_POINT('Ctrl Pts',(97.6335993547528,-0.104478821721182,
-7.93252461309413));
#30175=CARTESIAN_POINT('Ctrl Pts',(97.6340533559106,-0.0992492937059147,
-7.93216929534758));
#30176=CARTESIAN_POINT('Ctrl Pts',(97.6350048828449,-0.0873675624448035,
-7.93135995466523));
#30177=CARTESIAN_POINT('Ctrl Pts',(97.6354808770979,-0.0807138645901476,
-7.93090527670038));
#30178=CARTESIAN_POINT('Ctrl Pts',(97.6374679059321,-0.0491759301201907,
-7.92874301648142));
#30179=CARTESIAN_POINT('Ctrl Pts',(97.6382449876383,-0.0242538099230699,
-7.92701314135852));
#30180=CARTESIAN_POINT('Ctrl Pts',(97.6382307576569,0.000672359933839044,
-7.92526064390542));
#30181=CARTESIAN_POINT('Ctrl Pts',(97.6382307583967,0.000671062669383031,
-7.92526073511286));
#30182=CARTESIAN_POINT('Ctrl Pts',(97.6381788678385,0.0917416851970525,
-7.91885778732613));
#30183=CARTESIAN_POINT('Ctrl Pts',(97.6275636890022,0.182492453302888,-7.91214600970138));
#30184=CARTESIAN_POINT('Ctrl Pts',(97.5947290699091,0.321306745803253,-7.90170620881246));
#30185=CARTESIAN_POINT('Ctrl Pts',(97.5795656154965,0.370685317609632,-7.89796480067282));
#30186=CARTESIAN_POINT('Ctrl Pts',(97.5587390848017,0.42540851181193,-7.89389245952835));
#30187=CARTESIAN_POINT('Ctrl Pts',(97.5562103528544,0.431880092304319,-7.89341211582663));
#30188=CARTESIAN_POINT('Ctrl Pts',(97.5522624328536,0.441725760558389,-7.89268365600119));
#30189=CARTESIAN_POINT('Ctrl Pts',(97.5508845945892,0.445116104657489,-7.89243323497917));
#30190=CARTESIAN_POINT('Ctrl Pts',(97.5483323484103,0.451313253910075,-7.89197634301844));
#30191=CARTESIAN_POINT('Ctrl Pts',(97.547162863573,0.454121941042803,-7.89176959733242));
#30192=CARTESIAN_POINT('Ctrl Pts',(97.5444969317415,0.460455290347638,-7.8913041262469));
#30193=CARTESIAN_POINT('Ctrl Pts',(97.5429941715983,0.463977207610486,-7.89104578054566));
#30194=CARTESIAN_POINT('Ctrl Pts',(97.5390635449132,0.473066096652275,-7.89038021109147));
#30195=CARTESIAN_POINT('Ctrl Pts',(97.5366097107556,0.478621813088558,-7.88997447766068));
#30196=CARTESIAN_POINT('Ctrl Pts',(97.5197690095781,0.515966438396092,-7.88725304740198));
#30197=CARTESIAN_POINT('Ctrl Pts',(97.5040170461905,0.547124747641917,-7.88501095298144));
#30198=CARTESIAN_POINT('Ctrl Pts',(97.4422110397586,0.656968198972049,-7.87704906693644));
#30199=CARTESIAN_POINT('Ctrl Pts',(97.3884507087036,0.730940934143778,-7.87155206831638));
#30200=CARTESIAN_POINT('Ctrl Pts',(97.3089018822944,0.817292297682451,-7.86412814048908));
#30201=CARTESIAN_POINT('Ctrl Pts',(97.2904678529663,0.836006206917915,-7.86244966789188));
#30202=CARTESIAN_POINT('Ctrl Pts',(97.2622801296232,0.862770042867849,-7.85992857271642));
#30203=CARTESIAN_POINT('Ctrl Pts',(97.2529970444156,0.871304936576174,-7.85910519891827));
#30204=CARTESIAN_POINT('Ctrl Pts',(97.2378989691732,0.884745225689368,-7.8577756137069));
#30205=CARTESIAN_POINT('Ctrl Pts',(97.2321702316626,0.889746334120657,-7.85727326266728));
#30206=CARTESIAN_POINT('Ctrl Pts',(97.221211058643,0.899128080513568,-7.85631598703616));
#30207=CARTESIAN_POINT('Ctrl Pts',(97.2159901884433,0.903519446784354,-7.85586151772605));
#30208=CARTESIAN_POINT('Ctrl Pts',(97.2106885287038,0.907900685006797,-7.85540148842156));
#30209=CARTESIAN_POINT('Ctrl Pts',(97.2106455029646,0.907936235897516,-7.8553977551405));
#30210=CARTESIAN_POINT('Ctrl Pts',(97.2105558175339,0.908010329579029,-7.85538997346799));
#30211=CARTESIAN_POINT('Ctrl Pts',(97.2105091571299,0.908048872053512,-7.8553859250318));
#30212=CARTESIAN_POINT('Ctrl Pts',(97.2104117953303,0.90812928232232,-7.85537747778543));
#30213=CARTESIAN_POINT('Ctrl Pts',(97.2103610934887,0.908171149393383,-7.85537307895715));
#30214=CARTESIAN_POINT('Ctrl Pts',(97.2102551803057,0.908258592340649,-7.85536389034314));
#30215=CARTESIAN_POINT('Ctrl Pts',(97.2101999683967,0.908304167361049,-7.85535910053311));
#30216=CARTESIAN_POINT('Ctrl Pts',(97.2061063390936,0.911682652084415,-7.8550039768909));
#30217=CARTESIAN_POINT('Ctrl Pts',(97.2020458007649,0.914988551609131,-7.8546525760926));
#30218=CARTESIAN_POINT('Ctrl Pts',(97.1932846170847,0.922024868644866,-7.85389611600036));
#30219=CARTESIAN_POINT('Ctrl Pts',(97.1885772516971,0.925746642474763,-7.85349072866336));
#30220=CARTESIAN_POINT('Ctrl Pts',(97.1760998555832,0.935457580731893,-7.85241884138715));
#30221=CARTESIAN_POINT('Ctrl Pts',(97.1682832163167,0.941385810963418,-7.85174999845019));
#30222=CARTESIAN_POINT('Ctrl Pts',(97.1338660660346,0.966817192450627,-7.84881577862293));
#30223=CARTESIAN_POINT('Ctrl Pts',(97.1065292658109,0.98529396814419,-7.84651216950563));
#30224=CARTESIAN_POINT('Ctrl Pts',(96.9918347383923,1.05598859796899,-7.836948411576));
#30225=CARTESIAN_POINT('Ctrl Pts',(96.8986633753071,1.09792529657191,-7.82936131017581));
#30226=CARTESIAN_POINT('Ctrl Pts',(96.7806017521716,1.13361576901222,-7.82044134353543));
#30227=CARTESIAN_POINT('Ctrl Pts',(96.7597471231105,1.13929886813824,-7.81889264964768));
#30228=CARTESIAN_POINT('Ctrl Pts',(96.7255741137713,1.14760814458412,-7.81641003465013));
#30229=CARTESIAN_POINT('Ctrl Pts',(96.7123464609499,1.15058360964401,-7.81546232043411));
#30230=CARTESIAN_POINT('Ctrl Pts',(96.6943978749204,1.15429662326251,-7.81419680258446));
#30231=CARTESIAN_POINT('Ctrl Pts',(96.6897201245905,1.15523470560876,-7.81386884959797));
#30232=CARTESIAN_POINT('Ctrl Pts',(96.681908648989,1.15675191388651,-7.81332444525744));
#30233=CARTESIAN_POINT('Ctrl Pts',(96.678778086775,1.15734678336254,-7.81310713593988));
#30234=CARTESIAN_POINT('Ctrl Pts',(96.6728476068142,1.15844877380885,-7.81269716094467));
#30235=CARTESIAN_POINT('Ctrl Pts',(96.67004820822,1.15895846482445,-7.81250434883756));
#30236=CARTESIAN_POINT('Ctrl Pts',(96.6634161166412,1.16014116488754,-7.8120491777055));
#30237=CARTESIAN_POINT('Ctrl Pts',(96.6595818514943,1.16080533958989,-7.81178730673393));
#30238=CARTESIAN_POINT('Ctrl Pts',(96.6460368055927,1.16308253606897,-7.81086650454938));
#30239=CARTESIAN_POINT('Ctrl Pts',(96.6363088437271,1.16459285958177,-7.81021296366014));
#30240=CARTESIAN_POINT('Ctrl Pts',(96.5571348415205,1.1758703641614,-7.80494855049348));
#30241=CARTESIAN_POINT('Ctrl Pts',(96.4869523569598,1.17954019898972,-7.80061738570189));
#30242=CARTESIAN_POINT('Ctrl Pts',(96.3573388014611,1.17473550103533,-7.79259425294203));
#30243=CARTESIAN_POINT('Ctrl Pts',(96.2980822458911,1.16801875081837,-7.7889159212225));
#30244=CARTESIAN_POINT('Ctrl Pts',(96.2186095145754,1.15284409237539,-7.78376015977628));
#30245=CARTESIAN_POINT('Ctrl Pts',(96.1977428977383,1.14826822940311,-7.78238572714134));
#30246=CARTESIAN_POINT('Ctrl Pts',(96.1616851223464,1.1393267797889,-7.77996603116743));
#30247=CARTESIAN_POINT('Ctrl Pts',(96.1464357464839,1.13521805374715,-7.77892860056521));
#30248=CARTESIAN_POINT('Ctrl Pts',(96.1243503821836,1.1287884238588,-7.77740326998126));
#30249=CARTESIAN_POINT('Ctrl Pts',(96.1174453984027,1.12670922199922,-7.77692309221318));
#30250=CARTESIAN_POINT('Ctrl Pts',(96.1053246085734,1.12293770970135,-7.77607420382506));
#30251=CARTESIAN_POINT('Ctrl Pts',(96.1001006641551,1.12127212333614,-7.77570636529627));
#30252=CARTESIAN_POINT('Ctrl Pts',(96.0892351813118,1.11772403189962,-7.77493706397254));
#30253=CARTESIAN_POINT('Ctrl Pts',(96.0835959035028,1.11583515437995,-7.7745354029575));
#30254=CARTESIAN_POINT('Ctrl Pts',(96.0689257800281,1.11079749764821,-7.7734841463847));
#30255=CARTESIAN_POINT('Ctrl Pts',(96.0599187092887,1.10758133510916,-7.77283236868855));
#30256=CARTESIAN_POINT('Ctrl Pts',(96.0221448556305,1.09357236743689,-7.77007148455463));
#30257=CARTESIAN_POINT('Ctrl Pts',(95.9937692854553,1.08176660022033,-7.76792950014785));
#30258=CARTESIAN_POINT('Ctrl Pts',(95.9510389526017,1.06199420098715,-7.76459595846739));
#30259=CARTESIAN_POINT('Ctrl Pts',(95.9363398230804,1.05481676894557,-7.76342898525895));
#30260=CARTESIAN_POINT('Ctrl Pts',(95.9218015552896,1.04733928250123,-7.76225484780379));
#30261=CARTESIAN_POINT('Ctrl Pts',(95.9218016730721,1.04733934308044,-7.66392541087522));
#30262=CARTESIAN_POINT('Ctrl Pts',(95.923981392874,1.04846044093055,-7.66409230412672));
#30263=CARTESIAN_POINT('Ctrl Pts',(95.9261646025136,1.04957472918492,-7.66425876593663));
#30264=CARTESIAN_POINT('Ctrl Pts',(95.9317643886838,1.05241080267926,-7.6646839675234));
#30265=CARTESIAN_POINT('Ctrl Pts',(95.9351858978763,1.05412276754204,-7.6649420999066));
#30266=CARTESIAN_POINT('Ctrl Pts',(95.944051180343,1.05850466115847,-7.66560678627251));
#30267=CARTESIAN_POINT('Ctrl Pts',(95.9495074184012,1.0611493196062,-7.66601185632826));
#30268=CARTESIAN_POINT('Ctrl Pts',(95.9862798530973,1.07862365387436,-7.66871657412019));
#30269=CARTESIAN_POINT('Ctrl Pts',(96.018220186207,1.09210878084112,-7.67094365038082));
#30270=CARTESIAN_POINT('Ctrl Pts',(96.0771503032242,1.11397842592764,-7.67491543705369));
#30271=CARTESIAN_POINT('Ctrl Pts',(96.1039335913543,1.12283766412314,-7.67667138336449));
#30272=CARTESIAN_POINT('Ctrl Pts',(96.1770424663697,1.14414010667485,-7.68139279936664));
#30273=CARTESIAN_POINT('Ctrl Pts',(96.2238502174275,1.15472930241282,-7.68434131347457));
#30274=CARTESIAN_POINT('Ctrl Pts',(96.3238411505766,1.17101331010402,-7.69067649809304));
#30275=CARTESIAN_POINT('Ctrl Pts',(96.3770253976349,1.17600029435913,-7.69406862072802));
#30276=CARTESIAN_POINT('Ctrl Pts',(96.4411899657492,1.1776418308785,-7.6982871419761));
#30277=CARTESIAN_POINT('Ctrl Pts',(96.4520227688403,1.17776944700149,-7.69900349607877));
#30278=CARTESIAN_POINT('Ctrl Pts',(96.4690785456704,1.17773505944926,-7.70013858705303));
#30279=CARTESIAN_POINT('Ctrl Pts',(96.4753012878662,1.17767319065209,-7.70055423341445));
#30280=CARTESIAN_POINT('Ctrl Pts',(96.4869505466649,1.17746502665234,-7.70133530583461));
#30281=CARTESIAN_POINT('Ctrl Pts',(96.4923771303507,1.17733052305712,-7.70170035780464));
#30282=CARTESIAN_POINT('Ctrl Pts',(96.5045240580543,1.17694540726014,-7.70252028234999));
#30283=CARTESIAN_POINT('Ctrl Pts',(96.5112435305895,1.17667474018992,-7.70297576270701));
#30284=CARTESIAN_POINT('Ctrl Pts',(96.5283359003427,1.17583956405077,-7.70413940511488));
#30285=CARTESIAN_POINT('Ctrl Pts',(96.5387041420007,1.17519534330095,-7.70484999732243));
#30286=CARTESIAN_POINT('Ctrl Pts',(96.6243336689131,1.16873665653123,-7.71075922872014));
#30287=CARTESIAN_POINT('Ctrl Pts',(96.698870871402,1.15583711950869,-7.71617964687596));
#30288=CARTESIAN_POINT('Ctrl Pts',(96.8274458155472,1.12061534841979,-7.7259317615011));
#30289=CARTESIAN_POINT('Ctrl Pts',(96.882041191241,1.10123984115792,-7.73020463661731));
#30290=CARTESIAN_POINT('Ctrl Pts',(96.9537164314812,1.06968796768564,-7.73585944498116));
#30291=CARTESIAN_POINT('Ctrl Pts',(96.9722236550819,1.06095857194982,-7.73732331876027));
#30292=CARTESIAN_POINT('Ctrl Pts',(97.0021344371959,1.04588548132331,-7.73968541400261));
#30293=CARTESIAN_POINT('Ctrl Pts',(97.0136762307433,1.03982688791344,-7.74059592323309));
#30294=CARTESIAN_POINT('Ctrl Pts',(97.0292399282159,1.0313245719447,-7.74182007589355));
#30295=CARTESIAN_POINT('Ctrl Pts',(97.0333507758058,1.02904679804116,-7.74214306064631));
#30296=CARTESIAN_POINT('Ctrl Pts',(97.0402128531085,1.02519073401116,-7.74268147839931));
#30297=CARTESIAN_POINT('Ctrl Pts',(97.0429715059819,1.02362584646643,-7.74289773121208));
#30298=CARTESIAN_POINT('Ctrl Pts',(97.0482035591064,1.02062988484212,-7.74330744919929));
#30299=CARTESIAN_POINT('Ctrl Pts',(97.0506781178956,1.01920092746069,-7.74350104965702));
#30300=CARTESIAN_POINT('Ctrl Pts',(97.0565522982165,1.01578025856189,-7.74396025449424));
#30301=CARTESIAN_POINT('Ctrl Pts',(97.0599472012252,1.01378044989703,-7.74422534970025));
#30302=CARTESIAN_POINT('Ctrl Pts',(97.0719456412569,1.00663127700011,-7.74516144565428));
#30303=CARTESIAN_POINT('Ctrl Pts',(97.0804936776347,1.00138895061651,-7.74582685074794));
#30304=CARTESIAN_POINT('Ctrl Pts',(97.1395304446723,0.964137153080263,-7.75041955431513));
#30305=CARTESIAN_POINT('Ctrl Pts',(97.1875914875447,0.928429196611734,-7.75414603620714));
#30306=CARTESIAN_POINT('Ctrl Pts',(97.2833176830194,0.845294428741272,-7.76200156674863));
#30307=CARTESIAN_POINT('Ctrl Pts',(97.3300547112697,0.797134767390442,-7.76611449751116));
#30308=CARTESIAN_POINT('Ctrl Pts',(97.3941867288306,0.718657966222643,-7.77255740664575));
#30309=CARTESIAN_POINT('Ctrl Pts',(97.4147534228625,0.691114645895845,-7.77477522796733));
#30310=CARTESIAN_POINT('Ctrl Pts',(97.4394811072968,0.654786760845278,-7.77767124484812));
#30311=CARTESIAN_POINT('Ctrl Pts',(97.4447796286538,0.646794490101691,-7.77830660638022));
#30312=CARTESIAN_POINT('Ctrl Pts',(97.4532080207281,0.633737686267731,-7.77934221371402));
#30313=CARTESIAN_POINT('Ctrl Pts',(97.4563981888518,0.628712448665733,-7.77974023313545));
#30314=CARTESIAN_POINT('Ctrl Pts',(97.4624523569862,0.619014054877953,-7.78050743141556));
#30315=CARTESIAN_POINT('Ctrl Pts',(97.4653221036924,0.614344654616672,-7.78087638828942));
#30316=CARTESIAN_POINT('Ctrl Pts',(97.4718222383855,0.603600809592548,-7.78172446047449));
#30317=CARTESIAN_POINT('Ctrl Pts',(97.4754306490261,0.597513383611834,-7.7822043509442));
#30318=CARTESIAN_POINT('Ctrl Pts',(97.4867553406637,0.578009916324859,-7.78374012593532));
#30319=CARTESIAN_POINT('Ctrl Pts',(97.4942618576207,0.564474608690195,-7.78480336821043));
#30320=CARTESIAN_POINT('Ctrl Pts',(97.5385074194192,0.480849366789827,-7.79135988224784));
#30321=CARTESIAN_POINT('Ctrl Pts',(97.5683654796724,0.40736333352814,-7.79708871814974));
#30322=CARTESIAN_POINT('Ctrl Pts',(97.6059753545198,0.279125989572298,-7.80688944562775));
#30323=CARTESIAN_POINT('Ctrl Pts',(97.6176700059914,0.22579363957247,-7.81090600405515));
#30324=CARTESIAN_POINT('Ctrl Pts',(97.6280210618544,0.155609559437917,-7.81599592808213));
#30325=CARTESIAN_POINT('Ctrl Pts',(97.6300756242715,0.139329114946114,-7.81716285249217));
#30326=CARTESIAN_POINT('Ctrl Pts',(97.6329475763833,0.111982270537919,-7.81909455767893));
#30327=CARTESIAN_POINT('Ctrl Pts',(97.6339499796347,0.100937989160873,-7.81986696237905));
#30328=CARTESIAN_POINT('Ctrl Pts',(97.6351330921114,0.0854803105500236,
-7.82093575569451));
#30329=CARTESIAN_POINT('Ctrl Pts',(97.6354451638727,0.0810779633869377,
-7.82123875898059));
#30330=CARTESIAN_POINT('Ctrl Pts',(97.6359353436993,0.0735645232211535,
-7.82175340623233));
#30331=CARTESIAN_POINT('Ctrl Pts',(97.6361258629712,0.0704543133286296,
-7.82196571891625));
#30332=CARTESIAN_POINT('Ctrl Pts',(97.6364710750203,0.064426864369362,-7.82237572313969));
#30333=CARTESIAN_POINT('Ctrl Pts',(97.6366272600685,0.0615097779286169,
-7.8225735003458));
#30334=CARTESIAN_POINT('Ctrl Pts',(97.6370231344539,0.0535622265020901,
-7.82311064072549));
#30335=CARTESIAN_POINT('Ctrl Pts',(97.6372414179168,0.0485306844431066,
-7.8234488461278));
#30336=CARTESIAN_POINT('Ctrl Pts',(97.637957227386,0.0291625846617524,-7.82474411053741));
#30337=CARTESIAN_POINT('Ctrl Pts',(97.6382251109924,0.0148181076439342,
-7.82568950209409));
#30338=CARTESIAN_POINT('Ctrl Pts',(97.6382404784862,-0.0235631149471175,
-7.82819039740362));
#30339=CARTESIAN_POINT('Ctrl Pts',(97.6375143748193,-0.0475940345359999,
-7.82972620866432));
#30340=CARTESIAN_POINT('Ctrl Pts',(97.6327832013468,-0.125287048562484,
-7.83464160347656));
#30341=CARTESIAN_POINT('Ctrl Pts',(97.6258373578872,-0.178701947925456,
-7.83794595302156));
#30342=CARTESIAN_POINT('Ctrl Pts',(97.6007545329808,-0.303844985852653,
-7.84585154403032));
#30343=CARTESIAN_POINT('Ctrl Pts',(97.5794736190406,-0.374698412701719,
-7.85046793662601));
#30344=CARTESIAN_POINT('Ctrl Pts',(97.5477790168846,-0.452754685395738,
-7.85599649562586));
#30345=CARTESIAN_POINT('Ctrl Pts',(97.5437261244805,-0.462367572432125,
-7.85668510301689));
#30346=CARTESIAN_POINT('Ctrl Pts',(97.5368461327927,-0.478098796804973,
-7.85782547647642));
#30347=CARTESIAN_POINT('Ctrl Pts',(97.5340932087621,-0.48424908973175,-7.85827475498668));
#30348=CARTESIAN_POINT('Ctrl Pts',(97.5290271529877,-0.495311568997524,
-7.85908926490367));
#30349=CARTESIAN_POINT('Ctrl Pts',(97.5267325255483,-0.50023206040703,-7.85945386019599));
#30350=CARTESIAN_POINT('Ctrl Pts',(97.521739050489,-0.510749363739677,-7.86023822072937));
#30351=CARTESIAN_POINT('Ctrl Pts',(97.5190297785611,-0.516341014654776,
-7.86065833417033));
#30352=CARTESIAN_POINT('Ctrl Pts',(97.5114954458012,-0.531582533612204,
-7.86181212282035));
#30353=CARTESIAN_POINT('Ctrl Pts',(97.5065819321537,-0.541187751284302,
-7.8625488243611));
#30354=CARTESIAN_POINT('Ctrl Pts',(97.4770272598079,-0.597056186318608,
-7.86689159600093));
#30355=CARTESIAN_POINT('Ctrl Pts',(97.4494551542298,-0.641693939673995,
-7.87059978908286));
#30356=CARTESIAN_POINT('Ctrl Pts',(97.3736237896031,-0.747907263960275,
-7.88002573071777));
#30357=CARTESIAN_POINT('Ctrl Pts',(97.3220345654406,-0.806795777735824,
-7.88582339340791));
#30358=CARTESIAN_POINT('Ctrl Pts',(97.2402882546581,-0.883255588928051,
-7.8939333980572));
#30359=CARTESIAN_POINT('Ctrl Pts',(97.2145904897262,-0.905295055001402,
-7.89635247591214));
#30360=CARTESIAN_POINT('Ctrl Pts',(97.1832346826081,-0.929923902702669,
-7.8991234977911));
#30361=CARTESIAN_POINT('Ctrl Pts',(97.1784639431013,-0.933612257977767,
-7.89954039139932));
#30362=CARTESIAN_POINT('Ctrl Pts',(97.170628310543,-0.939574557225028,-7.90021718085949));
#30363=CARTESIAN_POINT('Ctrl Pts',(97.1675803930718,-0.94187047990306,-7.90047850593111));
#30364=CARTESIAN_POINT('Ctrl Pts',(97.162082953424,-0.945969842204705,-7.90094630844021));
#30365=CARTESIAN_POINT('Ctrl Pts',(97.1596375638603,-0.947778636336309,
-7.90115314436538));
#30366=CARTESIAN_POINT('Ctrl Pts',(97.1542258818935,-0.951749180392414,
-7.90160811688304));
#30367=CARTESIAN_POINT('Ctrl Pts',(97.1512564779503,-0.953906548782637,
-7.9018559572103));
#30368=CARTESIAN_POINT('Ctrl Pts',(97.1425945762482,-0.960138044451458,
-7.90257384813418));
#30369=CARTESIAN_POINT('Ctrl Pts',(97.1368756616,-0.964175431919296,-7.90304150269117));
#30370=CARTESIAN_POINT('Ctrl Pts',(97.0861931324487,-0.999282924268112,
-7.90713390707167));
#30371=CARTESIAN_POINT('Ctrl Pts',(97.0391470314475,-1.02724354803441,-7.91057601267292));
#30372=CARTESIAN_POINT('Ctrl Pts',(96.9102390934021,-1.09217829912979,-7.91955466080026));
#30373=CARTESIAN_POINT('Ctrl Pts',(96.8258164937886,-1.12323857126121,-7.92501210942893));
#30374=CARTESIAN_POINT('Ctrl Pts',(96.7157084209652,-1.15000578251797,-7.93230372389437));
#30375=CARTESIAN_POINT('Ctrl Pts',(96.6925665164683,-1.15489849320668,-7.93384366748186));
#30376=CARTESIAN_POINT('Ctrl Pts',(96.6607406382336,-1.1606320079399,-7.93597932178633));
#30377=CARTESIAN_POINT('Ctrl Pts',(96.6521704588125,-1.16207819276933,-7.93655615219706));
#30378=CARTESIAN_POINT('Ctrl Pts',(96.6384647125157,-1.1642352476759,-7.9374817464514));
#30379=CARTESIAN_POINT('Ctrl Pts',(96.6333389866055,-1.16500730872376,-7.93782859379942));
#30380=CARTESIAN_POINT('Ctrl Pts',(96.6227658495484,-1.16652857157378,-7.9385455581791));
#30381=CARTESIAN_POINT('Ctrl Pts',(96.6173179630493,-1.16727350972342,-7.93891579873738));
#30382=CARTESIAN_POINT('Ctrl Pts',(96.6046073473807,-1.1689209572902,-7.93978162148022));
#30383=CARTESIAN_POINT('Ctrl Pts',(96.5973410917316,-1.16979396486757,-7.94027810737867));
#30384=CARTESIAN_POINT('Ctrl Pts',(96.5737710898679,-1.17240318486601,-7.94189377898199));
#30385=CARTESIAN_POINT('Ctrl Pts',(96.5574397270239,-1.17386661608748,-7.94302131999425));
#30386=CARTESIAN_POINT('Ctrl Pts',(96.5187024889696,-1.17652394634718,-7.9457161908674));
#30387=CARTESIAN_POINT('Ctrl Pts',(96.4962832048433,-1.17741939404442,-7.94729202062163));
#30388=CARTESIAN_POINT('Ctrl Pts',(96.4087629222459,-1.17841317164145,-7.95350675958483));
#30389=CARTESIAN_POINT('Ctrl Pts',(96.3437299466168,-1.17375458646104,-7.95826892214971));
#30390=CARTESIAN_POINT('Ctrl Pts',(96.2773912255896,-1.1634334708004,-7.96319621355617));
#30391=CARTESIAN_POINT('Ctrl Pts',(96.2753608873686,-1.16311214015841,-7.96334707517624));
#30392=CARTESIAN_POINT('Ctrl Pts',(96.2138408374906,-1.15321052920601,-7.96791989695895));
#30393=CARTESIAN_POINT('Ctrl Pts',(96.155166685269,-1.13908319271317,-7.9723333659338));
#30394=CARTESIAN_POINT('Ctrl Pts',(96.0882896217135,-1.11743866191224,-7.97726264357549));
#30395=CARTESIAN_POINT('Ctrl Pts',(96.0787918472646,-1.11423022462396,-7.9779601054315));
#30396=CARTESIAN_POINT('Ctrl Pts',(96.0656198009241,-1.10959238300891,-7.97892267819898));
#30397=CARTESIAN_POINT('Ctrl Pts',(96.0619103105781,-1.1082653247258,-7.97919323199774));
#30398=CARTESIAN_POINT('Ctrl Pts',(96.0555219677818,-1.10594369208253,-7.97965817941775));
#30399=CARTESIAN_POINT('Ctrl Pts',(96.052839976488,-1.10495794693614,-7.97985307395861));
#30400=CARTESIAN_POINT('Ctrl Pts',(96.0471886032513,-1.10285745155562,-7.98026306879484));
#30401=CARTESIAN_POINT('Ctrl Pts',(96.0442200884078,-1.10174044941557,-7.98047802873518));
#30402=CARTESIAN_POINT('Ctrl Pts',(96.0368637933656,-1.09893842355254,-7.98100981441349));
#30403=CARTESIAN_POINT('Ctrl Pts',(96.0324814597836,-1.09723907713851,-7.98132580858024));
#30404=CARTESIAN_POINT('Ctrl Pts',(96.0159818528589,-1.09072709730348,-7.98251291855449));
#30405=CARTESIAN_POINT('Ctrl Pts',(96.0039340740785,-1.08573939457892,-7.98337438319121));
#30406=CARTESIAN_POINT('Ctrl Pts',(95.9731932581564,-1.07241067677955,-7.98556480544839));
#30407=CARTESIAN_POINT('Ctrl Pts',(95.9546297974243,-1.06378036505403,-7.98688015028496));
#30408=CARTESIAN_POINT('Ctrl Pts',(95.8845037051856,-1.02892701597441,-7.9918552458824));
#30409=CARTESIAN_POINT('Ctrl Pts',(95.8346714612259,-0.999401760449134,
-7.99540683162181));
#30410=CARTESIAN_POINT('Ctrl Pts',(95.7252821882188,-0.923186988955485,
-8.00366198635098));
#30411=CARTESIAN_POINT('Ctrl Pts',(95.6676555304831,-0.874195105200194,
-8.00837561357045));
#30412=CARTESIAN_POINT('Ctrl Pts',(95.6078818816454,-0.812574807312045,
-8.01400988825543));
#30413=CARTESIAN_POINT('Ctrl Pts',(95.6007477014007,-0.805022806449267,
-8.01469567892419));
#30414=CARTESIAN_POINT('Ctrl Pts',(95.5891613991801,-0.792428249643242,
-8.01583234665886));
#30415=CARTESIAN_POINT('Ctrl Pts',(95.5846508168138,-0.787440070819168,
-8.01628076441739));
#30416=CARTESIAN_POINT('Ctrl Pts',(95.5765771155062,-0.778356307117406,
-8.01709435359027));
#30417=CARTESIAN_POINT('Ctrl Pts',(95.5729990976729,-0.774274169509924,
-8.0174588954474));
#30418=CARTESIAN_POINT('Ctrl Pts',(95.565380121745,-0.765459532008716,-8.01824385330516));
#30419=CARTESIAN_POINT('Ctrl Pts',(95.5613482118395,-0.760719465040718,
-8.01866462253414));
#30420=CARTESIAN_POINT('Ctrl Pts',(95.5504010775743,-0.747640980844114,
-8.01982207874377));
#30421=CARTESIAN_POINT('Ctrl Pts',(95.5435631797032,-0.739238932524814,
-8.02056182435269));
#30422=CARTESIAN_POINT('Ctrl Pts',(95.5037412679311,-0.688905224362348,
-8.02497215138119));
#30423=CARTESIAN_POINT('Ctrl Pts',(95.4735260474554,-0.644871905957608,
-8.02874871213888));
#30424=CARTESIAN_POINT('Ctrl Pts',(95.4220126954558,-0.557654685753922,
-8.03606990122398));
#30425=CARTESIAN_POINT('Ctrl Pts',(95.4001694423836,-0.514911776524459,
-8.0395920312369));
#30426=CARTESIAN_POINT('Ctrl Pts',(95.3697136831079,-0.445103973447315,
-8.04517995291811));
#30427=CARTESIAN_POINT('Ctrl Pts',(95.3593658798564,-0.418851374801232,
-8.04724592331202));
#30428=CARTESIAN_POINT('Ctrl Pts',(95.3384308940089,-0.359582001908917,
-8.05180335635843));
#30429=CARTESIAN_POINT('Ctrl Pts',(95.3283373680479,-0.326415302427263,
-8.05428235473442));
#30430=CARTESIAN_POINT('Ctrl Pts',(95.3182127567085,-0.286975955233544,
-8.05711249804184));
#30431=CARTESIAN_POINT('Ctrl Pts',(95.3167504999801,-0.281091596912665,
-8.05753171356749));
#30432=CARTESIAN_POINT('Ctrl Pts',(95.3144397687624,-0.271476170337992,
-8.05821150108607));
#30433=CARTESIAN_POINT('Ctrl Pts',(95.3135639393123,-0.267751884754611,
-8.05847352285367));
#30434=CARTESIAN_POINT('Ctrl Pts',(95.3120243031907,-0.261058705927105,
-8.05894205227142));
#30435=CARTESIAN_POINT('Ctrl Pts',(95.3113538388309,-0.258091457737228,
-8.05914892367343));
#30436=CARTESIAN_POINT('Ctrl Pts',(95.309901671687,-0.251546805998029,-8.05960335702116));
#30437=CARTESIAN_POINT('Ctrl Pts',(95.3091251511017,-0.247968337789584,
-8.05985062733141));
#30438=CARTESIAN_POINT('Ctrl Pts',(95.3069213459685,-0.237578889177517,
-8.06056519979769));
#30439=CARTESIAN_POINT('Ctrl Pts',(95.305537690475,-0.230758665475385,-8.0610301397131));
#30440=CARTESIAN_POINT('Ctrl Pts',(95.2942875463215,-0.172667411780121,
-8.06495818342253));
#30441=CARTESIAN_POINT('Ctrl Pts',(95.2877787524103,-0.120797812134772,
-8.06825470066511));
#30442=CARTESIAN_POINT('Ctrl Pts',(95.2798825823654,0.0144152596926865,
-8.07669152404167));
#30443=CARTESIAN_POINT('Ctrl Pts',(95.2838495873202,0.0977678340915831,
-8.08175555754729));
#30444=CARTESIAN_POINT('Ctrl Pts',(95.3012726004469,0.210424564021685,-8.08902674324303));
#30445=CARTESIAN_POINT('Ctrl Pts',(95.3071673398022,0.240644875148239,-8.09101807885458));
#30446=CARTESIAN_POINT('Ctrl Pts',(95.316437071813,0.279911130639541,-8.09367700250467));
#30447=CARTESIAN_POINT('Ctrl Pts',(95.3187490843432,0.289197120202337,-8.09431108635793));
#30448=CARTESIAN_POINT('Ctrl Pts',(95.3226812400735,0.304207598564376,-8.09534512574232));
#30449=CARTESIAN_POINT('Ctrl Pts',(95.3242320828442,0.309949919541177,-8.09574286759459));
#30450=CARTESIAN_POINT('Ctrl Pts',(95.3272957451871,0.320961693719857,-8.09650988387517));
#30451=CARTESIAN_POINT('Ctrl Pts',(95.3288019944376,0.326232826421337,-8.09687893890141));
#30452=CARTESIAN_POINT('Ctrl Pts',(95.3323736130768,0.33840929047697,-8.09773596435205));
#30453=CARTESIAN_POINT('Ctrl Pts',(95.3344656624178,0.345306501001488,-8.09822478253417));
#30454=CARTESIAN_POINT('Ctrl Pts',(95.3413376921524,0.367235950547476,-8.0997899747078));
#30455=CARTESIAN_POINT('Ctrl Pts',(95.3463562418367,0.382191009621324,-8.10087399233418));
#30456=CARTESIAN_POINT('Ctrl Pts',(95.3588632736023,0.417119191439609,-8.10344631681161));
#30457=CARTESIAN_POINT('Ctrl Pts',(95.3665968033818,0.43699805579233,-8.10494211851914));
#30458=CARTESIAN_POINT('Ctrl Pts',(95.3978969844965,0.511408642158896,-8.11066317469452));
#30459=CARTESIAN_POINT('Ctrl Pts',(95.425035493879,0.56433568359023,-8.11499100548655));
#30460=CARTESIAN_POINT('Ctrl Pts',(95.4927894191806,0.674995981601999,-8.12450980863772));
#30461=CARTESIAN_POINT('Ctrl Pts',(95.5348399948096,0.731598988080648,-8.12969542746935));
#30462=CARTESIAN_POINT('Ctrl Pts',(95.5882422964497,0.791448966555949,-8.13531737553614));
#30463=CARTESIAN_POINT('Ctrl Pts',(95.5948801799698,0.798703360492994,-8.13600119577185));
#30464=CARTESIAN_POINT('Ctrl Pts',(95.6042695696886,0.808710245520468,-8.13694681263806));
#30465=CARTESIAN_POINT('Ctrl Pts',(95.6069448196807,0.811533279844901,-8.13721384481675));
#30466=CARTESIAN_POINT('Ctrl Pts',(95.6116009832352,0.816398161134206,-8.13767439646127));
#30467=CARTESIAN_POINT('Ctrl Pts',(95.6135753805651,0.818446157285428,-8.13786839545716));
#30468=CARTESIAN_POINT('Ctrl Pts',(95.6177772947821,0.82277321799582,-8.13827849373416));
#30469=CARTESIAN_POINT('Ctrl Pts',(95.6200066818052,0.825050437114664,-8.13849444208905));
#30470=CARTESIAN_POINT('Ctrl Pts',(95.6255980343187,0.830715571304896,-8.13903206510085));
#30471=CARTESIAN_POINT('Ctrl Pts',(95.6289714460034,0.834092195153589,-8.13935286776616));
#30472=CARTESIAN_POINT('Ctrl Pts',(95.6420173842216,0.84699274662755,-8.14058035559939));
#30473=CARTESIAN_POINT('Ctrl Pts',(95.6518342031193,0.856370129662178,-8.14147652344846));
#30474=CARTESIAN_POINT('Ctrl Pts',(95.6777227524703,0.88025756435866,-8.14377672248058));
#30475=CARTESIAN_POINT('Ctrl Pts',(95.6940368270737,0.894498349035152,-8.1451653624917));
#30476=CARTESIAN_POINT('Ctrl Pts',(95.7759368057593,0.962103074910108,-8.15189801471611));
#30477=CARTESIAN_POINT('Ctrl Pts',(95.8467046785975,1.00871463130525,-8.15700823768759));
#30478=CARTESIAN_POINT('Ctrl Pts',(95.9218018246467,1.04733942103997,-8.16230712347374));
#30479=CARTESIAN_POINT('Origin',(96.460480949577,-7.19464945638997E-16,
0.924367114736168));
#30480=CARTESIAN_POINT('',(95.9218016730721,1.04733934308043,-8.76046578184569));
#30481=CARTESIAN_POINT('',(95.921801762405,1.04733938902714,-8.66210246100831));
#30482=CARTESIAN_POINT('',(95.9218016730721,1.04733934308042,0.924367114736168));
#30483=CARTESIAN_POINT('Ctrl Pts',(95.9218016730721,1.04733934308043,-8.76046578184569));
#30484=CARTESIAN_POINT('Ctrl Pts',(95.9211842780576,1.04702179757625,-8.76041879885222));
#30485=CARTESIAN_POINT('Ctrl Pts',(95.9205671622309,1.04670370532963,-8.76037184943281));
#30486=CARTESIAN_POINT('Ctrl Pts',(95.9165307298097,1.04461860740334,-8.76006484091161));
#30487=CARTESIAN_POINT('Ctrl Pts',(95.913119753472,1.04283536502668,-8.75980577226046));
#30488=CARTESIAN_POINT('Ctrl Pts',(95.9013312091185,1.03659859431538,-8.75891147927471));
#30489=CARTESIAN_POINT('Ctrl Pts',(95.8929984894525,1.03206043884117,-8.75828121998423));
#30490=CARTESIAN_POINT('Ctrl Pts',(95.8181144841698,0.990095988105696,-8.75262590390221));
#30491=CARTESIAN_POINT('Ctrl Pts',(95.7552852822633,0.946375818399088,-8.74793572478132));
#30492=CARTESIAN_POINT('Ctrl Pts',(95.6623524818714,0.86727796028939,-8.74038626992124));
#30493=CARTESIAN_POINT('Ctrl Pts',(95.6293319022418,0.835685977619807,-8.73755738925862));
#30494=CARTESIAN_POINT('Ctrl Pts',(95.5715688439873,0.773603423845097,-8.73219260237199));
#30495=CARTESIAN_POINT('Ctrl Pts',(95.5463551035912,0.74363998872754,-8.72967626963997));
#30496=CARTESIAN_POINT('Ctrl Pts',(95.5166424333765,0.704530742097177,-8.72644233250801));
#30497=CARTESIAN_POINT('Ctrl Pts',(95.5107050311602,0.696505854939194,-8.72578134450696));
#30498=CARTESIAN_POINT('Ctrl Pts',(95.5013409497965,0.683507122522943,-8.72471424646144));
#30499=CARTESIAN_POINT('Ctrl Pts',(95.4978491887168,0.678580589470841,-8.7243106234197));
#30500=CARTESIAN_POINT('Ctrl Pts',(95.4912736773382,0.669150294930611,-8.72353942360661));
#30501=CARTESIAN_POINT('Ctrl Pts',(95.4881830407352,0.664651509069659,-8.72317211916705));
#30502=CARTESIAN_POINT('Ctrl Pts',(95.481187067939,0.654314822800542,-8.72232945364582));
#30503=CARTESIAN_POINT('Ctrl Pts',(95.4773024916593,0.648463191044452,-8.72185333684939));
#30504=CARTESIAN_POINT('Ctrl Pts',(95.46540918291,0.630194852233414,-8.72036954512109));
#30505=CARTESIAN_POINT('Ctrl Pts',(95.4575818680362,0.617662343407645,-8.7193553059623));
#30506=CARTESIAN_POINT('Ctrl Pts',(95.4025190146929,0.525692724165228,-8.71193540965759));
#30507=CARTESIAN_POINT('Ctrl Pts',(95.3645522209929,0.441101013695717,-8.70519592273347));
#30508=CARTESIAN_POINT('Ctrl Pts',(95.3181402789188,0.293354257713818,-8.69383120564699));
#30509=CARTESIAN_POINT('Ctrl Pts',(95.3041862876573,0.232343001431131,-8.68925602295264));
#30510=CARTESIAN_POINT('Ctrl Pts',(95.2939073356206,0.162090760520949,-8.68429738906492));
#30511=CARTESIAN_POINT('Ctrl Pts',(95.2927670840496,0.153661153550667,-8.68370747849889));
#30512=CARTESIAN_POINT('Ctrl Pts',(95.2912288159413,0.141280799914897,-8.68284923397529));
#30513=CARTESIAN_POINT('Ctrl Pts',(95.29075931823,0.137339443536495,-8.68257721416311));
#30514=CARTESIAN_POINT('Ctrl Pts',(95.2899671444323,0.130390352626268,-8.68209982383404));
#30515=CARTESIAN_POINT('Ctrl Pts',(95.2896361196581,0.127383661070721,-8.68189400279479));
#30516=CARTESIAN_POINT('Ctrl Pts',(95.2889425785984,0.120853036245441,-8.68144856056237));
#30517=CARTESIAN_POINT('Ctrl Pts',(95.2885843746164,0.117328723975617,-8.68120917777893));
#30518=CARTESIAN_POINT('Ctrl Pts',(95.2876404947567,0.107606179763843,-8.68055142589863));
#30519=CARTESIAN_POINT('Ctrl Pts',(95.2870880453752,0.101404728403375,-8.68013483393737));
#30520=CARTESIAN_POINT('Ctrl Pts',(95.2843838722493,0.0680596538361094,
-8.67790926236002));
#30521=CARTESIAN_POINT('Ctrl Pts',(95.2831245786215,0.0408496400342891,
-8.67614445703815));
#30522=CARTESIAN_POINT('Ctrl Pts',(95.2815696192174,-0.0936205332582201,
-8.66756895531445));
#30523=CARTESIAN_POINT('Ctrl Pts',(95.2949818918721,-0.200529130520746,
-8.66116360281169));
#30524=CARTESIAN_POINT('Ctrl Pts',(95.3283571361453,-0.325382365659745,
-8.65293680430483));
#30525=CARTESIAN_POINT('Ctrl Pts',(95.3346252602013,-0.346448973402391,
-8.65152396327156));
#30526=CARTESIAN_POINT('Ctrl Pts',(95.3465126448089,-0.382661965703558,
-8.64904286503726));
#30527=CARTESIAN_POINT('Ctrl Pts',(95.3518610343859,-0.397891199686078,
-8.6479830132691));
#30528=CARTESIAN_POINT('Ctrl Pts',(95.3600711271452,-0.419816853374509,
-8.64643078797672));
#30529=CARTESIAN_POINT('Ctrl Pts',(95.3626847787278,-0.426604654199901,
-8.64594653449259));
#30530=CARTESIAN_POINT('Ctrl Pts',(95.3673820050107,-0.438474542000598,
-8.64509297021063));
#30531=CARTESIAN_POINT('Ctrl Pts',(95.3694385899896,-0.443567125065877,
-8.64472456303101));
#30532=CARTESIAN_POINT('Ctrl Pts',(95.3737859137832,-0.454118939286172,
-8.64395654959733));
#30533=CARTESIAN_POINT('Ctrl Pts',(95.3760823431109,-0.459575643312554,
-8.64355676161306));
#30534=CARTESIAN_POINT('Ctrl Pts',(95.382146985966,-0.473687701068225,-8.64251588640876));
#30535=CARTESIAN_POINT('Ctrl Pts',(95.3859782342551,-0.482315333563207,
-8.64187269636415));
#30536=CARTESIAN_POINT('Ctrl Pts',(95.4022214265444,-0.51773924100463,-8.63920285196703));
#30537=CARTESIAN_POINT('Ctrl Pts',(95.415534380345,-0.544108022986234,-8.63714599639503));
#30538=CARTESIAN_POINT('Ctrl Pts',(95.4755117863384,-0.65256758896969,-8.62838312584974));
#30539=CARTESIAN_POINT('Ctrl Pts',(95.5309659408508,-0.729387289474188,
-8.62138758773002));
#30540=CARTESIAN_POINT('Ctrl Pts',(95.6147579853023,-0.820181837635842,
-8.6123813906755));
#30541=CARTESIAN_POINT('Ctrl Pts',(95.6353273565597,-0.840872971823087,
-8.61027283586771));
#30542=CARTESIAN_POINT('Ctrl Pts',(95.6648514106568,-0.868443881140002,
-8.60740581393572));
#30543=CARTESIAN_POINT('Ctrl Pts',(95.6731673572244,-0.875989991812716,
-8.60661476688659));
#30544=CARTESIAN_POINT('Ctrl Pts',(95.6878278629858,-0.888915869348591,
-8.60525039694788));
#30545=CARTESIAN_POINT('Ctrl Pts',(95.6941237391187,-0.894349400822565,
-8.60467387062112));
#30546=CARTESIAN_POINT('Ctrl Pts',(95.7034814761785,-0.902254026976828,
-8.60383133774801));
#30547=CARTESIAN_POINT('Ctrl Pts',(95.7064988447006,-0.904777054623755,
-8.60356182935913));
#30548=CARTESIAN_POINT('Ctrl Pts',(95.7118777212156,-0.909229105266357,
-8.6030853037642));
#30549=CARTESIAN_POINT('Ctrl Pts',(95.7142341411626,-0.911164124103672,
-8.60287786672912));
#30550=CARTESIAN_POINT('Ctrl Pts',(95.7193724395717,-0.91535023030522,-8.6024284177829));
#30551=CARTESIAN_POINT('Ctrl Pts',(95.7221570763296,-0.917597802290566,
-8.6021866518989));
#30552=CARTESIAN_POINT('Ctrl Pts',(95.7299385245949,-0.923820108665626,
-8.601515931548));
#30553=CARTESIAN_POINT('Ctrl Pts',(95.7349575691058,-0.927767027203849,
-8.60108886982957));
#30554=CARTESIAN_POINT('Ctrl Pts',(95.7635872130698,-0.949906625424945,
-8.59868250325961));
#30555=CARTESIAN_POINT('Ctrl Pts',(95.7878518124206,-0.967240331875523,
-8.59675632405785));
#30556=CARTESIAN_POINT('Ctrl Pts',(95.8680069556926,-1.02002300960022,-8.59065703546099));
#30557=CARTESIAN_POINT('Ctrl Pts',(95.9262346484818,-1.05169118227962,-8.58661386465318));
#30558=CARTESIAN_POINT('Ctrl Pts',(96.03923721859,-1.10132960663053,-8.57895404146153));
#30559=CARTESIAN_POINT('Ctrl Pts',(96.0932613484339,-1.1205007344467,-8.57536398091351));
#30560=CARTESIAN_POINT('Ctrl Pts',(96.1659300215136,-1.14046613070225,-8.57047341649828));
#30561=CARTESIAN_POINT('Ctrl Pts',(96.1835060987019,-1.14486161582736,-8.56928644051504));
#30562=CARTESIAN_POINT('Ctrl Pts',(96.2086004523608,-1.15052562382111,-8.56758257635424));
#30563=CARTESIAN_POINT('Ctrl Pts',(96.2160410040387,-1.15212937834259,-8.56707625195697));
#30564=CARTESIAN_POINT('Ctrl Pts',(96.2289302135854,-1.15477707416851,-8.566196972238));
#30565=CARTESIAN_POINT('Ctrl Pts',(96.2343717297784,-1.15585485822996,-8.56582509395023));
#30566=CARTESIAN_POINT('Ctrl Pts',(96.2448390772497,-1.15785134925287,-8.56510837616905));
#30567=CARTESIAN_POINT('Ctrl Pts',(96.2498636817537,-1.15877587528674,-8.56476372875672));
#30568=CARTESIAN_POINT('Ctrl Pts',(96.2617368480116,-1.16088076033953,-8.56394782681518));
#30569=CARTESIAN_POINT('Ctrl Pts',(96.2685900935064,-1.16203324109228,-8.56347571063541));
#30570=CARTESIAN_POINT('Ctrl Pts',(96.289118600927,-1.16529888102834,-8.56205780835957));
#30571=CARTESIAN_POINT('Ctrl Pts',(96.3028209119581,-1.16723169122311,-8.56110647160767));
#30572=CARTESIAN_POINT('Ctrl Pts',(96.3987508623386,-1.17904337428846,-8.55440947349797));
#30573=CARTESIAN_POINT('Ctrl Pts',(96.4817718175587,-1.18046425580085,-8.54840142969621));
#30574=CARTESIAN_POINT('Ctrl Pts',(96.5912543825941,-1.17078131615757,-8.54033712234632));
#30575=CARTESIAN_POINT('Ctrl Pts',(96.6181790593375,-1.16745960028257,-8.53834480689025));
#30576=CARTESIAN_POINT('Ctrl Pts',(96.6871408678306,-1.15652231572469,-8.53324499413282));
#30577=CARTESIAN_POINT('Ctrl Pts',(96.7289260181774,-1.14754371656134,-8.53015731660019));
#30578=CARTESIAN_POINT('Ctrl Pts',(96.7791962291346,-1.13384471562949,-8.52651067663623));
#30579=CARTESIAN_POINT('Ctrl Pts',(96.7882281126902,-1.13126702396626,-8.52585828241797));
#30580=CARTESIAN_POINT('Ctrl Pts',(96.8011868413537,-1.12740038181003,-8.52492719540668));
#30581=CARTESIAN_POINT('Ctrl Pts',(96.8051389760955,-1.12619846015263,-8.52464390170203));
#30582=CARTESIAN_POINT('Ctrl Pts',(96.8120181768897,-1.12406675575666,-8.52415205640604));
#30583=CARTESIAN_POINT('Ctrl Pts',(96.8149480460406,-1.12314628254219,-8.52394298260227));
#30584=CARTESIAN_POINT('Ctrl Pts',(96.8211684247907,-1.12116526836502,-8.52349998822256));
#30585=CARTESIAN_POINT('Ctrl Pts',(96.8244578888169,-1.1201016928115,-8.52326624386522));
#30586=CARTESIAN_POINT('Ctrl Pts',(96.8334472900785,-1.11715138602034,-8.52262877348939));
#30587=CARTESIAN_POINT('Ctrl Pts',(96.8391376545662,-1.11523549709474,-8.52222668750093));
#30588=CARTESIAN_POINT('Ctrl Pts',(96.866786812288,-1.10569027770406,-8.52027885394045));
#30589=CARTESIAN_POINT('Ctrl Pts',(96.8885327351065,-1.09745491291875,-8.51876500485213));
#30590=CARTESIAN_POINT('Ctrl Pts',(97.0128510821649,-1.04611628294192,-8.51013841814316));
#30591=CARTESIAN_POINT('Ctrl Pts',(97.1091498410261,-0.989295292884637,
-8.50351572056958));
#30592=CARTESIAN_POINT('Ctrl Pts',(97.2134379046955,-0.905895424642369,
-8.49501942527079));
#30593=CARTESIAN_POINT('Ctrl Pts',(97.2304261337612,-0.891501552738335,
-8.49358874200812));
#30594=CARTESIAN_POINT('Ctrl Pts',(97.2591285801648,-0.865749810891562,
-8.49107918161947));
#30595=CARTESIAN_POINT('Ctrl Pts',(97.271033824083,-0.854613812469825,-8.49000898352595));
#30596=CARTESIAN_POINT('Ctrl Pts',(97.2879317579071,-0.838136947522117,
-8.48844436315807));
#30597=CARTESIAN_POINT('Ctrl Pts',(97.2931122175869,-0.832990726556178,
-8.48795824783972));
#30598=CARTESIAN_POINT('Ctrl Pts',(97.3021076615307,-0.823886977371597,
-8.48710253898842));
#30599=CARTESIAN_POINT('Ctrl Pts',(97.3059434567362,-0.81995025519821,-8.48673386352082));
#30600=CARTESIAN_POINT('Ctrl Pts',(97.3133466633373,-0.812245075770864,
-8.48601480464279));
#30601=CARTESIAN_POINT('Ctrl Pts',(97.3169170074563,-0.808479601537116,
-8.48566455895368));
#30602=CARTESIAN_POINT('Ctrl Pts',(97.3264192367563,-0.798324469961256,
-8.48472296446376));
#30603=CARTESIAN_POINT('Ctrl Pts',(97.3323051522515,-0.79189243530133,-8.48412970254977));
#30604=CARTESIAN_POINT('Ctrl Pts',(97.354017975294,-0.767629510259118,-8.48190287322368));
#30605=CARTESIAN_POINT('Ctrl Pts',(97.3693727601446,-0.749385759080339,
-8.48025027865178));
#30606=CARTESIAN_POINT('Ctrl Pts',(97.4466517714443,-0.65169560283316,-8.47150611531008));
#30607=CARTESIAN_POINT('Ctrl Pts',(97.4987420384819,-0.565019850578628,
-8.46404776293676));
#30608=CARTESIAN_POINT('Ctrl Pts',(97.5511168404512,-0.445527834110276,
-8.45453284245056));
#30609=CARTESIAN_POINT('Ctrl Pts',(97.5620326663222,-0.417810663962877,
-8.45237863494645));
#30610=CARTESIAN_POINT('Ctrl Pts',(97.5756528823295,-0.378967236935836,
-8.44945613081243));
#30611=CARTESIAN_POINT('Ctrl Pts',(97.5792632684749,-0.36817217512048,-8.44865401945114));
#30612=CARTESIAN_POINT('Ctrl Pts',(97.5852662903431,-0.349318788476043,
-8.44727252384054));
#30613=CARTESIAN_POINT('Ctrl Pts',(97.5877301632562,-0.34128419113304,-8.44668983145004));
#30614=CARTESIAN_POINT('Ctrl Pts',(97.5912254298325,-0.329435249380985,
-8.44584005543365));
#30615=CARTESIAN_POINT('Ctrl Pts',(97.5923239030641,-0.325641202774733,
-8.44556938571883));
#30616=CARTESIAN_POINT('Ctrl Pts',(97.5942293624012,-0.318933750328886,
-8.4450934785937));
#30617=CARTESIAN_POINT('Ctrl Pts',(97.5950442422032,-0.316022683446636,
-8.44488780066328));
#30618=CARTESIAN_POINT('Ctrl Pts',(97.5967931533119,-0.309680931238853,
-8.44444163282195));
#30619=CARTESIAN_POINT('Ctrl Pts',(97.5977228635654,-0.306249136220512,
-8.44420138866213));
#30620=CARTESIAN_POINT('Ctrl Pts',(97.6002524912478,-0.296741255344784,
-8.44353895765058));
#30621=CARTESIAN_POINT('Ctrl Pts',(97.6018193779372,-0.290656388325064,
-8.4431185892707));
#30622=CARTESIAN_POINT('Ctrl Pts',(97.6101275723764,-0.257288717246765,
-8.44083146265122));
#30623=CARTESIAN_POINT('Ctrl Pts',(97.6159399941321,-0.229781476355569,
-8.43901182200827));
#30624=CARTESIAN_POINT('Ctrl Pts',(97.6323279481588,-0.135691566786816,
-8.43292874612855));
#30625=CARTESIAN_POINT('Ctrl Pts',(97.638172637943,-0.0684185474167267,
-8.42881073112888));
#30626=CARTESIAN_POINT('Ctrl Pts',(97.638288928963,0.0670203470091355,-8.42040720520913));
#30627=CARTESIAN_POINT('Ctrl Pts',(97.6324528730179,0.134919763600495,-8.41613413550818));
#30628=CARTESIAN_POINT('Ctrl Pts',(97.6190047976249,0.212193473866689,-8.41098671423547));
#30629=CARTESIAN_POINT('Ctrl Pts',(97.6170827189339,0.222431815812507,-8.41029908822471));
#30630=CARTESIAN_POINT('Ctrl Pts',(97.6136949506509,0.239244388044,-8.40915998524878));
#30631=CARTESIAN_POINT('Ctrl Pts',(97.6123081999403,0.245834073396765,-8.40871098582325));
#30632=CARTESIAN_POINT('Ctrl Pts',(97.6097014358219,0.257714598887316,-8.40789674518727));
#30633=CARTESIAN_POINT('Ctrl Pts',(97.6085011927426,0.263009619749616,-8.40753213777826));
#30634=CARTESIAN_POINT('Ctrl Pts',(97.6058480309298,0.274350083908236,-8.40674748774043));
#30635=CARTESIAN_POINT('Ctrl Pts',(97.6043837704946,0.280392677017655,-8.40632709499444));
#30636=CARTESIAN_POINT('Ctrl Pts',(97.6002437938077,0.296904851152215,-8.40517184912718));
#30637=CARTESIAN_POINT('Ctrl Pts',(97.5974717792407,0.307349428983304,-8.40443395722813));
#30638=CARTESIAN_POINT('Ctrl Pts',(97.5803208595963,0.36856166670961,-8.40006592030178));
#30639=CARTESIAN_POINT('Ctrl Pts',(97.562689114698,0.418347773561824,-8.39633222311502));
#30640=CARTESIAN_POINT('Ctrl Pts',(97.509522427056,0.541509408494223,-8.3866407084649));
#30641=CARTESIAN_POINT('Ctrl Pts',(97.4696048715636,0.6126894090522,-8.38059031032449));
#30642=CARTESIAN_POINT('Ctrl Pts',(97.4050826419625,0.704097088389595,-8.3725078247273));
#30643=CARTESIAN_POINT('Ctrl Pts',(97.3865334626102,0.728321473055659,-8.37033421998128));
#30644=CARTESIAN_POINT('Ctrl Pts',(97.3629628493765,0.75674483211,-8.36776944691956));
#30645=CARTESIAN_POINT('Ctrl Pts',(97.3588221728985,0.761655677787649,-8.36732578461432));
#30646=CARTESIAN_POINT('Ctrl Pts',(97.3523067567127,0.769255912953854,-8.36663864084424));
#30647=CARTESIAN_POINT('Ctrl Pts',(97.3499596327205,0.771968654146624,-8.36639327630558));
#30648=CARTESIAN_POINT('Ctrl Pts',(97.3455951780672,0.776966637785597,-8.36594109026902));
#30649=CARTESIAN_POINT('Ctrl Pts',(97.3435813735682,0.779254769130043,-8.36573403386395));
#30650=CARTESIAN_POINT('Ctrl Pts',(97.3389566729847,0.784468508441572,-8.36526211197091));
#30651=CARTESIAN_POINT('Ctrl Pts',(97.3363400316248,0.787388917153487,-8.36499767366084));
#30652=CARTESIAN_POINT('Ctrl Pts',(97.3281709839798,0.796415203079632,-8.3641798511745));
#30653=CARTESIAN_POINT('Ctrl Pts',(97.3225688064215,0.802475985936705,-8.3636299902638));
#30654=CARTESIAN_POINT('Ctrl Pts',(97.2820552915367,0.845392049097954,-8.35972685056704));
#30655=CARTESIAN_POINT('Ctrl Pts',(97.2448524988876,0.880019713295745,-8.35652509977306));
#30656=CARTESIAN_POINT('Ctrl Pts',(97.1398571894401,0.965780820581755,-8.34808344016331));
#30657=CARTESIAN_POINT('Ctrl Pts',(97.068591409239,1.01216887893699,-8.3429237716438));
#30658=CARTESIAN_POINT('Ctrl Pts',(96.9671112961228,1.06360745098873,-8.33565167848363));
#30659=CARTESIAN_POINT('Ctrl Pts',(96.9407860016459,1.07575181089376,-8.33377362916025));
#30660=CARTESIAN_POINT('Ctrl Pts',(96.9053929096018,1.09052108054632,-8.33124500271943));
#30661=CARTESIAN_POINT('Ctrl Pts',(96.8967020705501,1.09402650998677,-8.33062384178089));
#30662=CARTESIAN_POINT('Ctrl Pts',(96.8824679795996,1.09957122616767,-8.32960563061935));
#30663=CARTESIAN_POINT('Ctrl Pts',(96.8769494743406,1.10167322771075,-8.32921066703086));
#30664=CARTESIAN_POINT('Ctrl Pts',(96.8662633344815,1.10565181803414,-8.32844534035056));
#30665=CARTESIAN_POINT('Ctrl Pts',(96.8610978990314,1.1075339022676,-8.32807517003289));
#30666=CARTESIAN_POINT('Ctrl Pts',(96.8490341189216,1.11183403883277,-8.32721001601538));
#30667=CARTESIAN_POINT('Ctrl Pts',(96.8421261257348,1.11422414740502,-8.32671413318425));
#30668=CARTESIAN_POINT('Ctrl Pts',(96.819701613168,1.12174984229938,-8.32510261706217));
#30669=CARTESIAN_POINT('Ctrl Pts',(96.8041009091444,1.12662658888919,-8.32397868889354));
#30670=CARTESIAN_POINT('Ctrl Pts',(96.7669469884363,1.13739735591256,-8.32129407832577));
#30671=CARTESIAN_POINT('Ctrl Pts',(96.7453181829567,1.14300560672248,-8.31972498347182));
#30672=CARTESIAN_POINT('Ctrl Pts',(96.6605834513324,1.16242257878544,-8.31355345120968));
#30673=CARTESIAN_POINT('Ctrl Pts',(96.5965489616525,1.17164459404734,-8.30882966436784));
#30674=CARTESIAN_POINT('Ctrl Pts',(96.4691981810892,1.17940197167777,-8.29946576974513));
#30675=CARTESIAN_POINT('Ctrl Pts',(96.4060950144904,1.17818025902253,-8.29484277039885));
#30676=CARTESIAN_POINT('Ctrl Pts',(96.3334283030631,1.1709196655273,-8.28972179981462));
#30677=CARTESIAN_POINT('Ctrl Pts',(96.323481788128,1.16979762540815,-8.28902543102294));
#30678=CARTESIAN_POINT('Ctrl Pts',(96.3096438828062,1.1680576800051,-8.28806409847642));
#30679=CARTESIAN_POINT('Ctrl Pts',(96.305739797882,1.16754689054268,-8.28779370987133));
#30680=CARTESIAN_POINT('Ctrl Pts',(96.2990073946744,1.16663169662121,-8.28732895804583));
#30681=CARTESIAN_POINT('Ctrl Pts',(96.2961778819051,1.16623656557837,-8.28713409497307));
#30682=CARTESIAN_POINT('Ctrl Pts',(96.2902091667988,1.16538090286236,-8.28672406049733));
#30683=CARTESIAN_POINT('Ctrl Pts',(96.2870703361303,1.16491797494558,-8.28650903003984));
#30684=CARTESIAN_POINT('Ctrl Pts',(96.279282138397,1.16373716305372,-8.28597688976864));
#30685=CARTESIAN_POINT('Ctrl Pts',(96.2746350666321,1.16300408576626,-8.28566061379496));
#30686=CARTESIAN_POINT('Ctrl Pts',(96.2570975170206,1.1601297284631,-8.28447129234524));
#30687=CARTESIAN_POINT('Ctrl Pts',(96.2442380221496,1.15780172687388,-8.2836079439286));
#30688=CARTESIAN_POINT('Ctrl Pts',(96.211281539951,1.1512672099253,-8.28141164209038));
#30689=CARTESIAN_POINT('Ctrl Pts',(96.1912504127016,1.1467482515924,-8.28009239301039));
#30690=CARTESIAN_POINT('Ctrl Pts',(96.1153409310211,1.1275243779895,-8.27511812391382));
#30691=CARTESIAN_POINT('Ctrl Pts',(96.0604515700358,1.10923854495724,-8.2715706463311));
#30692=CARTESIAN_POINT('Ctrl Pts',(95.9781481430738,1.07491196548991,-8.26604898326986));
#30693=CARTESIAN_POINT('Ctrl Pts',(95.9496855826237,1.06168091221913,-8.26410025730001));
#30694=CARTESIAN_POINT('Ctrl Pts',(95.9218015205746,1.04733926464621,-8.26212858994183));
#30695=CARTESIAN_POINT('',(97.6382305443328,0.000598681062270171,-8.32477232136367));
#30696=CARTESIAN_POINT('Ctrl Pts',(95.9218018246467,1.04733942103997,-8.16230712347374));
#30697=CARTESIAN_POINT('Ctrl Pts',(95.9376213785056,1.05547590789257,-8.16342335775821));
#30698=CARTESIAN_POINT('Ctrl Pts',(95.9536330940809,1.06325799827498,-8.16454713565674));
#30699=CARTESIAN_POINT('Ctrl Pts',(95.9993064571837,1.08418854436589,-8.1677457616158));
#30700=CARTESIAN_POINT('Ctrl Pts',(96.0293304725305,1.09647420555693,-8.16984076206555));
#30701=CARTESIAN_POINT('Ctrl Pts',(96.0689874993574,1.11082084931101,-8.17261895661093));
#30702=CARTESIAN_POINT('Ctrl Pts',(96.0781944250211,1.11402292821804,-8.17326466054049));
#30703=CARTESIAN_POINT('Ctrl Pts',(96.0931184993395,1.11900658447433,-8.17431296398046));
#30704=CARTESIAN_POINT('Ctrl Pts',(96.0988114706818,1.12085953256381,-8.17471323324801));
#30705=CARTESIAN_POINT('Ctrl Pts',(96.1097329183442,1.12432237715949,-8.17548195875513));
#30706=CARTESIAN_POINT('Ctrl Pts',(96.1149589818321,1.12593941101157,-8.17585017235612));
#30707=CARTESIAN_POINT('Ctrl Pts',(96.1270159411701,1.12957819471921,-8.17670061075007));
#30708=CARTESIAN_POINT('Ctrl Pts',(96.1338542365482,1.13157447668932,-8.17718364132761));
#30709=CARTESIAN_POINT('Ctrl Pts',(96.1554494191646,1.13766663184967,-8.17871144984711));
#30710=CARTESIAN_POINT('Ctrl Pts',(96.1702678110726,1.14153663793594,-8.17976336547231));
#30711=CARTESIAN_POINT('Ctrl Pts',(96.2051113702321,1.14991418852876,-8.18224621418645));
#30712=CARTESIAN_POINT('Ctrl Pts',(96.2251867630577,1.15418924843768,-8.18368395328458));
#30713=CARTESIAN_POINT('Ctrl Pts',(96.2999933746522,1.1680866102826,-8.18906859257534));
#30714=CARTESIAN_POINT('Ctrl Pts',(96.3552681436596,1.17435583488003,-8.19310523061123));
#30715=CARTESIAN_POINT('Ctrl Pts',(96.4868476555972,1.17991420171222,-8.2027574443861));
#30716=CARTESIAN_POINT('Ctrl Pts',(96.5630604304775,1.17574320280996,-8.20838698803029));
#30717=CARTESIAN_POINT('Ctrl Pts',(96.6477295567153,1.16280832750164,-8.21438606753708));
#30718=CARTESIAN_POINT('Ctrl Pts',(96.6570998995637,1.1612606297152,-8.21504621847737));
#30719=CARTESIAN_POINT('Ctrl Pts',(96.6702417737039,1.15892634951521,-8.21596583650769));
#30720=CARTESIAN_POINT('Ctrl Pts',(96.6740294316017,1.15823440365383,-8.2162301506444));
#30721=CARTESIAN_POINT('Ctrl Pts',(96.6808769345714,1.15694873980231,-8.21670658284306));
#30722=CARTESIAN_POINT('Ctrl Pts',(96.6839379406715,1.15636142735559,-8.2169190496742));
#30723=CARTESIAN_POINT('Ctrl Pts',(96.6902045659298,1.15513324279914,-8.21735292706584));
#30724=CARTESIAN_POINT('Ctrl Pts',(96.6934099036018,1.15449116565154,-8.21757426899638));
#30725=CARTESIAN_POINT('Ctrl Pts',(96.701660562451,1.15280267445468,-8.21814260448124));
#30726=CARTESIAN_POINT('Ctrl Pts',(96.706701830934,1.15173646808278,-8.21848850757027));
#30727=CARTESIAN_POINT('Ctrl Pts',(96.7280597979011,1.14707270586781,-8.21994883013858));
#30728=CARTESIAN_POINT('Ctrl Pts',(96.7443068691964,1.14316103401756,-8.22104695234132));
#30729=CARTESIAN_POINT('Ctrl Pts',(96.7886996680762,1.13146805901097,-8.22402604699274));
#30730=CARTESIAN_POINT('Ctrl Pts',(96.8166489027617,1.12298358140763,-8.22587789398752));
#30731=CARTESIAN_POINT('Ctrl Pts',(96.9310258042014,1.08356174976196,-8.23346407644181));
#30732=CARTESIAN_POINT('Ctrl Pts',(97.014000519188,1.04361631120548,-8.23901238498897));
#30733=CARTESIAN_POINT('Ctrl Pts',(97.1181634727909,0.977520428472241,-8.24687328584309));
#30734=CARTESIAN_POINT('Ctrl Pts',(97.144136534596,0.959534916780235,-8.24891487487024));
#30735=CARTESIAN_POINT('Ctrl Pts',(97.1770996325259,0.934690752812255,-8.25163438835768));
#30736=CARTESIAN_POINT('Ctrl Pts',(97.1847727488286,0.928757514339493,-8.25227694135909));
#30737=CARTESIAN_POINT('Ctrl Pts',(97.1970538391894,0.91901640792623,-8.25332137609325));
#30738=CARTESIAN_POINT('Ctrl Pts',(97.201707743476,0.915266965168827,-8.25372095942066));
#30739=CARTESIAN_POINT('Ctrl Pts',(97.2103866369195,0.908165160879373,-8.25447340853585));
#30740=CARTESIAN_POINT('Ctrl Pts',(97.21441820407,0.904821039825654,-8.25482593955127));
#30741=CARTESIAN_POINT('Ctrl Pts',(97.2184747229205,0.901410287225249,-8.255183740089));
#30742=CARTESIAN_POINT('Ctrl Pts',(97.2185221684086,0.901370388295164,-8.255187925393));
#30743=CARTESIAN_POINT('Ctrl Pts',(97.2186131797962,0.9012938406779,-8.25519595459592));
#30744=CARTESIAN_POINT('Ctrl Pts',(97.2186567461433,0.901257192616039,-8.25519979846698));
#30745=CARTESIAN_POINT('Ctrl Pts',(97.2187403893975,0.901186821456293,-8.25520717903109));
#30746=CARTESIAN_POINT('Ctrl Pts',(97.218780466728,0.90115309883054,-8.25521071570583));
#30747=CARTESIAN_POINT('Ctrl Pts',(97.2240497492897,0.896718718985027,-8.2556757505796));
#30748=CARTESIAN_POINT('Ctrl Pts',(97.2292404544705,0.892272712292352,-8.25613907959916));
#30749=CARTESIAN_POINT('Ctrl Pts',(97.2401289638164,0.882780810148187,-8.2571222766092));
#30750=CARTESIAN_POINT('Ctrl Pts',(97.2458171210067,0.877724374734772,-8.25764256447768));
#30751=CARTESIAN_POINT('Ctrl Pts',(97.2608102664443,0.864133932322353,-8.25903203219213));
#30752=CARTESIAN_POINT('Ctrl Pts',(97.2700274946725,0.855505019569865,-8.25990509755621));
#30753=CARTESIAN_POINT('Ctrl Pts',(97.2980199134487,0.828441799380065,-8.2626162295607));
#30754=CARTESIAN_POINT('Ctrl Pts',(97.3163164459866,0.809526254503011,-8.26447381892073));
#30755=CARTESIAN_POINT('Ctrl Pts',(97.3953994078684,0.722087977457959,-8.27289646660675));
#30756=CARTESIAN_POINT('Ctrl Pts',(97.4486996239311,0.64722820615961,-8.27970909160612));
#30757=CARTESIAN_POINT('Ctrl Pts',(97.5093456169397,0.536807066780993,-8.28884125681446));
#30758=CARTESIAN_POINT('Ctrl Pts',(97.5245813818428,0.505934456595152,-8.29130250206012));
#30759=CARTESIAN_POINT('Ctrl Pts',(97.5408830509369,0.468895515912719,-8.29411514053513));
#30760=CARTESIAN_POINT('Ctrl Pts',(97.5432788478144,0.46333618560343,-8.2945336730474));
#30761=CARTESIAN_POINT('Ctrl Pts',(97.5471175739887,0.454236197606946,-8.29521257879922));
#30762=CARTESIAN_POINT('Ctrl Pts',(97.5485862794652,0.450706632784188,-8.2954743957543));
#30763=CARTESIAN_POINT('Ctrl Pts',(97.5511927632089,0.444355775744889,-8.29594271117344));
#30764=CARTESIAN_POINT('Ctrl Pts',(97.5523368172484,0.441537179297196,-8.29614957184232));
#30765=CARTESIAN_POINT('Ctrl Pts',(97.5548348966612,0.43531359645602,-8.29660416233487));
#30766=CARTESIAN_POINT('Ctrl Pts',(97.5561839592968,0.431906707707123,-8.29685159916921));
#30767=CARTESIAN_POINT('Ctrl Pts',(97.5600532922032,0.422000377830806,-8.29756714038691));
#30768=CARTESIAN_POINT('Ctrl Pts',(97.5625318400079,0.415484652260095,-8.29803287268604));
#30769=CARTESIAN_POINT('Ctrl Pts',(97.5833160763188,0.359351239590522,-8.30200638201027));
#30770=CARTESIAN_POINT('Ctrl Pts',(97.5983207980556,0.30856770415855,-8.30534320794276));
#30771=CARTESIAN_POINT('Ctrl Pts',(97.628674876271,0.172784145315577,-8.31400656589799));
#30772=CARTESIAN_POINT('Ctrl Pts',(97.6381868702256,0.0868239361698437,
-8.31925247929609));
#30773=CARTESIAN_POINT('Ctrl Pts',(97.6382307967427,0.000600001017636307,
-8.32477179780212));
#30774=CARTESIAN_POINT('Ctrl Pts',(97.6382307974286,0.000598653194140394,
-8.32477188407827));
#30775=CARTESIAN_POINT('Ctrl Pts',(97.6382392206163,-0.0159725571986599,
-8.32583263163235));
#30776=CARTESIAN_POINT('Ctrl Pts',(97.6378979026431,-0.0325416332374212,
-8.32690186388278));
#30777=CARTESIAN_POINT('Ctrl Pts',(97.6367128128061,-0.0609447856470732,
-8.32875333490612));
#30778=CARTESIAN_POINT('Ctrl Pts',(97.6360396297213,-0.0727834900835447,
-8.32953058173302));
#30779=CARTESIAN_POINT('Ctrl Pts',(97.6347089373993,-0.0912586028483084,
-8.33075321158656));
#30780=CARTESIAN_POINT('Ctrl Pts',(97.6341736078574,-0.0979032219807065,
-8.33119489236586));
#30781=CARTESIAN_POINT('Ctrl Pts',(97.633116109985,-0.109769667460043,-8.33198735939884));
#30782=CARTESIAN_POINT('Ctrl Pts',(97.6326153903691,-0.114993262975679,
-8.33233747966645));
#30783=CARTESIAN_POINT('Ctrl Pts',(97.6315356383286,-0.1255165293268,-8.33304548240145));
#30784=CARTESIAN_POINT('Ctrl Pts',(97.6309554970805,-0.130815959395499,
-8.33340339119062));
#30785=CARTESIAN_POINT('Ctrl Pts',(97.6296324605646,-0.142187290451245,
-8.33417439734584));
#30786=CARTESIAN_POINT('Ctrl Pts',(97.628878201172,-0.148257685264711,-8.33458783818055));
#30787=CARTESIAN_POINT('Ctrl Pts',(97.6267212323564,-0.164577266213844,
-8.33570445639677));
#30788=CARTESIAN_POINT('Ctrl Pts',(97.6252307472846,-0.174814103076982,
-8.33641034116554));
#30789=CARTESIAN_POINT('Ctrl Pts',(97.6176480683421,-0.222479970214684,
-8.33972357386405));
#30790=CARTESIAN_POINT('Ctrl Pts',(97.6098858946794,-0.259616637683789,
-8.34238221654071));
#30791=CARTESIAN_POINT('Ctrl Pts',(97.5750158959795,-0.393756554545006,
-8.35227324131233));
#30792=CARTESIAN_POINT('Ctrl Pts',(97.5372986198312,-0.487536874375286,
-8.35979328114584));
#30793=CARTESIAN_POINT('Ctrl Pts',(97.4790480813285,-0.591574945361573,
-8.36837896019924));
#30794=CARTESIAN_POINT('Ctrl Pts',(97.4695933649293,-0.607562448508005,
-8.36970418491041));
#30795=CARTESIAN_POINT('Ctrl Pts',(97.4533341308031,-0.633628616101496,
-8.37186705020228));
#30796=CARTESIAN_POINT('Ctrl Pts',(97.4467448336499,-0.643837124172231,
-8.37271467999996));
#30797=CARTESIAN_POINT('Ctrl Pts',(97.4374587663522,-0.657746401694128,
-8.37386847899008));
#30798=CARTESIAN_POINT('Ctrl Pts',(97.4348969081134,-0.661535732143874,
-8.37418269431734));
#30799=CARTESIAN_POINT('Ctrl Pts',(97.4305356649558,-0.667906288813469,
-8.37471062264048));
#30800=CARTESIAN_POINT('Ctrl Pts',(97.428747911615,-0.670495378472053,-8.37492508866309));
#30801=CARTESIAN_POINT('Ctrl Pts',(97.4253024255865,-0.675442736868094,
-8.37533467902837));
#30802=CARTESIAN_POINT('Ctrl Pts',(97.4236463876081,-0.677802117725618,
-8.37552991785086));
#30803=CARTESIAN_POINT('Ctrl Pts',(97.4191879243562,-0.684104817828945,
-8.37605128460905));
#30804=CARTESIAN_POINT('Ctrl Pts',(97.4163697997968,-0.688037043567038,
-8.37637637124131));
#30805=CARTESIAN_POINT('Ctrl Pts',(97.405903430926,-0.702452693990141,-8.37756789149714));
#30806=CARTESIAN_POINT('Ctrl Pts',(97.3981059801271,-0.712827322481144,
-8.37842490051302));
#30807=CARTESIAN_POINT('Ctrl Pts',(97.3204164942796,-0.812713158967548,
-8.38669419186976));
#30808=CARTESIAN_POINT('Ctrl Pts',(97.238088213149,-0.891810683197873,-8.39343675762738));
#30809=CARTESIAN_POINT('Ctrl Pts',(97.1228414963137,-0.974250060021788,
-8.40237357785148));
#30810=CARTESIAN_POINT('Ctrl Pts',(97.0994104536838,-0.989774516967249,
-8.40416523485624));
#30811=CARTESIAN_POINT('Ctrl Pts',(97.0641821565468,-1.0113428722489,-8.40684059241589));
#30812=CARTESIAN_POINT('Ctrl Pts',(97.0528015696989,-1.01805000561974,-8.40770211824817));
#30813=CARTESIAN_POINT('Ctrl Pts',(97.0319632719575,-1.02986332979704,-8.40927642913202));
#30814=CARTESIAN_POINT('Ctrl Pts',(97.0225438004328,-1.03503423231993,-8.4099869085273));
#30815=CARTESIAN_POINT('Ctrl Pts',(97.0076350180766,-1.04295501235957,-8.41111031068038));
#30816=CARTESIAN_POINT('Ctrl Pts',(97.0021925532073,-1.04579217274279,-8.41152017771205));
#30817=CARTESIAN_POINT('Ctrl Pts',(96.9966573556901,-1.04862287328072,-8.41193686312558));
#30818=CARTESIAN_POINT('Ctrl Pts',(96.9965864609357,-1.04865911979573,-8.41194220000072));
#30819=CARTESIAN_POINT('Ctrl Pts',(96.9964209083942,-1.04874374102696,-8.41195466254078));
#30820=CARTESIAN_POINT('Ctrl Pts',(96.9963262477872,-1.0487921100896,-8.41196178839662));
#30821=CARTESIAN_POINT('Ctrl Pts',(96.9961053615563,-1.0489049393915,-8.41197841614494));
#30822=CARTESIAN_POINT('Ctrl Pts',(96.9959791307749,-1.04896938969725,-8.41198791838805));
#30823=CARTESIAN_POINT('Ctrl Pts',(96.9956848752093,-1.04911956233236,-8.41201006879238));
#30824=CARTESIAN_POINT('Ctrl Pts',(96.9955168415815,-1.04920526702239,-8.41202271755359));
#30825=CARTESIAN_POINT('Ctrl Pts',(96.9908003906001,-1.05160944098781,-8.41237774505554));
#30826=CARTESIAN_POINT('Ctrl Pts',(96.9862370290952,-1.05389832021191,-8.41272114002119));
#30827=CARTESIAN_POINT('Ctrl Pts',(96.9756273597883,-1.059133833904,-8.41351934926885));
#30828=CARTESIAN_POINT('Ctrl Pts',(96.9695704528358,-1.06205846190355,-8.4139749066734));
#30829=CARTESIAN_POINT('Ctrl Pts',(96.9540926268301,-1.06936923610807,-8.41513887929156));
#30830=CARTESIAN_POINT('Ctrl Pts',(96.9446382613142,-1.0736827914018,-8.41584972703787));
#30831=CARTESIAN_POINT('Ctrl Pts',(96.8660674157879,-1.10828197788786,-8.42175754354924));
#30832=CARTESIAN_POINT('Ctrl Pts',(96.7942566176936,-1.13198023258078,-8.42717612754659));
#30833=CARTESIAN_POINT('Ctrl Pts',(96.6642970988846,-1.16142022136874,-8.43692382029308));
#30834=CARTESIAN_POINT('Ctrl Pts',(96.6070433823238,-1.17002463992289,-8.44119411273427));
#30835=CARTESIAN_POINT('Ctrl Pts',(96.52895620662,-1.17593625296761,-8.44684903970999));
#30836=CARTESIAN_POINT('Ctrl Pts',(96.508485818296,-1.17694968628901,-8.44831532663428));
#30837=CARTESIAN_POINT('Ctrl Pts',(96.4749530420315,-1.17773337046574,-8.45068086426726));
#30838=CARTESIAN_POINT('Ctrl Pts',(96.4619029600606,-1.1778214408856,-8.45159244455721));
#30839=CARTESIAN_POINT('Ctrl Pts',(96.4441520343127,-1.17764618392891,-8.45281779036776));
#30840=CARTESIAN_POINT('Ctrl Pts',(96.43945083449,-1.17757161316871,-8.45314092004508));
#30841=CARTESIAN_POINT('Ctrl Pts',(96.4315789125318,-1.17739959063944,-8.45367951175966));
#30842=CARTESIAN_POINT('Ctrl Pts',(96.4284079498098,-1.17731747937758,-8.45389579472045));
#30843=CARTESIAN_POINT('Ctrl Pts',(96.4223814925994,-1.1771370594775,-8.45430551774925));
#30844=CARTESIAN_POINT('Ctrl Pts',(96.4195259719922,-1.1770411699135,-8.45449909343269));
#30845=CARTESIAN_POINT('Ctrl Pts',(96.4127349759271,-1.176788382249,-8.45495817417184));
#30846=CARTESIAN_POINT('Ctrl Pts',(96.4087998515414,-1.17662213127505,-8.45522317070103));
#30847=CARTESIAN_POINT('Ctrl Pts',(96.3948590583756,-1.17596308779483,-8.45615857024002));
#30848=CARTESIAN_POINT('Ctrl Pts',(96.384858585929,-1.17536236578321,-8.45682338843237));
#30849=CARTESIAN_POINT('Ctrl Pts',(96.3155119626332,-1.17030796927137,-8.46139799979149));
#30850=CARTESIAN_POINT('Ctrl Pts',(96.2565625723474,-1.16148864254912,-8.46510876878153));
#30851=CARTESIAN_POINT('Ctrl Pts',(96.1330059625051,-1.13330116666639,-8.47296146268175));
#30852=CARTESIAN_POINT('Ctrl Pts',(96.068888917809,-1.11277423120893,-8.47708672042868));
#30853=CARTESIAN_POINT('Ctrl Pts',(95.9751094120417,-1.07363599069651,-8.48354641586234));
#30854=CARTESIAN_POINT('Ctrl Pts',(95.9439442028268,-1.05899443342629,-8.48576789680546));
#30855=CARTESIAN_POINT('Ctrl Pts',(95.9049702986871,-1.03855429685316,-8.48866806842902));
#30856=CARTESIAN_POINT('Ctrl Pts',(95.8965287162861,-1.03399467135022,-8.48930376882515));
#30857=CARTESIAN_POINT('Ctrl Pts',(95.8829407577058,-1.02643939570379,-8.4903397920286));
#30858=CARTESIAN_POINT('Ctrl Pts',(95.8777596271705,-1.02350689518473,-8.49073788508202));
#30859=CARTESIAN_POINT('Ctrl Pts',(95.8678521795802,-1.01779970449294,-8.49150513188693));
#30860=CARTESIAN_POINT('Ctrl Pts',(95.8631225493015,-1.01503105241784,-8.49187406296975));
#30861=CARTESIAN_POINT('Ctrl Pts',(95.8523325665774,-1.00861323100451,-8.49272194315122));
#30862=CARTESIAN_POINT('Ctrl Pts',(95.8462854736071,-1.00494229636424,-8.49320166622082));
#30863=CARTESIAN_POINT('Ctrl Pts',(95.8271264802143,-0.99307416147238,-8.49473635058312));
#30864=CARTESIAN_POINT('Ctrl Pts',(95.814143246543,-0.984673401847484,-8.49579865488929));
#30865=CARTESIAN_POINT('Ctrl Pts',(95.7352913549769,-0.931421076440506,
-8.50239248583097));
#30866=CARTESIAN_POINT('Ctrl Pts',(95.6739613913848,-0.880243095976197,
-8.50816324845082));
#30867=CARTESIAN_POINT('Ctrl Pts',(95.5858991665516,-0.790156366322242,
-8.5174029828112));
#30868=CARTESIAN_POINT('Ctrl Pts',(95.5555031009311,-0.755152790578475,
-8.52081160964979));
#30869=CARTESIAN_POINT('Ctrl Pts',(95.5143762584434,-0.701730808254361,
-8.5256841105564));
#30870=CARTESIAN_POINT('Ctrl Pts',(95.5019564887557,-0.684668663603472,
-8.52719514758669));
#30871=CARTESIAN_POINT('Ctrl Pts',(95.4824510421254,-0.656300345233046,
-8.52962437156156));
#30872=CARTESIAN_POINT('Ctrl Pts',(95.4750874342494,-0.645191677327805,
-8.5305556744556));
#30873=CARTESIAN_POINT('Ctrl Pts',(95.4653624018703,-0.629965555754765,
-8.53180296083662));
#30874=CARTESIAN_POINT('Ctrl Pts',(95.4628352965825,-0.625955811873396,
-8.53212873354624));
#30875=CARTESIAN_POINT('Ctrl Pts',(95.4586532710032,-0.61923055156973,-8.5326705009611));
#30876=CARTESIAN_POINT('Ctrl Pts',(95.4569850417627,-0.61652342802353,-8.53288733689324));
#30877=CARTESIAN_POINT('Ctrl Pts',(95.4538422470899,-0.611376896545914,
-8.53329716717314));
#30878=CARTESIAN_POINT('Ctrl Pts',(95.4523655440753,-0.608938844717003,
-8.53349030313241));
#30879=CARTESIAN_POINT('Ctrl Pts',(95.4488832289914,-0.603142119974017,
-8.53394716861775));
#30880=CARTESIAN_POINT('Ctrl Pts',(95.4468854549054,-0.59977874207513,-8.53421040115479));
#30881=CARTESIAN_POINT('Ctrl Pts',(95.4399124979376,-0.587904987854958,
-8.53513342793279));
#30882=CARTESIAN_POINT('Ctrl Pts',(95.4350272745504,-0.579341881095869,
-8.53578782797955));
#30883=CARTESIAN_POINT('Ctrl Pts',(95.3967842589272,-0.510307554410845,
-8.54098224062719));
#30884=CARTESIAN_POINT('Ctrl Pts',(95.36869213472,-0.44706180687142,-8.54525141769817));
#30885=CARTESIAN_POINT('Ctrl Pts',(95.3449414061817,-0.37773568272148,-8.5497847485548));
#30886=CARTESIAN_POINT('Ctrl Pts',(95.34360083012,-0.373753284475691,-8.55004464719236));
#30887=CARTESIAN_POINT('Ctrl Pts',(95.3243124592721,-0.315423496565407,
-8.55384477511811));
#30888=CARTESIAN_POINT('Ctrl Pts',(95.310329465387,-0.259849444097576,-8.55738671506793));
#30889=CARTESIAN_POINT('Ctrl Pts',(95.2968346320253,-0.182915999438662,
-8.56236816534095));
#30890=CARTESIAN_POINT('Ctrl Pts',(95.2937749494476,-0.162259198428188,
-8.56371265947386));
#30891=CARTESIAN_POINT('Ctrl Pts',(95.2894011079331,-0.1261265244011,-8.56608435046378));
#30892=CARTESIAN_POINT('Ctrl Pts',(95.287840940841,-0.110685451145692,-8.56710414537149));
#30893=CARTESIAN_POINT('Ctrl Pts',(95.286007407231,-0.0880808904912756,
-8.56860826421662));
#30894=CARTESIAN_POINT('Ctrl Pts',(95.2854935643887,-0.0809381603499936,
-8.5690851717157));
#30895=CARTESIAN_POINT('Ctrl Pts',(95.284701828785,-0.068326452183756,-8.56993030137004));
#30896=CARTESIAN_POINT('Ctrl Pts',(95.284396876667,-0.0628593404331867,
-8.57029767646876));
#30897=CARTESIAN_POINT('Ctrl Pts',(95.2838391923939,-0.0514282886749231,
-8.57106802598894));
#30898=CARTESIAN_POINT('Ctrl Pts',(95.2835936565079,-0.0454641702217535,
-8.57147121209585));
#30899=CARTESIAN_POINT('Ctrl Pts',(95.2830692914335,-0.0298376782038799,
-8.57253101724502));
#30900=CARTESIAN_POINT('Ctrl Pts',(95.2828640671068,-0.0201734537291122,
-8.5731898848881));
#30901=CARTESIAN_POINT('Ctrl Pts',(95.2824952750901,0.0211594125294026,
-8.57602314687485));
#30902=CARTESIAN_POINT('Ctrl Pts',(95.2834901153434,0.0528225255822563,
-8.57823261008795));
#30903=CARTESIAN_POINT('Ctrl Pts',(95.2923559830223,0.176215314340497,-8.5870009905925));
#30904=CARTESIAN_POINT('Ctrl Pts',(95.3096931054212,0.266928711875819,-8.59382194027456));
#30905=CARTESIAN_POINT('Ctrl Pts',(95.3461421143299,0.382342066056478,-8.60264342910261));
#30906=CARTESIAN_POINT('Ctrl Pts',(95.3558972987908,0.40967264824717,-8.60474035401363));
#30907=CARTESIAN_POINT('Ctrl Pts',(95.3728194965996,0.452066766911041,-8.60797972913013));
#30908=CARTESIAN_POINT('Ctrl Pts',(95.3793136272116,0.467385375310766,-8.60914736039707));
#30909=CARTESIAN_POINT('Ctrl Pts',(95.3882384258373,0.487255065858787,-8.61065350251444));
#30910=CARTESIAN_POINT('Ctrl Pts',(95.3903770900645,0.491934204160688,-8.6110075659273));
#30911=CARTESIAN_POINT('Ctrl Pts',(95.3939240041136,0.499561827048202,-8.61158354419316));
#30912=CARTESIAN_POINT('Ctrl Pts',(95.3953139559845,0.502518669685959,-8.61180652669242));
#30913=CARTESIAN_POINT('Ctrl Pts',(95.398054403159,0.508285960691424,-8.61224081945136));
#30914=CARTESIAN_POINT('Ctrl Pts',(95.3994037794112,0.511096882861558,-8.61245219050216));
#30915=CARTESIAN_POINT('Ctrl Pts',(95.402446304048,0.517370863497887,-8.61292337208669));
#30916=CARTESIAN_POINT('Ctrl Pts',(95.4041453393494,0.520831067755723,-8.61318282702259));
#30917=CARTESIAN_POINT('Ctrl Pts',(95.4101003838315,0.532809917757184,-8.61407982287164));
#30918=CARTESIAN_POINT('Ctrl Pts',(95.4144428308351,0.541285515805737,-8.61471235892664));
#30919=CARTESIAN_POINT('Ctrl Pts',(95.4542031382021,0.616623835850128,-8.62032407155302));
#30920=CARTESIAN_POINT('Ctrl Pts',(95.4958900581477,0.67999095751371,-8.62497471224905));
#30921=CARTESIAN_POINT('Ctrl Pts',(95.5784303611809,0.782434427210256,-8.63311283983266));
#30922=CARTESIAN_POINT('Ctrl Pts',(95.6165353063062,0.823390541596666,-8.63657465287442));
#30923=CARTESIAN_POINT('Ctrl Pts',(95.6724613362659,0.875525040333735,-8.64145330767545));
#30924=CARTESIAN_POINT('Ctrl Pts',(95.6878870509317,0.889166801479525,-8.64277972748967));
#30925=CARTESIAN_POINT('Ctrl Pts',(95.7154252675029,0.912262466272874,-8.64512239240248));
#30926=CARTESIAN_POINT('Ctrl Pts',(95.7273801088304,0.921896902424378,-8.64613148934295));
#30927=CARTESIAN_POINT('Ctrl Pts',(95.7451580267079,0.935659674561807,-8.64762274174136));
#30928=CARTESIAN_POINT('Ctrl Pts',(95.7508360468243,0.939973413900392,-8.64809766340276));
#30929=CARTESIAN_POINT('Ctrl Pts',(95.7609394249046,0.947505490666184,-8.64894053586588));
#30930=CARTESIAN_POINT('Ctrl Pts',(95.7653487345696,0.950745077042163,-8.6493076548794));
#30931=CARTESIAN_POINT('Ctrl Pts',(95.7746269416008,0.957462868727021,-8.65007873618765));
#30932=CARTESIAN_POINT('Ctrl Pts',(95.7795000809177,0.960934919487381,-8.65048291868082));
#30933=CARTESIAN_POINT('Ctrl Pts',(95.7923683063355,0.969956325422524,-8.65154823968423));
#30934=CARTESIAN_POINT('Ctrl Pts',(95.8004059495252,0.975443879336585,-8.65221166985895));
#30935=CARTESIAN_POINT('Ctrl Pts',(95.8353978852335,0.998703449836975,-8.65509214989827));
#30936=CARTESIAN_POINT('Ctrl Pts',(95.8630063518476,1.01546106633469,-8.65734573735509));
#30937=CARTESIAN_POINT('Ctrl Pts',(95.9013687031556,1.0366396328609,-8.66045379444873));
#30938=CARTESIAN_POINT('Ctrl Pts',(95.9115484421861,1.04206578788199,-8.6612763282379));
#30939=CARTESIAN_POINT('Ctrl Pts',(95.921801762405,1.04733938902713,-8.66210246100831));
#30940=CARTESIAN_POINT('Origin',(96.460480949577,-7.19464945638997E-16,
0.924367114736168));
#30941=CARTESIAN_POINT('',(95.9218016185417,1.04733931503377,-9.26219012624909));
#30942=CARTESIAN_POINT('',(95.9218016730733,1.04733934308104,-9.16391269549479));
#30943=CARTESIAN_POINT('',(95.9218016730721,1.04733934308042,0.924367114736168));
#30944=CARTESIAN_POINT('',(97.6382311976804,0.000311627330674785,-8.92336529225763));
#30945=CARTESIAN_POINT('Ctrl Pts',(95.9218016185417,1.04733931503376,-9.26219012624909));
#30946=CARTESIAN_POINT('Ctrl Pts',(95.8332784251477,1.00180907100097,-9.25501416132673));
#30947=CARTESIAN_POINT('Ctrl Pts',(95.7508631399599,0.945229306744171,-9.24755876670025));
#30948=CARTESIAN_POINT('Ctrl Pts',(95.6635171965987,0.86732228481971,-9.23923800564499));
#30949=CARTESIAN_POINT('Ctrl Pts',(95.6507616381096,0.855426142460901,-9.23801205511989));
#30950=CARTESIAN_POINT('Ctrl Pts',(95.6343871797205,0.83946031424405,-9.23642906382491));
#30951=CARTESIAN_POINT('Ctrl Pts',(95.6305263087149,0.835643364573313,-9.23605512220094));
#30952=CARTESIAN_POINT('Ctrl Pts',(95.6243399411904,0.829442201897154,-9.23545502250654));
#30953=CARTESIAN_POINT('Ctrl Pts',(95.6219979779109,0.827074639387784,-9.23522762682557));
#30954=CARTESIAN_POINT('Ctrl Pts',(95.6174828636359,0.822471282382071,-9.23478886182069));
#30955=CARTESIAN_POINT('Ctrl Pts',(95.6153085170151,0.820236760164353,-9.23457740587272));
#30956=CARTESIAN_POINT('Ctrl Pts',(95.610071736312,0.814812117809688,-9.2340676684695));
#30957=CARTESIAN_POINT('Ctrl Pts',(95.6070183058351,0.811613291314616,-9.23377006855282));
#30958=CARTESIAN_POINT('Ctrl Pts',(95.5963341544147,0.800293417965915,-9.23272705236595));
#30959=CARTESIAN_POINT('Ctrl Pts',(95.5888004600422,0.792081046873416,-9.23198851643698));
#30960=CARTESIAN_POINT('Ctrl Pts',(95.5703933134886,0.771434918124074,-9.23017257084104));
#30961=CARTESIAN_POINT('Ctrl Pts',(95.5596624405256,0.758876738002787,-9.22910360267678));
#30962=CARTESIAN_POINT('Ctrl Pts',(95.5142318550548,0.70338781346771,-9.22451117616927));
#30963=CARTESIAN_POINT('Ctrl Pts',(95.4823079087213,0.658270608994931,-9.22110546872755));
#30964=CARTESIAN_POINT('Ctrl Pts',(95.4130661535855,0.544187317139664,-9.21285082608394));
#30965=CARTESIAN_POINT('Ctrl Pts',(95.3792394750312,0.473426349609431,-9.20800302113732));
#30966=CARTESIAN_POINT('Ctrl Pts',(95.3474189686693,0.385263793617961,-9.20189512861979));
#30967=CARTESIAN_POINT('Ctrl Pts',(95.342446799899,0.370587058396515,-9.20087685596749));
#30968=CARTESIAN_POINT('Ctrl Pts',(95.3356267486446,0.349067642520101,-9.19937964886737));
#30969=CARTESIAN_POINT('Ctrl Pts',(95.3335486392436,0.342299220968954,-9.19890814633734));
#30970=CARTESIAN_POINT('Ctrl Pts',(95.3299701140216,0.330258023865242,-9.19806809013768));
#30971=CARTESIAN_POINT('Ctrl Pts',(95.3284452343853,0.32499269135528,-9.1977003354521));
#30972=CARTESIAN_POINT('Ctrl Pts',(95.3253415942028,0.313989053433054,-9.19693082963369));
#30973=CARTESIAN_POINT('Ctrl Pts',(95.3237694649128,0.308249055451559,-9.19652887774416));
#30974=CARTESIAN_POINT('Ctrl Pts',(95.3197795457139,0.293235754425902,-9.1954760083271));
#30975=CARTESIAN_POINT('Ctrl Pts',(95.3174313588221,0.283944579297801,-9.19482289623396));
#30976=CARTESIAN_POINT('Ctrl Pts',(95.3072009027109,0.241280090969467,-9.19181613537016));
#30977=CARTESIAN_POINT('Ctrl Pts',(95.3006658508474,0.207604123923289,-9.18942063446428));
#30978=CARTESIAN_POINT('Ctrl Pts',(95.2857668404014,0.107684458492103,-9.18224382992015));
#30979=CARTESIAN_POINT('Ctrl Pts',(95.2815537781544,0.0409644271714967,
-9.17735578153224));
#30980=CARTESIAN_POINT('Ctrl Pts',(95.2843263917638,-0.0858425006856801,
-9.16804775771988));
#30981=CARTESIAN_POINT('Ctrl Pts',(95.2902396280184,-0.145757237615887,
-9.16364524380017));
#30982=CARTESIAN_POINT('Ctrl Pts',(95.3024488669829,-0.214842747839243,
-9.15872543845992));
#30983=CARTESIAN_POINT('Ctrl Pts',(95.3043210274542,-0.224699714615762,
-9.15802740159081));
#30984=CARTESIAN_POINT('Ctrl Pts',(95.307103818103,-0.23839418593838,-9.15706415567521));
#30985=CARTESIAN_POINT('Ctrl Pts',(95.3079080405473,-0.242252524822921,
-9.15679349441877));
#30986=CARTESIAN_POINT('Ctrl Pts',(95.3093288295732,-0.248901640744811,
-9.15632840163204));
#30987=CARTESIAN_POINT('Ctrl Pts',(95.309936207762,-0.251694313963008,-9.15613346858606));
#30988=CARTESIAN_POINT('Ctrl Pts',(95.3112390682229,-0.257581481905566,
-9.15572343796251));
#30989=CARTESIAN_POINT('Ctrl Pts',(95.3119368959619,-0.260675428491912,
-9.15550848052399));
#30990=CARTESIAN_POINT('Ctrl Pts',(95.3136995903661,-0.268346151201486,
-9.15497677600476));
#30991=CARTESIAN_POINT('Ctrl Pts',(95.3147793796356,-0.272919506809456,
-9.1546608597584));
#30992=CARTESIAN_POINT('Ctrl Pts',(95.3189559007996,-0.290147101585245,
-9.15347451595903));
#30993=CARTESIAN_POINT('Ctrl Pts',(95.3222352798843,-0.302756680496362,
-9.15261372299451));
#30994=CARTESIAN_POINT('Ctrl Pts',(95.3311966315269,-0.335007371820055,
-9.15042543884504));
#30995=CARTESIAN_POINT('Ctrl Pts',(95.3371821602943,-0.354560205331172,
-9.14911152636124));
#30996=CARTESIAN_POINT('Ctrl Pts',(95.3620467297682,-0.428818907265126,
-9.14413615180968));
#30997=CARTESIAN_POINT('Ctrl Pts',(95.3844393162725,-0.482264035663483,
-9.1405830800919));
#30998=CARTESIAN_POINT('Ctrl Pts',(95.4448872518983,-0.601134383103912,
-9.13232576128364));
#30999=CARTESIAN_POINT('Ctrl Pts',(95.4854873975158,-0.664965014217853,
-9.12761148916091));
#31000=CARTESIAN_POINT('Ctrl Pts',(95.538302413555,-0.732659367047439,-9.12197645673039));
#31001=CARTESIAN_POINT('Ctrl Pts',(95.544801117809,-0.740765438529941,-9.12129062762627));
#31002=CARTESIAN_POINT('Ctrl Pts',(95.555682023743,-0.753975596535628,-9.12015388854749));
#31003=CARTESIAN_POINT('Ctrl Pts',(95.5600023147449,-0.759130108362933,
-9.11970543810132));
#31004=CARTESIAN_POINT('Ctrl Pts',(95.5678891868428,-0.768377823073261,
-9.11889178407716));
#31005=CARTESIAN_POINT('Ctrl Pts',(95.5714403968185,-0.77248393365631,-9.11852721011585));
#31006=CARTESIAN_POINT('Ctrl Pts',(95.5791234004798,-0.781244306060536,
-9.1177421765769));
#31007=CARTESIAN_POINT('Ctrl Pts',(95.5832639370711,-0.785890644750674,
-9.11732136366434));
#31008=CARTESIAN_POINT('Ctrl Pts',(95.5947128477063,-0.798534929345098,
-9.11616376877424));
#31009=CARTESIAN_POINT('Ctrl Pts',(95.6020949093263,-0.806465022122779,
-9.11542392732011));
#31010=CARTESIAN_POINT('Ctrl Pts',(95.6464821035948,-0.852847502169106,
-9.11101236205437));
#31011=CARTESIAN_POINT('Ctrl Pts',(95.6859514661125,-0.888845086902073,
-9.1072345911344));
#31012=CARTESIAN_POINT('Ctrl Pts',(95.7652559284584,-0.951869766641753,
-9.09991300930379));
#31013=CARTESIAN_POINT('Ctrl Pts',(95.8045768963787,-0.979379049581392,
-9.09639177378336));
#31014=CARTESIAN_POINT('Ctrl Pts',(95.8695093277414,-1.01913819128113,-9.09080562642547));
#31015=CARTESIAN_POINT('Ctrl Pts',(95.8940778211517,-1.03299453091597,-9.08874052508318));
#31016=CARTESIAN_POINT('Ctrl Pts',(95.9498950387495,-1.06188410789788,-9.08418363042193));
#31017=CARTESIAN_POINT('Ctrl Pts',(95.9813607684307,-1.07644794516997,-9.08170432428314));
#31018=CARTESIAN_POINT('Ctrl Pts',(96.0190358030001,-1.09190567912478,-9.07887385225048));
#31019=CARTESIAN_POINT('Ctrl Pts',(96.0246634113963,-1.09416402190214,-9.07845460074052));
#31020=CARTESIAN_POINT('Ctrl Pts',(96.0338701310051,-1.09777634843818,-9.07777475470072));
#31021=CARTESIAN_POINT('Ctrl Pts',(96.0374387577416,-1.0991564978109,-9.07751271016649));
#31022=CARTESIAN_POINT('Ctrl Pts',(96.043856932835,-1.1016028081397,-9.07704413952237));
#31023=CARTESIAN_POINT('Ctrl Pts',(96.0467039351538,-1.10267533807656,-9.07683724960353));
#31024=CARTESIAN_POINT('Ctrl Pts',(96.0529870685079,-1.10501457450796,-9.07638277326989));
#31025=CARTESIAN_POINT('Ctrl Pts',(96.0564249676695,-1.10627629341864,-9.0761354785603));
#31026=CARTESIAN_POINT('Ctrl Pts',(96.0664133977201,-1.1098893024343,-9.07542082715038));
#31027=CARTESIAN_POINT('Ctrl Pts',(96.0729790918501,-1.1121986401365,-9.07495583326609));
#31028=CARTESIAN_POINT('Ctrl Pts',(96.1289905470844,-1.13134320341494,-9.07102631995454));
#31029=CARTESIAN_POINT('Ctrl Pts',(96.1794921087499,-1.14493234273633,-9.06772852293112));
#31030=CARTESIAN_POINT('Ctrl Pts',(96.312409385237,-1.1713686081228,-9.05928699315287));
#31031=CARTESIAN_POINT('Ctrl Pts',(96.3955718663988,-1.17890458442218,-9.05421956648677));
#31032=CARTESIAN_POINT('Ctrl Pts',(96.5095442979045,-1.17712838993749,-9.04694846659041));
#31033=CARTESIAN_POINT('Ctrl Pts',(96.5402225146593,-1.17544863241202,-9.04496126539066));
#31034=CARTESIAN_POINT('Ctrl Pts',(96.5803190218028,-1.17167629870942,-9.04230704886361));
#31035=CARTESIAN_POINT('Ctrl Pts',(96.5898284265352,-1.17066465473783,-9.04167338303666));
#31036=CARTESIAN_POINT('Ctrl Pts',(96.6052297671665,-1.16883626277116,-9.04063983406126));
#31037=CARTESIAN_POINT('Ctrl Pts',(96.6111298136731,-1.16809047034655,-9.04024216028685));
#31038=CARTESIAN_POINT('Ctrl Pts',(96.6224583441052,-1.16657123693149,-9.03947514356716));
#31039=CARTESIAN_POINT('Ctrl Pts',(96.6278875834212,-1.16580450521287,-9.03910601910244));
#31040=CARTESIAN_POINT('Ctrl Pts',(96.6404448233589,-1.16394161163298,-9.03824863620056));
#31041=CARTESIAN_POINT('Ctrl Pts',(96.6475684418948,-1.16281784359028,-9.03775952806478));
#31042=CARTESIAN_POINT('Ctrl Pts',(96.6702599122193,-1.15902430091659,-9.03619258634598));
#31043=CARTESIAN_POINT('Ctrl Pts',(96.6857840071798,-1.15610684349203,-9.03510708558295));
#31044=CARTESIAN_POINT('Ctrl Pts',(96.7221573549886,-1.14851075738763,-9.03253064001181));
#31045=CARTESIAN_POINT('Ctrl Pts',(96.7429466835705,-1.1435753196859,-9.0310321681964));
#31046=CARTESIAN_POINT('Ctrl Pts',(96.8211627608579,-1.12274375100132,-9.02529536512948));
#31047=CARTESIAN_POINT('Ctrl Pts',(96.8774837088491,-1.10306489479191,-9.02095383538607));
#31048=CARTESIAN_POINT('Ctrl Pts',(96.9962989981343,-1.05114576597485,-9.01144141500817));
#31049=CARTESIAN_POINT('Ctrl Pts',(97.0579015001254,-1.01739808530671,-9.00627656180522));
#31050=CARTESIAN_POINT('Ctrl Pts',(97.1242927047042,-0.972905603992704,
-9.00067475197841));
#31051=CARTESIAN_POINT('Ctrl Pts',(97.1323763299039,-0.967340671148337,
-8.99999222008305));
#31052=CARTESIAN_POINT('Ctrl Pts',(97.1435779716884,-0.959421057888762,
-8.99904678457792));
#31053=CARTESIAN_POINT('Ctrl Pts',(97.1467549973599,-0.957151106337928,
-8.99877868051539));
#31054=CARTESIAN_POINT('Ctrl Pts',(97.1522303069411,-0.953197778031151,
-8.99831678201743));
#31055=CARTESIAN_POINT('Ctrl Pts',(97.1545338560112,-0.951521802676203,
-8.99812250161839));
#31056=CARTESIAN_POINT('Ctrl Pts',(97.1593343201527,-0.94800245839582,-8.99771777073918));
#31057=CARTESIAN_POINT('Ctrl Pts',(97.1618300733611,-0.946157545923668,
-8.9975074324903));
#31058=CARTESIAN_POINT('Ctrl Pts',(97.1678524781998,-0.941668736802228,
-8.99699999122045));
#31059=CARTESIAN_POINT('Ctrl Pts',(97.1713716780376,-0.939014836468964,
-8.9967035655622));
#31060=CARTESIAN_POINT('Ctrl Pts',(97.1790357241446,-0.933167441947189,
-8.99605802801546));
#31061=CARTESIAN_POINT('Ctrl Pts',(97.1831743781743,-0.929965939927039,
-8.99570944004017));
#31062=CARTESIAN_POINT('Ctrl Pts',(97.1948426707389,-0.920814863777414,
-8.99472623318917));
#31063=CARTESIAN_POINT('Ctrl Pts',(97.2023213017794,-0.914800555213958,
-8.99409556215138));
#31064=CARTESIAN_POINT('Ctrl Pts',(97.2929932359935,-0.840038988469825,
-8.98643137536576));
#31065=CARTESIAN_POINT('Ctrl Pts',(97.3664388077481,-0.76025586850915,-8.97999646387024));
#31066=CARTESIAN_POINT('Ctrl Pts',(97.4540863476987,-0.633985087939889,
-8.97033442780474));
#31067=CARTESIAN_POINT('Ctrl Pts',(97.477962422791,-0.594911333428827,-8.96741037220426));
#31068=CARTESIAN_POINT('Ctrl Pts',(97.5045333345108,-0.545127309715428,
-8.96370132341083));
#31069=CARTESIAN_POINT('Ctrl Pts',(97.5094344125026,-0.535635871324302,
-8.96299500506957));
#31070=CARTESIAN_POINT('Ctrl Pts',(97.5169983466645,-0.520485487562804,
-8.96186818838862));
#31071=CARTESIAN_POINT('Ctrl Pts',(97.5197464772194,-0.514869587875632,
-8.96145063788746));
#31072=CARTESIAN_POINT('Ctrl Pts',(97.5247958486115,-0.504339469967128,
-8.9606678244623));
#31073=CARTESIAN_POINT('Ctrl Pts',(97.52710810395,-0.499430693029835,-8.96030295086229));
#31074=CARTESIAN_POINT('Ctrl Pts',(97.5321939444214,-0.488437337636629,
-8.95948581864335));
#31075=CARTESIAN_POINT('Ctrl Pts',(97.5349497784742,-0.482344802663101,
-8.95903297133037));
#31076=CARTESIAN_POINT('Ctrl Pts',(97.5429294590955,-0.464295736129671,
-8.95769125082671));
#31077=CARTESIAN_POINT('Ctrl Pts',(97.5480065195336,-0.452275819960613,
-8.95679749733693));
#31078=CARTESIAN_POINT('Ctrl Pts',(97.5789173118845,-0.375563045826508,
-8.95108988856989));
#31079=CARTESIAN_POINT('Ctrl Pts',(97.5991639724754,-0.308780551613872,
-8.94609295436767));
#31080=CARTESIAN_POINT('Ctrl Pts',(97.6299280764564,-0.16137194007726,-8.9350904266245));
#31081=CARTESIAN_POINT('Ctrl Pts',(97.638252237779,-0.0806385399990132,
-8.929079197479));
#31082=CARTESIAN_POINT('Ctrl Pts',(97.6382309086937,0.000310323435185096,
-8.92336488290745));
#31083=CARTESIAN_POINT('Ctrl Pts',(97.6382309083588,0.000311592030453068,
-8.92336479335523));
#31084=CARTESIAN_POINT('Ctrl Pts',(97.6382276895883,0.0124778426499294,
-8.9225059580564));
#31085=CARTESIAN_POINT('Ctrl Pts',(97.6380359531211,0.0246439812452245,
-8.92165456740108));
#31086=CARTESIAN_POINT('Ctrl Pts',(97.6375296113348,0.0408386007025197,
-8.92053300477536));
#31087=CARTESIAN_POINT('Ctrl Pts',(97.6373827885247,0.0448709939316155,
-8.92025471094953));
#31088=CARTESIAN_POINT('Ctrl Pts',(97.6370893274945,0.0519324893646293,
-8.91976915610684));
#31089=CARTESIAN_POINT('Ctrl Pts',(97.6369517093267,0.0549618996042393,
-8.91956142878702));
#31090=CARTESIAN_POINT('Ctrl Pts',(97.636657125303,0.0609374264415622,-8.91915286931953));
#31091=CARTESIAN_POINT('Ctrl Pts',(97.6365007874133,0.0638835510311558,
-8.91895200686091));
#31092=CARTESIAN_POINT('Ctrl Pts',(97.6361389968834,0.0702492204367553,
-8.9185192649837));
#31093=CARTESIAN_POINT('Ctrl Pts',(97.6359296948163,0.0736684819833694,
-8.91828759858531));
#31094=CARTESIAN_POINT('Ctrl Pts',(97.6353218691996,0.0829350650225935,
-8.91766174528768));
#31095=CARTESIAN_POINT('Ctrl Pts',(97.6348946066744,0.0887804988577374,
-8.91726909985336));
#31096=CARTESIAN_POINT('Ctrl Pts',(97.6326888707052,0.116146122393434,-8.91543995848173));
#31097=CARTESIAN_POINT('Ctrl Pts',(97.6303622920809,0.137619466719396,-8.91403086391976));
#31098=CARTESIAN_POINT('Ctrl Pts',(97.6187467021329,0.222861201831005,-8.90849877630197));
#31099=CARTESIAN_POINT('Ctrl Pts',(97.6048218237422,0.285888264249353,-8.90454185578871));
#31100=CARTESIAN_POINT('Ctrl Pts',(97.5634371774038,0.419920242698919,-8.89586072487024));
#31101=CARTESIAN_POINT('Ctrl Pts',(97.5341231161294,0.490036592359137,-8.89113791524995));
#31102=CARTESIAN_POINT('Ctrl Pts',(97.4920792842694,0.568393992170254,-8.8853190825196));
#31103=CARTESIAN_POINT('Ctrl Pts',(97.4856901193522,0.579838762393659,-8.88445518669768));
#31104=CARTESIAN_POINT('Ctrl Pts',(97.4757490374506,0.596967876397367,-8.88313962084845));
#31105=CARTESIAN_POINT('Ctrl Pts',(97.4723372783363,0.602732695763284,-8.88269292527567));
#31106=CARTESIAN_POINT('Ctrl Pts',(97.4660728559163,0.613114533831275,-8.88188114088289));
#31107=CARTESIAN_POINT('Ctrl Pts',(97.4632370853661,0.61774156744024,-8.88151666830515));
#31108=CARTESIAN_POINT('Ctrl Pts',(97.4570703848893,0.627649216240995,-8.88073038011151));
#31109=CARTESIAN_POINT('Ctrl Pts',(97.4537292535835,0.632923253816214,-8.88030820072308));
#31110=CARTESIAN_POINT('Ctrl Pts',(97.4445797007711,0.647115115993269,-8.87916216788381));
#31111=CARTESIAN_POINT('Ctrl Pts',(97.4386921939768,0.655981001165737,-8.87843542538287));
#31112=CARTESIAN_POINT('Ctrl Pts',(97.4072312126746,0.701991967803485,-8.87460575947559));
#31113=CARTESIAN_POINT('Ctrl Pts',(97.3796630547364,0.737720903967526,-8.87142867429431));
#31114=CARTESIAN_POINT('Ctrl Pts',(97.2791439462794,0.853590358476638,-8.86040950179982));
#31115=CARTESIAN_POINT('Ctrl Pts',(97.1972327732983,0.925213385596874,-8.85227200437735));
#31116=CARTESIAN_POINT('Ctrl Pts',(97.0985135410843,0.990002638551259,-8.84392264336416));
#31117=CARTESIAN_POINT('Ctrl Pts',(97.0902659467377,0.99526965372209,-8.84323545128999));
#31118=CARTESIAN_POINT('Ctrl Pts',(97.0774484045568,1.00323195139268,-8.84218443958758));
#31119=CARTESIAN_POINT('Ctrl Pts',(97.0729244866847,1.00600005227844,-8.84181669158475));
#31120=CARTESIAN_POINT('Ctrl Pts',(97.0644822237792,1.0110876588527,-8.84113656880563));
#31121=CARTESIAN_POINT('Ctrl Pts',(97.060568847061,1.01341517165003,-8.84082372806416));
#31122=CARTESIAN_POINT('Ctrl Pts',(97.0539597647108,1.01729426972501,-8.84029958641083));
#31123=CARTESIAN_POINT('Ctrl Pts',(97.051271263729,1.01885795902174,-8.84008753116873));
#31124=CARTESIAN_POINT('Ctrl Pts',(97.0461022073597,1.02183705202581,-8.83968208750244));
#31125=CARTESIAN_POINT('Ctrl Pts',(97.0436226540505,1.02325410891238,-8.83948859078269));
#31126=CARTESIAN_POINT('Ctrl Pts',(97.0377160768376,1.02660125638527,-8.8390299511251));
#31127=CARTESIAN_POINT('Ctrl Pts',(97.0342844636194,1.02852324238589,-8.8387653142942));
#31128=CARTESIAN_POINT('Ctrl Pts',(97.0221083623426,1.03526295500918,-8.83783252987749));
#31129=CARTESIAN_POINT('Ctrl Pts',(97.0133120188657,1.03998680846358,-8.83716992620203));
#31130=CARTESIAN_POINT('Ctrl Pts',(96.9539772956563,1.07088540751493,-8.8327681510595));
#31131=CARTESIAN_POINT('Ctrl Pts',(96.9016525248316,1.09348226976643,-8.8292107009021));
#31132=CARTESIAN_POINT('Ctrl Pts',(96.7825310760637,1.13497545290733,-8.82138807095433));
#31133=CARTESIAN_POINT('Ctrl Pts',(96.715293193805,1.15193564854449,-8.81714607711188));
#31134=CARTESIAN_POINT('Ctrl Pts',(96.6240770276374,1.16656261123013,-8.81127695664107));
#31135=CARTESIAN_POINT('Ctrl Pts',(96.6010952461265,1.16955526613333,-8.80978976997621));
#31136=CARTESIAN_POINT('Ctrl Pts',(96.56132016922,1.17354544884839,-8.80719032863235));
#31137=CARTESIAN_POINT('Ctrl Pts',(96.5445658886967,1.17486473510556,-8.80608765129259));
#31138=CARTESIAN_POINT('Ctrl Pts',(96.5204114854098,1.17624742758363,-8.80448418320723));
#31139=CARTESIAN_POINT('Ctrl Pts',(96.5130295297029,1.1766003240665,-8.80399229991763));
#31140=CARTESIAN_POINT('Ctrl Pts',(96.5001387082074,1.17709502048667,-8.80312991557893));
#31141=CARTESIAN_POINT('Ctrl Pts',(96.4946312029094,1.17726767708703,-8.80276037754926));
#31142=CARTESIAN_POINT('Ctrl Pts',(96.4832508565428,1.17754451872483,-8.80199444203392));
#31143=CARTESIAN_POINT('Ctrl Pts',(96.4773780527988,1.17764342990208,-8.80159789217506));
#31144=CARTESIAN_POINT('Ctrl Pts',(96.4622802390568,1.17778475362582,-8.80057500305499));
#31145=CARTESIAN_POINT('Ctrl Pts',(96.453055171937,1.17776271495903,-8.79994669585846));
#31146=CARTESIAN_POINT('Ctrl Pts',(96.4160964373965,1.17724019093933,-8.79741567913715));
#31147=CARTESIAN_POINT('Ctrl Pts',(96.3883860345321,1.1758684252349,-8.79548656255368));
#31148=CARTESIAN_POINT('Ctrl Pts',(96.2646127433491,1.16534980695569,-8.78672288011929));
#31149=CARTESIAN_POINT('Ctrl Pts',(96.1698511337788,1.14539668457812,-8.77957436320877));
#31150=CARTESIAN_POINT('Ctrl Pts',(96.0509117732827,1.1046289492316,-8.77040832924488));
#31151=CARTESIAN_POINT('Ctrl Pts',(96.0235809783956,1.0941072481382,-8.76829155837132));
#31152=CARTESIAN_POINT('Ctrl Pts',(95.9812832004364,1.07598548108368,-8.76502541241066));
#31153=CARTESIAN_POINT('Ctrl Pts',(95.9660386378216,1.06906599881069,-8.76385039570325));
#31154=CARTESIAN_POINT('Ctrl Pts',(95.9462971708132,1.05959270031176,-8.76233625385094));
#31155=CARTESIAN_POINT('Ctrl Pts',(95.941663089498,1.05733139526956,-8.76198137666944));
#31156=CARTESIAN_POINT('Ctrl Pts',(95.9341146724985,1.05358639762704,-8.76140439909831));
#31157=CARTESIAN_POINT('Ctrl Pts',(95.9311914618543,1.05212090263434,-8.76118122435437));
#31158=CARTESIAN_POINT('Ctrl Pts',(95.9261134092303,1.0495485992528,-8.76079404995843));
#31159=CARTESIAN_POINT('Ctrl Pts',(95.9239558417446,1.04844729918809,-8.76062971140502));
#31160=CARTESIAN_POINT('Ctrl Pts',(95.9218016730721,1.04733934308043,-8.76046578184569));
#31161=CARTESIAN_POINT('Ctrl Pts',(95.921801762405,1.04733938902713,-8.66210246100831));
#31162=CARTESIAN_POINT('Ctrl Pts',(96.0026452746676,1.08891971908056,-8.66861620224818));
#31163=CARTESIAN_POINT('Ctrl Pts',(96.0880613387606,1.12101445553017,-8.67538701849297));
#31164=CARTESIAN_POINT('Ctrl Pts',(96.1973600557611,1.1481862295067,-8.68353275506134));
#31165=CARTESIAN_POINT('Ctrl Pts',(96.2185218236774,1.15283134845987,-8.68508516595406));
#31166=CARTESIAN_POINT('Ctrl Pts',(96.2531391665135,1.15943470315772,-8.68757302155445));
#31167=CARTESIAN_POINT('Ctrl Pts',(96.266521185894,1.16174829267295,-8.68852232754309));
#31168=CARTESIAN_POINT('Ctrl Pts',(96.2846579683376,1.16456177497881,-8.68978959231629));
#31169=CARTESIAN_POINT('Ctrl Pts',(96.2893795233907,1.16526484217128,-8.69011773593559));
#31170=CARTESIAN_POINT('Ctrl Pts',(96.2972602562689,1.16638939640873,-8.6906623568494));
#31171=CARTESIAN_POINT('Ctrl Pts',(96.3004170587716,1.16682679535453,-8.69087969365735));
#31172=CARTESIAN_POINT('Ctrl Pts',(96.3063948843866,1.16763035190628,-8.69128964389267));
#31173=CARTESIAN_POINT('Ctrl Pts',(96.309215516796,1.1679991110707,-8.69148240421451));
#31174=CARTESIAN_POINT('Ctrl Pts',(96.3158952565737,1.16884779267269,-8.69193735710874));
#31175=CARTESIAN_POINT('Ctrl Pts',(96.3197554893138,1.16931883203664,-8.69219906264013));
#31176=CARTESIAN_POINT('Ctrl Pts',(96.3333724455114,1.17091201264814,-8.69311818073018));
#31177=CARTESIAN_POINT('Ctrl Pts',(96.3431411238883,1.17193126671885,-8.69377023082555));
#31178=CARTESIAN_POINT('Ctrl Pts',(96.4231719686491,1.17927083242644,-8.69906081889157));
#31179=CARTESIAN_POINT('Ctrl Pts',(96.4938691601936,1.17938952544481,-8.70341612414954));
#31180=CARTESIAN_POINT('Ctrl Pts',(96.6232038990814,1.16795964666036,-8.71144754105458));
#31181=CARTESIAN_POINT('Ctrl Pts',(96.6817658415168,1.1582922052049,-8.71510942033331));
#31182=CARTESIAN_POINT('Ctrl Pts',(96.7600454756172,1.13921461501162,-8.7202441729295));
#31183=CARTESIAN_POINT('Ctrl Pts',(96.7806002045575,1.13361035000759,-8.72161502937965));
#31184=CARTESIAN_POINT('Ctrl Pts',(96.8160771968344,1.12289569042697,-8.72402898261375));
#31185=CARTESIAN_POINT('Ctrl Pts',(96.8310700204213,1.11803717517318,-8.72506429855792));
#31186=CARTESIAN_POINT('Ctrl Pts',(96.8527683615087,1.11052130090468,-8.72658706548817));
#31187=CARTESIAN_POINT('Ctrl Pts',(96.8595545184739,1.10810074274621,-8.72706683106561));
#31188=CARTESIAN_POINT('Ctrl Pts',(96.8714639462168,1.10372917362666,-8.72791522153835));
#31189=CARTESIAN_POINT('Ctrl Pts',(96.876596650974,1.10180435357681,-8.72828297735421));
#31190=CARTESIAN_POINT('Ctrl Pts',(96.8872713451955,1.09771599874422,-8.72905233389177));
#31191=CARTESIAN_POINT('Ctrl Pts',(96.8928107401524,1.09554616773264,-8.7294541343246));
#31192=CARTESIAN_POINT('Ctrl Pts',(96.9072217739639,1.08977491832561,-8.73050626607426));
#31193=CARTESIAN_POINT('Ctrl Pts',(96.9160662032585,1.0861071788856,-8.73115878659929));
#31194=CARTESIAN_POINT('Ctrl Pts',(96.953197770417,1.0701755653839,-8.73392776786964));
#31195=CARTESIAN_POINT('Ctrl Pts',(96.9810400775148,1.05691224719204,-8.73607735087099));
#31196=CARTESIAN_POINT('Ctrl Pts',(97.0819626491045,1.00387986758731,-8.74415021342976));
#31197=CARTESIAN_POINT('Ctrl Pts',(97.1512834224217,0.957498228828896,-8.7502811304991));
#31198=CARTESIAN_POINT('Ctrl Pts',(97.2552030990649,0.870767548907848,-8.76018962993834));
#31199=CARTESIAN_POINT('Ctrl Pts',(97.2930132780533,0.834691945012636,-8.76397653379108));
#31200=CARTESIAN_POINT('Ctrl Pts',(97.3330129195074,0.791095092138699,-8.76809170927561));
#31201=CARTESIAN_POINT('Ctrl Pts',(97.3376718568838,0.785925951567453,-8.76857280931927));
#31202=CARTESIAN_POINT('Ctrl Pts',(97.3447120756631,0.777974154780736,-8.76930216092445));
#31203=CARTESIAN_POINT('Ctrl Pts',(97.3471265506215,0.775221290285062,-8.76955272602837));
#31204=CARTESIAN_POINT('Ctrl Pts',(97.3515234101857,0.770160794970356,-8.77000973662444));
#31205=CARTESIAN_POINT('Ctrl Pts',(97.3535097008062,0.76785673575338,-8.77021645811504));
#31206=CARTESIAN_POINT('Ctrl Pts',(97.3579739539885,0.762637533034789,-8.77068169363572));
#31207=CARTESIAN_POINT('Ctrl Pts',(97.3604466542095,0.759717994573912,-8.77093982949921));
#31208=CARTESIAN_POINT('Ctrl Pts',(97.3668012330325,0.752140525536331,-8.77160453089989));
#31209=CARTESIAN_POINT('Ctrl Pts',(97.3706615049553,0.747464505368721,-8.77200961239814));
#31210=CARTESIAN_POINT('Ctrl Pts',(97.3963404878921,0.715865134402268,-8.7747146272142));
#31211=CARTESIAN_POINT('Ctrl Pts',(97.4170001286997,0.688017101278722,-8.77694197076325));
#31212=CARTESIAN_POINT('Ctrl Pts',(97.4521644223828,0.635965151452648,-8.78091117087153));
#31213=CARTESIAN_POINT('Ctrl Pts',(97.4670844960221,0.612076142840339,-8.78266435391822));
#31214=CARTESIAN_POINT('Ctrl Pts',(97.5050231779529,0.546185502445568,-8.78737858818703));
#31215=CARTESIAN_POINT('Ctrl Pts',(97.5263594562209,0.503279234907906,-8.79032268798985));
#31216=CARTESIAN_POINT('Ctrl Pts',(97.5658709742785,0.409959225388626,-8.79665941474394));
#31217=CARTESIAN_POINT('Ctrl Pts',(97.5833376457288,0.359368087666697,-8.80005784508494));
#31218=CARTESIAN_POINT('Ctrl Pts',(97.600138935057,0.297308263386022,-8.80428344482528));
#31219=CARTESIAN_POINT('Ctrl Pts',(97.6028265324198,0.286808444625609,-8.80500010931137));
#31220=CARTESIAN_POINT('Ctrl Pts',(97.6068287985501,0.270222891142982,-8.80613558140108));
#31221=CARTESIAN_POINT('Ctrl Pts',(97.6082408179135,0.264161094544596,-8.80655129495597));
#31222=CARTESIAN_POINT('Ctrl Pts',(97.610794211434,0.252792260657839,-8.80733242701998));
#31223=CARTESIAN_POINT('Ctrl Pts',(97.6119470757702,0.247487951207393,-8.80769747089252));
#31224=CARTESIAN_POINT('Ctrl Pts',(97.6144457408349,0.235596113074426,-8.8085172898266));
#31225=CARTESIAN_POINT('Ctrl Pts',(97.6157718721288,0.229004692063425,-8.80897267196527));
#31226=CARTESIAN_POINT('Ctrl Pts',(97.6190022366783,0.2122058076789,-8.81013589345186));
#31227=CARTESIAN_POINT('Ctrl Pts',(97.620828016972,0.201984030810402,-8.81084615992917));
#31228=CARTESIAN_POINT('Ctrl Pts',(97.6330339133282,0.128010272761377,-8.81600535362275));
#31229=CARTESIAN_POINT('Ctrl Pts',(97.6382873521505,0.0635346200625748,
-8.82061337127098));
#31230=CARTESIAN_POINT('Ctrl Pts',(97.6381857070302,-0.0518979240526905,
-8.82901867298229));
#31231=CARTESIAN_POINT('Ctrl Pts',(97.6348463079867,-0.102702002495823,
-8.83276932423325));
#31232=CARTESIAN_POINT('Ctrl Pts',(97.6221331347851,-0.199651755711864,
-8.83991300674831));
#31233=CARTESIAN_POINT('Ctrl Pts',(97.6132571065783,-0.245773838948051,
-8.84330439417029));
#31234=CARTESIAN_POINT('Ctrl Pts',(97.6000755396993,-0.297421981170072,
-8.8470129608494));
#31235=CARTESIAN_POINT('Ctrl Pts',(97.5984496763939,-0.303583342707689,
-8.84745387802189));
#31236=CARTESIAN_POINT('Ctrl Pts',(97.595743393164,-0.313511721550963,-8.84816162059654));
#31237=CARTESIAN_POINT('Ctrl Pts',(97.5946940656155,-0.317286974029813,
-8.84843009375209));
#31238=CARTESIAN_POINT('Ctrl Pts',(97.592795103803,-0.323989207806551,-8.84890548276808));
#31239=CARTESIAN_POINT('Ctrl Pts',(97.5919529295628,-0.326918200587228,
-8.84911281083175));
#31240=CARTESIAN_POINT('Ctrl Pts',(97.5900943410519,-0.333288952834766,
-8.84956282566048));
#31241=CARTESIAN_POINT('Ctrl Pts',(97.5890735615615,-0.336729353213197,
-8.84980526064934));
#31242=CARTESIAN_POINT('Ctrl Pts',(97.5861271996069,-0.346495753401351,
-8.85049194277615));
#31243=CARTESIAN_POINT('Ctrl Pts',(97.5841640073638,-0.352810399453397,
-8.85093410273578));
#31244=CARTESIAN_POINT('Ctrl Pts',(97.5702126224545,-0.396387231014497,
-8.85397490603897));
#31245=CARTESIAN_POINT('Ctrl Pts',(97.5564250981301,-0.433052362258197,
-8.85648037560189));
#31246=CARTESIAN_POINT('Ctrl Pts',(97.5097107399221,-0.540667867192817,
-8.86386262415609));
#31247=CARTESIAN_POINT('Ctrl Pts',(97.4715252860834,-0.609093588533009,
-8.86860707027188));
#31248=CARTESIAN_POINT('Ctrl Pts',(97.3999750429592,-0.711796911411264,
-8.87646733590535));
#31249=CARTESIAN_POINT('Ctrl Pts',(97.3708276890198,-0.748713577394931,
-8.8794678433591));
#31250=CARTESIAN_POINT('Ctrl Pts',(97.3324001863698,-0.791812798322973,
-8.88326254688917));
#31251=CARTESIAN_POINT('Ctrl Pts',(97.3251355717588,-0.799739354371371,
-8.88397340470888));
#31252=CARTESIAN_POINT('Ctrl Pts',(97.3134659407791,-0.812127423533355,
-8.88510582237831));
#31253=CARTESIAN_POINT('Ctrl Pts',(97.3091319569148,-0.816655259246756,
-8.88552438355297));
#31254=CARTESIAN_POINT('Ctrl Pts',(97.3013583782963,-0.824647830939835,
-8.88627171676063));
#31255=CARTESIAN_POINT('Ctrl Pts',(97.2979329665957,-0.82812620606204,-8.88659987326107));
#31256=CARTESIAN_POINT('Ctrl Pts',(97.2899486553138,-0.836133771616152,
-8.88736218769851));
#31257=CARTESIAN_POINT('Ctrl Pts',(97.2853741495215,-0.840647110716185,
-8.88779702256677));
#31258=CARTESIAN_POINT('Ctrl Pts',(97.2723060671461,-0.853331083643872,
-8.88903398477828));
#31259=CARTESIAN_POINT('Ctrl Pts',(97.2637266657072,-0.861411784139035,
-8.88983990832325));
#31260=CARTESIAN_POINT('Ctrl Pts',(97.1936635394484,-0.925445433698404,
-8.8963746517436));
#31261=CARTESIAN_POINT('Ctrl Pts',(97.126545887193,-0.974863275694764,-8.90237486083419));
#31262=CARTESIAN_POINT('Ctrl Pts',(96.9903447759414,-1.05447304683196,-8.91394057979042));
#31263=CARTESIAN_POINT('Ctrl Pts',(96.922446900855,-1.08593665415552,-8.91945601027064));
#31264=CARTESIAN_POINT('Ctrl Pts',(96.842967863557,-1.11395286756346,-8.92535992027495));
#31265=CARTESIAN_POINT('Ctrl Pts',(96.833874452062,-1.11703381215986,-8.92602741084338));
#31266=CARTESIAN_POINT('Ctrl Pts',(96.8210655382787,-1.12119970544098,-8.92695550341283));
#31267=CARTESIAN_POINT('Ctrl Pts',(96.8173811112285,-1.12237796697934,-8.92722106710744));
#31268=CARTESIAN_POINT('Ctrl Pts',(96.8107130433086,-1.1244742268811,-8.9276990784321));
#31269=CARTESIAN_POINT('Ctrl Pts',(96.8077314367788,-1.12539855443997,-8.92791188208985));
#31270=CARTESIAN_POINT('Ctrl Pts',(96.8016266293524,-1.12726453332523,-8.92834563196215));
#31271=CARTESIAN_POINT('Ctrl Pts',(96.798503135777,-1.12820508118679,-8.92856651470408));
#31272=CARTESIAN_POINT('Ctrl Pts',(96.7904663083689,-1.13058876171693,-8.92913227078558));
#31273=CARTESIAN_POINT('Ctrl Pts',(96.7855473337465,-1.13201286804066,-8.92947607253095));
#31274=CARTESIAN_POINT('Ctrl Pts',(96.7648154269111,-1.13786874069433,-8.93091532125131));
#31275=CARTESIAN_POINT('Ctrl Pts',(96.7489191217967,-1.14200185305585,-8.93199504986969));
#31276=CARTESIAN_POINT('Ctrl Pts',(96.7052540704864,-1.15238494866848,-8.93490924530784));
#31277=CARTESIAN_POINT('Ctrl Pts',(96.677336012989,-1.15796332289593,-8.93671610637991));
#31278=CARTESIAN_POINT('Ctrl Pts',(96.5634931877829,-1.17644811160953,-8.9439547395685));
#31279=CARTESIAN_POINT('Ctrl Pts',(96.4764689390601,-1.1808414794972,-8.94921309518676));
#31280=CARTESIAN_POINT('Ctrl Pts',(96.3531593540693,-1.17342275468991,-8.95704253774371));
#31281=CARTESIAN_POINT('Ctrl Pts',(96.3166932962594,-1.16951425198565,-8.95940223384516));
#31282=CARTESIAN_POINT('Ctrl Pts',(96.2704201922636,-1.16235769593161,-8.96248394779818));
#31283=CARTESIAN_POINT('Ctrl Pts',(96.2603898597982,-1.16067310209854,-8.96315719026119));
#31284=CARTESIAN_POINT('Ctrl Pts',(96.2444011709794,-1.15777439442056,-8.96423932142411));
#31285=CARTESIAN_POINT('Ctrl Pts',(96.2384280708523,-1.15664365117532,-8.96464559415983));
#31286=CARTESIAN_POINT('Ctrl Pts',(96.2271182292784,-1.15441179582903,-8.96541879096145));
#31287=CARTESIAN_POINT('Ctrl Pts',(96.2217798369081,-1.15331978682177,-8.96578541936212));
#31288=CARTESIAN_POINT('Ctrl Pts',(96.209651848317,-1.15075110357181,-8.96662223763662));
#31289=CARTESIAN_POINT('Ctrl Pts',(96.2028674087887,-1.14925132170226,-8.96709314594343));
#31290=CARTESIAN_POINT('Ctrl Pts',(96.1820837443378,-1.14446356151313,-8.96854453698026));
#31291=CARTESIAN_POINT('Ctrl Pts',(96.1681315890108,-1.14097925799956,-8.96953117834694));
#31292=CARTESIAN_POINT('Ctrl Pts',(96.1004376446571,-1.12275077657516,-8.97438059094485));
#31293=CARTESIAN_POINT('Ctrl Pts',(96.047732075131,-1.10446242725119,-8.97835422834948));
#31294=CARTESIAN_POINT('Ctrl Pts',(95.9533692625956,-1.06401942127327,-8.98581298357337));
#31295=CARTESIAN_POINT('Ctrl Pts',(95.9113592283587,-1.04295956951831,-8.98926897422103));
#31296=CARTESIAN_POINT('Ctrl Pts',(95.8231962375153,-0.991956469866126,
-8.99673154841249));
#31297=CARTESIAN_POINT('Ctrl Pts',(95.7776470957344,-0.961170537998989,
-9.00072390880263));
#31298=CARTESIAN_POINT('Ctrl Pts',(95.7293417335712,-0.92334820751348,-9.00499318991353));
#31299=CARTESIAN_POINT('Ctrl Pts',(95.7243078949355,-0.919339819495835,
-9.0054385021301));
#31300=CARTESIAN_POINT('Ctrl Pts',(95.716247524516,-0.912812779271459,-9.0061518914059));
#31301=CARTESIAN_POINT('Ctrl Pts',(95.713200411131,-0.910319921218946,-9.00642165760369));
#31302=CARTESIAN_POINT('Ctrl Pts',(95.7078155141216,-0.905869252183274,
-9.00689844664392));
#31303=CARTESIAN_POINT('Ctrl Pts',(95.705472771868,-0.90391759144402,-9.00710589134667));
#31304=CARTESIAN_POINT('Ctrl Pts',(95.7003995353483,-0.899657761856323,
-9.00755513339919));
#31305=CARTESIAN_POINT('Ctrl Pts',(95.6976719574077,-0.897346247020134,
-9.00779668637519));
#31306=CARTESIAN_POINT('Ctrl Pts',(95.6899772717571,-0.890764866611322,
-9.00847832761034));
#31307=CARTESIAN_POINT('Ctrl Pts',(95.685035103162,-0.886465853405737,-9.00891637670522));
#31308=CARTESIAN_POINT('Ctrl Pts',(95.6520568623407,-0.857292418303717,
-9.01184309335455));
#31309=CARTESIAN_POINT('Ctrl Pts',(95.6251829805327,-0.831130390173551,
-9.01424641764324));
#31310=CARTESIAN_POINT('Ctrl Pts',(95.5636988577416,-0.765274172404805,
-9.01992516067165));
#31311=CARTESIAN_POINT('Ctrl Pts',(95.5304130895609,-0.724456286997456,
-9.02315645332247));
#31312=CARTESIAN_POINT('Ctrl Pts',(95.4577096039204,-0.621994394564452,
-9.03093980649257));
#31313=CARTESIAN_POINT('Ctrl Pts',(95.4210881083236,-0.558648222203954,
-9.03550849996856));
#31314=CARTESIAN_POINT('Ctrl Pts',(95.386197010051,-0.482823429841529,-9.04098566184126));
#31315=CARTESIAN_POINT('Ctrl Pts',(95.3819519172179,-0.473264790652232,
-9.04167599163561));
#31316=CARTESIAN_POINT('Ctrl Pts',(95.3751789246654,-0.457449549611166,
-9.04281863079031));
#31317=CARTESIAN_POINT('Ctrl Pts',(95.3725764357243,-0.451225377475119,
-9.04326843524873));
#31318=CARTESIAN_POINT('Ctrl Pts',(95.3679760934093,-0.439951912217908,
-9.04408350902235));
#31319=CARTESIAN_POINT('Ctrl Pts',(95.3659593992626,-0.434910473575024,
-9.04444813821783));
#31320=CARTESIAN_POINT('Ctrl Pts',(95.3617119734176,-0.424075860306241,
-9.04523213973406));
#31321=CARTESIAN_POINT('Ctrl Pts',(95.3594920473265,-0.418278654535147,
-9.04565185721066));
#31322=CARTESIAN_POINT('Ctrl Pts',(95.3535489632979,-0.40238348462306,-9.04680343263187));
#31323=CARTESIAN_POINT('Ctrl Pts',(95.349918303695,-0.39225181604212,-9.04753829748996));
#31324=CARTESIAN_POINT('Ctrl Pts',(95.3296008541513,-0.333009770201912,
-9.05184133235174));
#31325=CARTESIAN_POINT('Ctrl Pts',(95.3160363395497,-0.282896575225514,
-9.05550939519109));
#31326=CARTESIAN_POINT('Ctrl Pts',(95.291379816098,-0.160212360778678,-9.06454386764575));
#31327=CARTESIAN_POINT('Ctrl Pts',(95.2836782018558,-0.0871763788865241,
-9.06997315389065));
#31328=CARTESIAN_POINT('Ctrl Pts',(95.2825938975948,0.0046540075335601,
-9.07665259779763));
#31329=CARTESIAN_POINT('Ctrl Pts',(95.2828135099476,0.0232169289674477,
-9.07799447330159));
#31330=CARTESIAN_POINT('Ctrl Pts',(95.2842545183918,0.0638244603832813,
-9.08090230399666));
#31331=CARTESIAN_POINT('Ctrl Pts',(95.2856571515968,0.0858567077776324,
-9.08246216078433));
#31332=CARTESIAN_POINT('Ctrl Pts',(95.2882186663797,0.113714676535725,-9.08440165798949));
#31333=CARTESIAN_POINT('Ctrl Pts',(95.2888031843305,0.119587233140062,-9.08480865167357));
#31334=CARTESIAN_POINT('Ctrl Pts',(95.2897976628285,0.128870086636871,-9.08544879429877));
#31335=CARTESIAN_POINT('Ctrl Pts',(95.290178431839,0.132283312783194,-9.08568348380922));
#31336=CARTESIAN_POINT('Ctrl Pts',(95.290928640726,0.138751312871955,-9.08612685445825));
#31337=CARTESIAN_POINT('Ctrl Pts',(95.2912951180347,0.141806281616544,-9.08633568297616));
#31338=CARTESIAN_POINT('Ctrl Pts',(95.2921869840546,0.149002336107572,-9.08682625900769));
#31339=CARTESIAN_POINT('Ctrl Pts',(95.2927224212851,0.15314211363836,-9.08710744963118));
#31340=CARTESIAN_POINT('Ctrl Pts',(95.2945673128121,0.16683344497711,-9.08803427043197));
#31341=CARTESIAN_POINT('Ctrl Pts',(95.2959720762489,0.176372065257464,-9.0886748968747));
#31342=CARTESIAN_POINT('Ctrl Pts',(95.3046118192007,0.230424255908912,-9.09228172881294));
#31343=CARTESIAN_POINT('Ctrl Pts',(95.314282469017,0.274515485252917,-9.09513427424002));
#31344=CARTESIAN_POINT('Ctrl Pts',(95.3300461253124,0.330739571111064,-9.09877817154008));
#31345=CARTESIAN_POINT('Ctrl Pts',(95.3338488197845,0.343469953300518,-9.09960360304719));
#31346=CARTESIAN_POINT('Ctrl Pts',(95.3666718678334,0.446935783694662,-9.10633365250383));
#31347=CARTESIAN_POINT('Ctrl Pts',(95.4063835015753,0.533897345921919,-9.11216097206476));
#31348=CARTESIAN_POINT('Ctrl Pts',(95.4636995518088,0.62748055799282,-9.11932437364334));
#31349=CARTESIAN_POINT('Ctrl Pts',(95.4714942850816,0.639695515979718,-9.12027770664394));
#31350=CARTESIAN_POINT('Ctrl Pts',(95.4833687995423,0.657567850032197,-9.12170171611157));
#31351=CARTESIAN_POINT('Ctrl Pts',(95.4872768641221,0.663338100593111,-9.12216607465751));
#31352=CARTESIAN_POINT('Ctrl Pts',(95.4943326955004,0.67355944827148,-9.12299707094115));
#31353=CARTESIAN_POINT('Ctrl Pts',(95.4974606153455,0.678024050726204,-9.12336295772801));
#31354=CARTESIAN_POINT('Ctrl Pts',(95.5041352036542,0.687411586742202,-9.12413857113665));
#31355=CARTESIAN_POINT('Ctrl Pts',(95.5076891354094,0.692329135463135,-9.12454856621731));
#31356=CARTESIAN_POINT('Ctrl Pts',(95.517269665803,0.705372155491361,-9.12564607069554));
#31357=CARTESIAN_POINT('Ctrl Pts',(95.5233631154638,0.713447655751167,-9.12633612932253));
#31358=CARTESIAN_POINT('Ctrl Pts',(95.5546588761258,0.753830432212282,-9.12984155859137));
#31359=CARTESIAN_POINT('Ctrl Pts',(95.58142815977,0.784881806145456,-9.13271783672671));
#31360=CARTESIAN_POINT('Ctrl Pts',(95.6787011198604,0.886484168771322,-9.14277850183074));
#31361=CARTESIAN_POINT('Ctrl Pts',(95.7564981755249,0.94944129940154,-9.15022718970229));
#31362=CARTESIAN_POINT('Ctrl Pts',(95.8632688936181,1.01543122228265,-9.15925078542189));
#31363=CARTESIAN_POINT('Ctrl Pts',(95.8856933115311,1.02829091681967,-9.1610842947984));
#31364=CARTESIAN_POINT('Ctrl Pts',(95.9129354082631,1.04274343654859,-9.16322435212941));
#31365=CARTESIAN_POINT('Ctrl Pts',(95.9173612125742,1.0450554758084,-9.16356934140438));
#31366=CARTESIAN_POINT('Ctrl Pts',(95.9218016730733,1.04733934308103,-9.1639126954948));
#31367=CARTESIAN_POINT('Origin',(96.460480949577,-7.19464945638997E-16,
0.924367114736168));
#31368=CARTESIAN_POINT('',(95.9218016501122,1.04733933127144,-9.76219702307975));
#31369=CARTESIAN_POINT('',(95.9218016730721,1.04733934308042,-9.66286811608663));
#31370=CARTESIAN_POINT('',(95.9218016730721,1.04733934308042,0.924367114736168));
#31371=CARTESIAN_POINT('Ctrl Pts',(95.9218016501122,1.04733933127145,-9.76219702307975));
#31372=CARTESIAN_POINT('Ctrl Pts',(95.8859551904519,1.02890237850787,-9.75965259857021));
#31373=CARTESIAN_POINT('Ctrl Pts',(95.8510742174078,1.00863488510987,-9.75706685301096));
#31374=CARTESIAN_POINT('Ctrl Pts',(95.8082201404791,0.980697856469402,-9.75370467124793));
#31375=CARTESIAN_POINT('Ctrl Pts',(95.7992262958196,0.974656205474092,-9.75298824003682));
#31376=CARTESIAN_POINT('Ctrl Pts',(95.7851994043365,0.964950067071735,-9.75185302554793));
#31377=CARTESIAN_POINT('Ctrl Pts',(95.7801097237193,0.961368186389378,-9.75143733331187));
#31378=CARTESIAN_POINT('Ctrl Pts',(95.7706339977982,0.9545866740277,-9.75065617333148));
#31379=CARTESIAN_POINT('Ctrl Pts',(95.7662412058318,0.951396716214778,-9.75029107974152));
#31380=CARTESIAN_POINT('Ctrl Pts',(95.7564559991169,0.944187040075249,-9.74947105952465));
#31381=CARTESIAN_POINT('Ctrl Pts',(95.7510756834141,0.940151297724262,-9.74901552497651));
#31382=CARTESIAN_POINT('Ctrl Pts',(95.737472929536,0.929764703474581,-9.74785173960773));
#31383=CARTESIAN_POINT('Ctrl Pts',(95.7292995630512,0.923350837376153,-9.74714105803139));
#31384=CARTESIAN_POINT('Ctrl Pts',(95.6624215877496,0.869425032570293,-9.74122918043905));
#31385=CARTESIAN_POINT('Ctrl Pts',(95.6083377002103,0.816484307829847,-9.73580597333349));
#31386=CARTESIAN_POINT('Ctrl Pts',(95.5223932718477,0.714450945155771,-9.72604671231284));
#31387=CARTESIAN_POINT('Ctrl Pts',(95.4884028671743,0.667467678364804,-9.7217694792751));
#31388=CARTESIAN_POINT('Ctrl Pts',(95.44729189965,0.600799206543354,-9.71611408146137));
#31389=CARTESIAN_POINT('Ctrl Pts',(95.4370306462928,0.583147762462043,-9.71465352815616));
#31390=CARTESIAN_POINT('Ctrl Pts',(95.4209874716981,0.553821011983468,-9.71229615852173));
#31391=CARTESIAN_POINT('Ctrl Pts',(95.4149313973869,0.542301182802119,-9.71138711082909));
#31392=CARTESIAN_POINT('Ctrl Pts',(95.4069508619269,0.526489769144039,-9.71016458051316));
#31393=CARTESIAN_POINT('Ctrl Pts',(95.4048595770507,0.522284062884356,-9.70984178698023));
#31394=CARTESIAN_POINT('Ctrl Pts',(95.4013986043073,0.515218112832308,-9.70930359446622));
#31395=CARTESIAN_POINT('Ctrl Pts',(95.4000152249072,0.51236468011977,-9.70908737710467));
#31396=CARTESIAN_POINT('Ctrl Pts',(95.3974069812261,0.506928957773521,-9.7086776614679));
#31397=CARTESIAN_POINT('Ctrl Pts',(95.3961799689023,0.504347750459011,-9.70848402831789));
#31398=CARTESIAN_POINT('Ctrl Pts',(95.3932829018368,0.49819567350931,-9.70802465654521));
#31399=CARTESIAN_POINT('Ctrl Pts',(95.391621341949,0.494620806772807,-9.70775942803424));
#31400=CARTESIAN_POINT('Ctrl Pts',(95.385792224421,0.481912840934746,-9.70682238729961));
#31401=CARTESIAN_POINT('Ctrl Pts',(95.381723382299,0.472734565796525,-9.70615618611606));
#31402=CARTESIAN_POINT('Ctrl Pts',(95.3541720295892,0.40837692421404,-9.70155047877698));
#31403=CARTESIAN_POINT('Ctrl Pts',(95.3348135389338,0.351519378942257,-9.69781304091315));
#31404=CARTESIAN_POINT('Ctrl Pts',(95.3032170928488,0.228697882328771,-9.68995593415588));
#31405=CARTESIAN_POINT('Ctrl Pts',(95.2921061103653,0.162671419829283,-9.68585200399263));
#31406=CARTESIAN_POINT('Ctrl Pts',(95.2838558549581,0.0618564476482338,
-9.6794213451601));
#31407=CARTESIAN_POINT('Ctrl Pts',(95.2825533035396,0.0275490047474106,
-9.67720620339286));
#31408=CARTESIAN_POINT('Ctrl Pts',(95.2828054225735,-0.0163490089426878,
-9.67431322973995));
#31409=CARTESIAN_POINT('Ctrl Pts',(95.2829774790101,-0.0259326989281477,
-9.67367812195108));
#31410=CARTESIAN_POINT('Ctrl Pts',(95.2834459430347,-0.0414617368867229,
-9.6726428293934));
#31411=CARTESIAN_POINT('Ctrl Pts',(95.2836704837632,-0.0474089401186523,
-9.67224486872131));
#31412=CARTESIAN_POINT('Ctrl Pts',(95.2841883834959,-0.0588294355572201,
-9.67147771624354));
#31413=CARTESIAN_POINT('Ctrl Pts',(95.2844748954074,-0.0643028951119048,
-9.67110874594469));
#31414=CARTESIAN_POINT('Ctrl Pts',(95.2852189348757,-0.0768398338296617,
-9.67026054729053));
#31415=CARTESIAN_POINT('Ctrl Pts',(95.2857019521605,-0.0839015298191893,
-9.66978054286784));
#31416=CARTESIAN_POINT('Ctrl Pts',(95.2874445843107,-0.106398155289384,
-9.66824400479199));
#31417=CARTESIAN_POINT('Ctrl Pts',(95.288944940145,-0.121812235576373,-9.66718010226665));
#31418=CARTESIAN_POINT('Ctrl Pts',(95.2999177011923,-0.215368901695882,
-9.66065196487231));
#31419=CARTESIAN_POINT('Ctrl Pts',(95.3168991471132,-0.292416437063511,
-9.65495490582798));
#31420=CARTESIAN_POINT('Ctrl Pts',(95.3560870521407,-0.411848393887781,
-9.64573718168791));
#31421=CARTESIAN_POINT('Ctrl Pts',(95.3734046135435,-0.455598816334138,
-9.64227655404078));
#31422=CARTESIAN_POINT('Ctrl Pts',(95.4022832226942,-0.517459655926531,
-9.63734150021458));
#31423=CARTESIAN_POINT('Ctrl Pts',(95.4117955220666,-0.536475449482421,
-9.63581878476946));
#31424=CARTESIAN_POINT('Ctrl Pts',(95.4281338964913,-0.567039786626174,
-9.633372990048));
#31425=CARTESIAN_POINT('Ctrl Pts',(95.434651383726,-0.578747179305988,-9.63243658481255));
#31426=CARTESIAN_POINT('Ctrl Pts',(95.4437480526257,-0.594450866877249,
-9.63118363540933));
#31427=CARTESIAN_POINT('Ctrl Pts',(95.446153424185,-0.598545979893881,-9.63085718962409));
#31428=CARTESIAN_POINT('Ctrl Pts',(95.4502115924571,-0.605360233479817,
-9.63031461401684));
#31429=CARTESIAN_POINT('Ctrl Pts',(95.4518507333845,-0.608087390053742,
-9.63009763767671));
#31430=CARTESIAN_POINT('Ctrl Pts',(95.454978473789,-0.613243793507612,-9.62968775809024));
#31431=CARTESIAN_POINT('Ctrl Pts',(95.4564648645179,-0.615674329880191,
-9.62949471180154));
#31432=CARTESIAN_POINT('Ctrl Pts',(95.4600097988215,-0.621424004043693,
-9.62903835213527));
#31433=CARTESIAN_POINT('Ctrl Pts',(95.4620760778907,-0.624738368892867,
-9.62877553296718));
#31434=CARTESIAN_POINT('Ctrl Pts',(95.4693951447811,-0.636349284878479,
-9.62785546428633));
#31435=CARTESIAN_POINT('Ctrl Pts',(95.4747353395464,-0.644590639520166,
-9.62720356349149));
#31436=CARTESIAN_POINT('Ctrl Pts',(95.518938404173,-0.710973510562911,-9.62195374949609));
#31437=CARTESIAN_POINT('Ctrl Pts',(95.5628117749466,-0.765622922601538,
-9.61763392512529));
#31438=CARTESIAN_POINT('Ctrl Pts',(95.6526389221856,-0.859097719116934,
-9.60961459335801));
#31439=CARTESIAN_POINT('Ctrl Pts',(95.6972050010947,-0.898925358209768,
-9.6059284605526));
#31440=CARTESIAN_POINT('Ctrl Pts',(95.761578133085,-0.948202145616376,-9.60076273497721));
#31441=CARTESIAN_POINT('Ctrl Pts',(95.7789105813841,-0.960736283753483,
-9.59938660352113));
#31442=CARTESIAN_POINT('Ctrl Pts',(95.8096307771272,-0.981702095110454,
-9.59696417698904));
#31443=CARTESIAN_POINT('Ctrl Pts',(95.822865199314,-0.990348962262571,-9.59592573904913));
#31444=CARTESIAN_POINT('Ctrl Pts',(95.8423867953013,-1.00255011061876,-9.59439918537191));
#31445=CARTESIAN_POINT('Ctrl Pts',(95.8485393284822,-1.0063173238857,-9.59391880907546));
#31446=CARTESIAN_POINT('Ctrl Pts',(95.859428753683,-1.01284815812958,-9.59306967845667));
#31447=CARTESIAN_POINT('Ctrl Pts',(95.8641511086371,-1.01563568895872,-9.59270179762273));
#31448=CARTESIAN_POINT('Ctrl Pts',(95.874034436112,-1.02137696677683,-9.59193251505349));
#31449=CARTESIAN_POINT('Ctrl Pts',(95.8791986449019,-1.02432480271343,-9.59153091580406));
#31450=CARTESIAN_POINT('Ctrl Pts',(95.892722240761,-1.03190914605693,-9.59048005983638));
#31451=CARTESIAN_POINT('Ctrl Pts',(95.901116002572,-1.03648313246012,-9.58982862435961));
#31452=CARTESIAN_POINT('Ctrl Pts',(95.9366764927274,-1.05530323395806,-9.58707149231913));
#31453=CARTESIAN_POINT('Ctrl Pts',(95.9643365492331,-1.06858619715539,-9.58493303263459));
#31454=CARTESIAN_POINT('Ctrl Pts',(96.0689309243904,-1.11387794247038,-9.57686364034604));
#31455=CARTESIAN_POINT('Ctrl Pts',(96.1486695586333,-1.13877379048116,-9.57072363283565));
#31456=CARTESIAN_POINT('Ctrl Pts',(96.2815894238688,-1.16525631087155,-9.56080220974697));
#31457=CARTESIAN_POINT('Ctrl Pts',(96.33345483736,-1.17204527172996,-9.55701168976383));
#31458=CARTESIAN_POINT('Ctrl Pts',(96.3925511677265,-1.17580995510247,-9.55289304259375));
#31459=CARTESIAN_POINT('Ctrl Pts',(96.3995012063141,-1.17619087844943,-9.55241183030035));
#31460=CARTESIAN_POINT('Ctrl Pts',(96.4101128557629,-1.17667817605298,-9.55168232025463));
#31461=CARTESIAN_POINT('Ctrl Pts',(96.4137721177493,-1.17682911283672,-9.55143170803378));
#31462=CARTESIAN_POINT('Ctrl Pts',(96.4204725206237,-1.17707418828228,-9.55097462377396));
#31463=CARTESIAN_POINT('Ctrl Pts',(96.4235133340026,-1.17717361291988,-9.55076787555905));
#31464=CARTESIAN_POINT('Ctrl Pts',(96.4303792334441,-1.17737147453957,-9.55030259045109));
#31465=CARTESIAN_POINT('Ctrl Pts',(96.4342044362904,-1.17746305600493,-9.55004443172208));
#31466=CARTESIAN_POINT('Ctrl Pts',(96.4440927691344,-1.17765158665202,-9.54937967669437));
#31467=CARTESIAN_POINT('Ctrl Pts',(96.4501564133056,-1.17772035720364,-9.54897456460657));
#31468=CARTESIAN_POINT('Ctrl Pts',(96.4908761042343,-1.1778676604155,-9.54626940342467));
#31469=CARTESIAN_POINT('Ctrl Pts',(96.5255241434315,-1.17646333535691,-9.54404194948902));
#31470=CARTESIAN_POINT('Ctrl Pts',(96.5881484456094,-1.17114923716987,-9.54007068966371));
#31471=CARTESIAN_POINT('Ctrl Pts',(96.6161402226448,-1.16775846669995,-9.53831561173425));
#31472=CARTESIAN_POINT('Ctrl Pts',(96.6913337700111,-1.15589782805985,-9.53359578930069));
#31473=CARTESIAN_POINT('Ctrl Pts',(96.7381822487611,-1.14554559493261,-9.53064800233047));
#31474=CARTESIAN_POINT('Ctrl Pts',(96.8355895263926,-1.11769304590989,-9.52431269752399));
#31475=CARTESIAN_POINT('Ctrl Pts',(96.8858468571973,-1.09954851988977,-9.52091967414613));
#31476=CARTESIAN_POINT('Ctrl Pts',(96.9446142311109,-1.07369801028633,-9.51670010441911));
#31477=CARTESIAN_POINT('Ctrl Pts',(96.9544708171645,-1.06919897564376,-9.51598366696585));
#31478=CARTESIAN_POINT('Ctrl Pts',(96.9698892185514,-1.06190254354049,-9.51484845148636));
#31479=CARTESIAN_POINT('Ctrl Pts',(96.9754934853382,-1.05919586572956,-9.51443276475589));
#31480=CARTESIAN_POINT('Ctrl Pts',(96.9859455307391,-1.05404530620512,-9.51365162066659));
#31481=CARTESIAN_POINT('Ctrl Pts',(96.9907983938131,-1.05161206736982,-9.51328653749921));
#31482=CARTESIAN_POINT('Ctrl Pts',(97.0016252260918,-1.04608946353732,-9.51246654799852));
#31483=CARTESIAN_POINT('Ctrl Pts',(97.0075898638776,-1.04298232313767,-9.51201103382089));
#31484=CARTESIAN_POINT('Ctrl Pts',(97.0226995506075,-1.03494600459869,-9.51084731390792));
#31485=CARTESIAN_POINT('Ctrl Pts',(97.0318064318337,-1.02994668265892,-9.51013667776087));
#31486=CARTESIAN_POINT('Ctrl Pts',(97.1065147089747,-0.987639029854072,
-9.50422858454984));
#31487=CARTESIAN_POINT('Ctrl Pts',(97.1684449873345,-0.944231704060049,
-9.49880945708824));
#31488=CARTESIAN_POINT('Ctrl Pts',(97.2697365825046,-0.857638245867293,
-9.48906112779236));
#31489=CARTESIAN_POINT('Ctrl Pts',(97.3108586993011,-0.81688186071571,-9.48479076685285));
#31490=CARTESIAN_POINT('Ctrl Pts',(97.3622755606574,-0.757813587199519,
-9.47913573117237));
#31491=CARTESIAN_POINT('Ctrl Pts',(97.3753245597906,-0.742008235792204,
-9.47766940251814));
#31492=CARTESIAN_POINT('Ctrl Pts',(97.3959976894294,-0.715593302520383,
-9.47530379049061));
#31493=CARTESIAN_POINT('Ctrl Pts',(97.4038692637876,-0.705183571225206,
-9.4743921769645));
#31494=CARTESIAN_POINT('Ctrl Pts',(97.4143398134915,-0.690847623066946,
-9.47316677951444));
#31495=CARTESIAN_POINT('Ctrl Pts',(97.4170903339025,-0.687033957145837,
-9.47284363073537));
#31496=CARTESIAN_POINT('Ctrl Pts',(97.4216581523541,-0.680619945372944,
-9.47230500493844));
#31497=CARTESIAN_POINT('Ctrl Pts',(97.4234878936372,-0.678028577309876,
-9.47208870690451));
#31498=CARTESIAN_POINT('Ctrl Pts',(97.4269458266491,-0.673089049200456,
-9.47167895283645));
#31499=CARTESIAN_POINT('Ctrl Pts',(97.4285759733574,-0.670742314262643,
-9.4714853611806));
#31500=CARTESIAN_POINT('Ctrl Pts',(97.4324329809438,-0.66514646985121,-9.47102623864534));
#31501=CARTESIAN_POINT('Ctrl Pts',(97.4346521321528,-0.661892049942476,
-9.47076121641535));
#31502=CARTESIAN_POINT('Ctrl Pts',(97.442457819903,-0.650320589331951,-9.46982570428204));
#31503=CARTESIAN_POINT('Ctrl Pts',(97.4479547003819,-0.641943183283677,
-9.46916080076482));
#31504=CARTESIAN_POINT('Ctrl Pts',(97.4871209619809,-0.580558859525506,
-9.46437011267051));
#31505=CARTESIAN_POINT('Ctrl Pts',(97.5166144735962,-0.524997485779002,
-9.46046650915653));
#31506=CARTESIAN_POINT('Ctrl Pts',(97.5672262681078,-0.407922157811988,
-9.45256963243796));
#31507=CARTESIAN_POINT('Ctrl Pts',(97.5879695640729,-0.346488785834593,
-9.44858816834218));
#31508=CARTESIAN_POINT('Ctrl Pts',(97.6089473610301,-0.261954743813344,
-9.44304743214294));
#31509=CARTESIAN_POINT('Ctrl Pts',(97.6137149089239,-0.240097331154344,
-9.44161021404495));
#31510=CARTESIAN_POINT('Ctrl Pts',(97.6208867666266,-0.202042142555787,
-9.4390902408425));
#31511=CARTESIAN_POINT('Ctrl Pts',(97.6235810768083,-0.185905188569885,
-9.43801626633463));
#31512=CARTESIAN_POINT('Ctrl Pts',(97.6269920582106,-0.162481897634714,
-9.43644712753011));
#31513=CARTESIAN_POINT('Ctrl Pts',(97.6279783664016,-0.155236307944396,
-9.43596033906931));
#31514=CARTESIAN_POINT('Ctrl Pts',(97.6295879339619,-0.14252771489406,-9.43510385717476));
#31515=CARTESIAN_POINT('Ctrl Pts',(97.6302405347156,-0.137068602094876,
-9.43473508707107));
#31516=CARTESIAN_POINT('Ctrl Pts',(97.6315146219413,-0.125738058193731,
-9.43396782133301));
#31517=CARTESIAN_POINT('Ctrl Pts',(97.6321302267512,-0.119866134497164,
-9.43356915395697));
#31518=CARTESIAN_POINT('Ctrl Pts',(97.6336081332065,-0.104668014213329,
-9.43253448221552));
#31519=CARTESIAN_POINT('Ctrl Pts',(97.6344033685614,-0.095335867280265,
-9.43189642183917));
#31520=CARTESIAN_POINT('Ctrl Pts',(97.6372002648836,-0.0571332458221609,
-9.42927262217701));
#31521=CARTESIAN_POINT('Ctrl Pts',(97.6382486527104,-0.0282053345403859,
-9.42725795700893));
#31522=CARTESIAN_POINT('Ctrl Pts',(97.6381988360772,0.0521916868471752,
-9.42157768963717));
#31523=CARTESIAN_POINT('Ctrl Pts',(97.6347940729209,0.103590782919541,-9.41785139203066));
#31524=CARTESIAN_POINT('Ctrl Pts',(97.617189254572,0.236546808710548,-9.40803746655624));
#31525=CARTESIAN_POINT('Ctrl Pts',(97.597740096058,0.317130997477428,-9.40190418519218));
#31526=CARTESIAN_POINT('Ctrl Pts',(97.566910878893,0.403724255026715,-9.39547326972626));
#31527=CARTESIAN_POINT('Ctrl Pts',(97.5637088862815,0.412393738420563,-9.39483150476054));
#31528=CARTESIAN_POINT('Ctrl Pts',(97.5589536710704,0.424816697425107,-9.39391577835899));
#31529=CARTESIAN_POINT('Ctrl Pts',(97.5574826602829,0.428600973186868,-9.39363735470494));
#31530=CARTESIAN_POINT('Ctrl Pts',(97.5548646214973,0.435234273324378,-9.39315033390435));
#31531=CARTESIAN_POINT('Ctrl Pts',(97.5537259769176,0.438086526974744,-9.39294125456747));
#31532=CARTESIAN_POINT('Ctrl Pts',(97.5512820076479,0.444139688565794,-9.39249827890143));
#31533=CARTESIAN_POINT('Ctrl Pts',(97.5499737392852,0.447339326680638,-9.39226455858095));
#31534=CARTESIAN_POINT('Ctrl Pts',(97.5463552794594,0.456078973178444,-9.39162722522645));
#31535=CARTESIAN_POINT('Ctrl Pts',(97.5440167554704,0.46160724777128,-9.39122525102946));
#31536=CARTESIAN_POINT('Ctrl Pts',(97.5310437962972,0.491633481092809,-9.38904709874659));
#31537=CARTESIAN_POINT('Ctrl Pts',(97.5196198101522,0.515784273382338,-9.38731380062034));
#31538=CARTESIAN_POINT('Ctrl Pts',(97.4779256047128,0.596687933488769,-9.38150232586648));
#31539=CARTESIAN_POINT('Ctrl Pts',(97.4438337871889,0.65134362304228,-9.37756291412851));
#31540=CARTESIAN_POINT('Ctrl Pts',(97.3618095508863,0.761608451092322,-9.36904914138031));
#31541=CARTESIAN_POINT('Ctrl Pts',(97.3128099496039,0.816072218763233,-9.36447494702547));
#31542=CARTESIAN_POINT('Ctrl Pts',(97.251406931976,0.872720003483838,-9.35899267628131));
#31543=CARTESIAN_POINT('Ctrl Pts',(97.2436379240827,0.879698389241347,-9.35830337965559));
#31544=CARTESIAN_POINT('Ctrl Pts',(97.2307022953402,0.891010434065669,-9.35716207731774));
#31545=CARTESIAN_POINT('Ctrl Pts',(97.2255893216783,0.895404763697256,-9.35671256590973));
#31546=CARTESIAN_POINT('Ctrl Pts',(97.216290696226,0.903258641847561,-9.35589777458998));
#31547=CARTESIAN_POINT('Ctrl Pts',(97.212118281935,0.906733624677735,-9.35553313236064));
#31548=CARTESIAN_POINT('Ctrl Pts',(97.2031213655216,0.914121908489025,-9.35474882671488));
#31549=CARTESIAN_POINT('Ctrl Pts',(97.198289651343,0.918026126001126,-9.35432881613633));
#31550=CARTESIAN_POINT('Ctrl Pts',(97.1849889965757,0.928600757789876,-9.35317571529104));
#31551=CARTESIAN_POINT('Ctrl Pts',(97.1764591749049,0.935193266119392,-9.35243960515133));
#31552=CARTESIAN_POINT('Ctrl Pts',(97.1260842532683,0.973033766220799,-9.34811064298131));
#31553=CARTESIAN_POINT('Ctrl Pts',(97.0822942394661,1.0015834035715,-9.34441645064773));
#31554=CARTESIAN_POINT('Ctrl Pts',(96.9701811969145,1.06448524508665,-9.33513283559314));
#31555=CARTESIAN_POINT('Ctrl Pts',(96.9001331014893,1.09527535787211,-9.32947001769076));
#31556=CARTESIAN_POINT('Ctrl Pts',(96.8117530641047,1.12426916652382,-9.32272075086632));
#31557=CARTESIAN_POINT('Ctrl Pts',(96.7957956035911,1.12913125212418,-9.32151783558619));
#31558=CARTESIAN_POINT('Ctrl Pts',(96.7597762500007,1.13927500221777,-9.31884466599141));
#31559=CARTESIAN_POINT('Ctrl Pts',(96.7396663000653,1.14436920415061,-9.31738100904247));
#31560=CARTESIAN_POINT('Ctrl Pts',(96.7137941241155,1.15020036733815,-9.31554308650517));
#31561=CARTESIAN_POINT('Ctrl Pts',(96.7081479578379,1.15142933168303,-9.31514471604512));
#31562=CARTESIAN_POINT('Ctrl Pts',(96.6991581583803,1.15331689608347,-9.31451499968291));
#31563=CARTESIAN_POINT('Ctrl Pts',(96.6958204075905,1.154002605301,-9.31428219479942));
#31564=CARTESIAN_POINT('Ctrl Pts',(96.6894543824504,1.15528167621914,-9.31384013008019));
#31565=CARTESIAN_POINT('Ctrl Pts',(96.6864267743582,1.15587761845616,-9.31363073920797));
#31566=CARTESIAN_POINT('Ctrl Pts',(96.6792415155632,1.15726262571735,-9.31313575933227));
#31567=CARTESIAN_POINT('Ctrl Pts',(96.6750819006015,1.15804119240724,-9.31285075672145));
#31568=CARTESIAN_POINT('Ctrl Pts',(96.6611036303633,1.16057964089917,-9.31189792231971));
#31569=CARTESIAN_POINT('Ctrl Pts',(96.6512665132075,1.16223725969956,-9.31123548693794));
#31570=CARTESIAN_POINT('Ctrl Pts',(96.6273321931131,1.16595826453804,-9.30964079295392));
#31571=CARTESIAN_POINT('Ctrl Pts',(96.6132160358401,1.16789128088837,-9.30871455268559));
#31572=CARTESIAN_POINT('Ctrl Pts',(96.5567626493365,1.17458066438581,-9.30505483216197));
#31573=CARTESIAN_POINT('Ctrl Pts',(96.514213441249,1.17729489988081,-9.30239524977197));
#31574=CARTESIAN_POINT('Ctrl Pts',(96.3750715147137,1.1786095131862,-9.29376481014584));
#31575=CARTESIAN_POINT('Ctrl Pts',(96.2788007321574,1.16764951072788,-9.28786478668805));
#31576=CARTESIAN_POINT('Ctrl Pts',(96.1709999593411,1.14170998014678,-9.28062537908701));
#31577=CARTESIAN_POINT('Ctrl Pts',(96.1571133216392,1.13809884269981,-9.2796811969285));
#31578=CARTESIAN_POINT('Ctrl Pts',(96.1366106696226,1.13236535692382,-9.27826822661105));
#31579=CARTESIAN_POINT('Ctrl Pts',(96.1299415331896,1.13043661943327,-9.27780561166113));
#31580=CARTESIAN_POINT('Ctrl Pts',(96.1180693220419,1.12688909319762,-9.27697652457454));
#31581=CARTESIAN_POINT('Ctrl Pts',(96.1128596526335,1.12529293219493,-9.27661078991669));
#31582=CARTESIAN_POINT('Ctrl Pts',(96.1018572937299,1.12183828775926,-9.27583422535463));
#31583=CARTESIAN_POINT('Ctrl Pts',(96.0960675702115,1.11997096255215,-9.27542311823925));
#31584=CARTESIAN_POINT('Ctrl Pts',(96.080620552989,1.11485646919493,-9.27431955173233));
#31585=CARTESIAN_POINT('Ctrl Pts',(96.0709906764101,1.11152875968215,-9.27362449371967));
#31586=CARTESIAN_POINT('Ctrl Pts',(96.0218915104046,1.09384561913521,-9.27004328299704));
#31587=CARTESIAN_POINT('Ctrl Pts',(95.9831717603254,1.07751293683962,-9.26709298075929));
#31588=CARTESIAN_POINT('Ctrl Pts',(95.9374941354851,1.05529964700024,-9.26345652482644));
#31589=CARTESIAN_POINT('Ctrl Pts',(95.9296240398814,1.05136263071937,-9.26282423601162));
#31590=CARTESIAN_POINT('Ctrl Pts',(95.9218016185417,1.04733931503376,-9.26219012624909));
#31591=CARTESIAN_POINT('',(97.6382309056894,0.000321523407826734,-9.32563288532119));
#31592=CARTESIAN_POINT('Ctrl Pts',(95.9218016730733,1.04733934308103,-9.1639126954948));
#31593=CARTESIAN_POINT('Ctrl Pts',(95.922814848987,1.04786045104073,-9.16399103829153));
#31594=CARTESIAN_POINT('Ctrl Pts',(95.9238287879189,1.04838009233506,-9.16406929595243));
#31595=CARTESIAN_POINT('Ctrl Pts',(95.9279792234048,1.05049958171471,-9.16438904021808));
#31596=CARTESIAN_POINT('Ctrl Pts',(95.9311221772002,1.05208685501054,-9.16462978372474));
#31597=CARTESIAN_POINT('Ctrl Pts',(95.936732942886,1.05488892929961,-9.16505703168365));
#31598=CARTESIAN_POINT('Ctrl Pts',(95.939197888489,1.05610917908104,-9.16524386338441));
#31599=CARTESIAN_POINT('Ctrl Pts',(95.9451213194579,1.0590157307738,-9.16569077717861));
#31600=CARTESIAN_POINT('Ctrl Pts',(95.9485838179442,1.06069373245005,-9.16595035026591));
#31601=CARTESIAN_POINT('Ctrl Pts',(95.9591582030892,1.06575446814968,-9.16673820088793));
#31602=CARTESIAN_POINT('Ctrl Pts',(95.9662960244338,1.06908294838597,-9.16726331563224));
#31603=CARTESIAN_POINT('Ctrl Pts',(95.9829965585636,1.07666766646834,-9.16847765797699));
#31604=CARTESIAN_POINT('Ctrl Pts',(95.9925838192388,1.08086858579362,-9.16916399532946));
#31605=CARTESIAN_POINT('Ctrl Pts',(96.0263765587037,1.09514187831299,-9.17154994191645));
#31606=CARTESIAN_POINT('Ctrl Pts',(96.0508624790331,1.10453395101049,-9.17321972048688));
#31607=CARTESIAN_POINT('Ctrl Pts',(96.1492301884765,1.13854309227748,-9.17977139358815));
#31608=CARTESIAN_POINT('Ctrl Pts',(96.2251598181554,1.15662533032439,-9.18449776961288));
#31609=CARTESIAN_POINT('Ctrl Pts',(96.3495170094827,1.17347794025397,-9.19237453603823));
#31610=CARTESIAN_POINT('Ctrl Pts',(96.3970527609507,1.17700447016527,-9.19541367264068));
#31611=CARTESIAN_POINT('Ctrl Pts',(96.4554530408275,1.17778865940993,-9.19925166261787));
#31612=CARTESIAN_POINT('Ctrl Pts',(96.4662395141318,1.17778530829299,-9.19996476278667));
#31613=CARTESIAN_POINT('Ctrl Pts',(96.4832990891366,1.17754565848997,-9.20109995777827));
#31614=CARTESIAN_POINT('Ctrl Pts',(96.4895731338883,1.1774073583786,-9.2015190287545));
#31615=CARTESIAN_POINT('Ctrl Pts',(96.5012670021924,1.17705606397813,-9.20230318961481));
#31616=CARTESIAN_POINT('Ctrl Pts',(96.5066870626377,1.17685575720505,-9.20266787769109));
#31617=CARTESIAN_POINT('Ctrl Pts',(96.5187542795268,1.17632630391864,-9.2034826555472));
#31618=CARTESIAN_POINT('Ctrl Pts',(96.5254003765902,1.17597823922385,-9.20393331850885));
#31619=CARTESIAN_POINT('Ctrl Pts',(96.5449123104133,1.17479046615917,-9.2052622224221));
#31620=CARTESIAN_POINT('Ctrl Pts',(96.5577673745231,1.17379581814988,-9.20614520439128));
#31621=CARTESIAN_POINT('Ctrl Pts',(96.5869802357034,1.17105233426194,-9.20816949999865));
#31622=CARTESIAN_POINT('Ctrl Pts',(96.6033226237227,1.16917143692625,-9.20931466270758));
#31623=CARTESIAN_POINT('Ctrl Pts',(96.6582174266742,1.1616853477804,-9.21320510040282));
#31624=CARTESIAN_POINT('Ctrl Pts',(96.696526756446,1.15451046970759,-9.21599425470878));
#31625=CARTESIAN_POINT('Ctrl Pts',(96.778019076342,1.13502219176143,-9.22207222122691));
#31626=CARTESIAN_POINT('Ctrl Pts',(96.8209983638215,1.12211084362784,-9.22536839884872));
#31627=CARTESIAN_POINT('Ctrl Pts',(96.9193232450497,1.08633963104154,-9.23304227804842));
#31628=CARTESIAN_POINT('Ctrl Pts',(96.9738802387444,1.06164631933635,-9.23740504343882));
#31629=CARTESIAN_POINT('Ctrl Pts',(97.0319255438538,1.02984796581947,-9.24200988958387));
#31630=CARTESIAN_POINT('Ctrl Pts',(97.0374954285506,1.02673757726301,-9.24245131555883));
#31631=CARTESIAN_POINT('Ctrl Pts',(97.0464471546272,1.02164281368668,-9.24315971210766));
#31632=CARTESIAN_POINT('Ctrl Pts',(97.0498447510446,1.01968659050402,-9.24342833520348));
#31633=CARTESIAN_POINT('Ctrl Pts',(97.055817845369,1.01620765294511,-9.24390006398209));
#31634=CARTESIAN_POINT('Ctrl Pts',(97.0583973770067,1.01469205176521,-9.24410360732617));
#31635=CARTESIAN_POINT('Ctrl Pts',(97.0639634191068,1.0113931332502,-9.24454241270291));
#31636=CARTESIAN_POINT('Ctrl Pts',(97.0669478183563,1.00960640790023,-9.2447774539566));
#31637=CARTESIAN_POINT('Ctrl Pts',(97.0731460440199,1.00585820066837,-9.24526520495842));
#31638=CARTESIAN_POINT('Ctrl Pts',(97.0763584744495,1.00389447309009,-9.24551777177673));
#31639=CARTESIAN_POINT('Ctrl Pts',(97.084565964538,0.998823089156785,-9.24616262672578));
#31640=CARTESIAN_POINT('Ctrl Pts',(97.0895473255119,0.995693309879872,-9.24655359487434));
#31641=CARTESIAN_POINT('Ctrl Pts',(97.1040763463914,0.986412194474156,-9.24769335394931));
#31642=CARTESIAN_POINT('Ctrl Pts',(97.1135589961314,0.980159751339093,-9.24843651446852));
#31643=CARTESIAN_POINT('Ctrl Pts',(97.1474892275136,0.957076568149981,-9.25109870094033));
#31644=CARTESIAN_POINT('Ctrl Pts',(97.1713903370831,0.939459431143961,-9.25297995838663));
#31645=CARTESIAN_POINT('Ctrl Pts',(97.2731280256641,0.858361431341868,-9.26113372196366));
#31646=CARTESIAN_POINT('Ctrl Pts',(97.3433228603323,0.785983443176158,-9.26719052002289));
#31647=CARTESIAN_POINT('Ctrl Pts',(97.4179664287171,0.686222210637065,-9.27520244793632));
#31648=CARTESIAN_POINT('Ctrl Pts',(97.4318476498015,0.666427767296901,-9.27677565144272));
#31649=CARTESIAN_POINT('Ctrl Pts',(97.4499181195329,0.63889432496033,-9.27895024457551));
#31650=CARTESIAN_POINT('Ctrl Pts',(97.4546448548664,0.631514049183242,-9.27953182557908));
#31651=CARTESIAN_POINT('Ctrl Pts',(97.4620427518038,0.619674133616652,-9.28046310977286));
#31652=CARTESIAN_POINT('Ctrl Pts',(97.4647675785383,0.615248275882033,-9.28081085240701));
#31653=CARTESIAN_POINT('Ctrl Pts',(97.4703110390121,0.606109239880254,-9.28152821811447));
#31654=CARTESIAN_POINT('Ctrl Pts',(97.4731261761087,0.601394100092953,-9.28189795603467));
#31655=CARTESIAN_POINT('Ctrl Pts',(97.4795923950988,0.59038954088573,-9.28276010586785));
#31656=CARTESIAN_POINT('Ctrl Pts',(97.4832183708644,0.584085705503281,-9.28325339813373));
#31657=CARTESIAN_POINT('Ctrl Pts',(97.4947006076781,0.563688824558587,-9.28484790831653));
#31658=CARTESIAN_POINT('Ctrl Pts',(97.5023254307736,0.549468310679476,-9.2859571791848));
#31659=CARTESIAN_POINT('Ctrl Pts',(97.5196359476891,0.515527215968371,-9.28860043245823));
#31660=CARTESIAN_POINT('Ctrl Pts',(97.5290664365317,0.495683942702836,-9.29014248266009));
#31661=CARTESIAN_POINT('Ctrl Pts',(97.5430286305111,0.46405239273454,-9.29259559516936));
#31662=CARTESIAN_POINT('Ctrl Pts',(97.5479353973612,0.452434427257455,-9.29349553308035));
#31663=CARTESIAN_POINT('Ctrl Pts',(97.5916981364443,0.343988444268873,-9.30188403299866));
#31664=CARTESIAN_POINT('Ctrl Pts',(97.6177087725841,0.242489700997993,-9.30970477735835));
#31665=CARTESIAN_POINT('Ctrl Pts',(97.6322371076608,0.12016086300608,-9.3184813902564));
#31666=CARTESIAN_POINT('Ctrl Pts',(97.6340120284564,0.101370767593353,-9.31981018525258));
#31667=CARTESIAN_POINT('Ctrl Pts',(97.6357258832803,0.0769776311818763,
-9.32150367281578));
#31668=CARTESIAN_POINT('Ctrl Pts',(97.6360774700598,0.0714075207628335,
-9.321888248877));
#31669=CARTESIAN_POINT('Ctrl Pts',(97.6365774784201,0.0624766447800458,
-9.32250123347332));
#31670=CARTESIAN_POINT('Ctrl Pts',(97.6367511153154,0.0591174611465136,
-9.32273097436978));
#31671=CARTESIAN_POINT('Ctrl Pts',(97.6370484999609,0.0528429352808183,
-9.32315850962415));
#31672=CARTESIAN_POINT('Ctrl Pts',(97.6371758069143,0.0499278411504255,
-9.32335649199225));
#31673=CARTESIAN_POINT('Ctrl Pts',(97.6374145460375,0.0439517227946099,
-9.32376108715971));
#31674=CARTESIAN_POINT('Ctrl Pts',(97.6375248733501,0.0408906645931219,
-9.32396764019607));
#31675=CARTESIAN_POINT('Ctrl Pts',(97.6378027476884,0.0322439599734504,
-9.32454924827992));
#31676=CARTESIAN_POINT('Ctrl Pts',(97.6379424881039,0.0266574109352865,
-9.32492283818597));
#31677=CARTESIAN_POINT('Ctrl Pts',(97.6381657953044,0.0141771713317196,
-9.32575298202203));
#31678=CARTESIAN_POINT('Ctrl Pts',(97.6382286077225,0.00728328496665232,
-9.32620850998168));
#31679=CARTESIAN_POINT('Ctrl Pts',(97.6382308853076,0.000389084372464196,
-9.32666138302753));
#31680=CARTESIAN_POINT('Ctrl Pts',(97.6382309056894,0.000321523407826734,
-9.3256328853212));
#31681=CARTESIAN_POINT('Ctrl Pts',(97.6382435761352,-0.0460907022632928,
-9.32878688556136));
#31682=CARTESIAN_POINT('Ctrl Pts',(97.6355084800378,-0.0926118624646665,
-9.33194088580153));
#31683=CARTESIAN_POINT('Ctrl Pts',(97.630013099911,-0.138887047038513,-9.3350948860417));
#31684=CARTESIAN_POINT('Ctrl Pts',(97.6245255048694,-0.185096675409236,
-9.33824441813588));
#31685=CARTESIAN_POINT('Ctrl Pts',(97.6162854232476,-0.231060459664611,
-9.34139395023005));
#31686=CARTESIAN_POINT('Ctrl Pts',(97.6053323074263,-0.276424367469098,
-9.34454348232423));
#31687=CARTESIAN_POINT('Ctrl Pts',(97.5943897069927,-0.321744724279503,
-9.34768999075355));
#31688=CARTESIAN_POINT('Ctrl Pts',(97.580739357164,-0.366465795608954,-9.35083649918288));
#31689=CARTESIAN_POINT('Ctrl Pts',(97.5644720036866,-0.410242385603896,
-9.3539830076122));
#31690=CARTESIAN_POINT('Ctrl Pts',(97.5482128406558,-0.453996934531981,
-9.35712793180661));
#31691=CARTESIAN_POINT('Ctrl Pts',(97.5293394803747,-0.496807413645105,
-9.36027285600101));
#31692=CARTESIAN_POINT('Ctrl Pts',(97.5079920405549,-0.538345220818771,
-9.36341778019541));
#31693=CARTESIAN_POINT('Ctrl Pts',(97.4866293822363,-0.579912640117923,
-9.36656494639285));
#31694=CARTESIAN_POINT('Ctrl Pts',(97.4627893710122,-0.620205065273235,
-9.36971211259029));
#31695=CARTESIAN_POINT('Ctrl Pts',(97.4366588202512,-0.658917162704153,
-9.37285927878773));
#31696=CARTESIAN_POINT('Ctrl Pts',(97.4105207063682,-0.697640464809353,
-9.37600735588834));
#31697=CARTESIAN_POINT('Ctrl Pts',(97.3820910706567,-0.734782072069771,
-9.37915543298895));
#31698=CARTESIAN_POINT('Ctrl Pts',(97.3515987835877,-0.770067573923226,
-9.38230351008955));
#31699=CARTESIAN_POINT('Ctrl Pts',(97.3210452391043,-0.805423962509669,
-9.38545791151287));
#31700=CARTESIAN_POINT('Ctrl Pts',(97.2884211566196,-0.838916383833414,
-9.38861231293619));
#31701=CARTESIAN_POINT('Ctrl Pts',(97.2539931952205,-0.870306485391062,
-9.39176671435952));
#31702=CARTESIAN_POINT('Ctrl Pts',(97.2204727647251,-0.900869134898895,
-9.39483796485964));
#31703=CARTESIAN_POINT('Ctrl Pts',(97.1852428631882,-0.929438738903102,
-9.39790921535977));
#31704=CARTESIAN_POINT('Ctrl Pts',(97.1485766766973,-0.955834364740461,
-9.4009804658599));
#31705=CARTESIAN_POINT('Ctrl Pts',(97.1092791289799,-0.984124281558804,
-9.40427212568688));
#31706=CARTESIAN_POINT('Ctrl Pts',(97.0681436983917,-1.0100517204561,-9.40756378551386));
#31707=CARTESIAN_POINT('Ctrl Pts',(97.0254881052638,-1.03337407385842,-9.41085544534085));
#31708=CARTESIAN_POINT('Ctrl Pts',(96.9843815618015,-1.05584946954454,-9.41402756763054));
#31709=CARTESIAN_POINT('Ctrl Pts',(96.9418639163497,-1.07590545553094,-9.41719968992023));
#31710=CARTESIAN_POINT('Ctrl Pts',(96.8982506177933,-1.09336763263313,-9.42037181220992));
#31711=CARTESIAN_POINT('Ctrl Pts',(96.8546806647558,-1.11081245477359,-9.42354078185372));
#31712=CARTESIAN_POINT('Ctrl Pts',(96.8100177291949,-1.12566836392258,-9.42670975149752));
#31713=CARTESIAN_POINT('Ctrl Pts',(96.7645997277354,-1.13780790613858,-9.42987872114132));
#31714=CARTESIAN_POINT('Ctrl Pts',(96.719206867905,-1.14994072837884,-9.43304593656748));
#31715=CARTESIAN_POINT('Ctrl Pts',(96.6730603079208,-1.15936001857546,-9.43621315199364));
#31716=CARTESIAN_POINT('Ctrl Pts',(96.626513111044,-1.16598815768369,-9.4393803674198));
#31717=CARTESIAN_POINT('Ctrl Pts',(96.5799711876462,-1.17261554586911,-9.44254722402212));
#31718=CARTESIAN_POINT('Ctrl Pts',(96.5330292694809,-1.17645233430959,-9.44571408062444));
#31719=CARTESIAN_POINT('Ctrl Pts',(96.4860478852236,-1.17747246010327,-9.44888093722676));
#31720=CARTESIAN_POINT('Ctrl Pts',(96.4390189437089,-1.17849361852691,-9.45205099950334));
#31721=CARTESIAN_POINT('Ctrl Pts',(96.3919510147601,-1.17669241495227,-9.45522106177993));
#31722=CARTESIAN_POINT('Ctrl Pts',(96.3452049779548,-1.17209492485317,-9.45839112405651));
#31723=CARTESIAN_POINT('Ctrl Pts',(96.2984304480075,-1.16749463244296,-9.4615631185832));
#31724=CARTESIAN_POINT('Ctrl Pts',(96.2519787513863,-1.1600947496835,-9.46473511310989));
#31725=CARTESIAN_POINT('Ctrl Pts',(96.2062023526948,-1.14997280736007,-9.46790710763658));
#31726=CARTESIAN_POINT('Ctrl Pts',(96.1603436706197,-1.13983267077747,-9.47108480384469));
#31727=CARTESIAN_POINT('Ctrl Pts',(96.1151632425546,-1.12696087008998,-9.47426250005281));
#31728=CARTESIAN_POINT('Ctrl Pts',(96.0709982369142,-1.11148471831006,-9.47744019626092));
#31729=CARTESIAN_POINT('Ctrl Pts',(96.0592304063825,-1.10736107496876,-9.47828689807644));
#31730=CARTESIAN_POINT('Ctrl Pts',(96.0475345487335,-1.10305279343504,-9.47913359989196));
#31731=CARTESIAN_POINT('Ctrl Pts',(96.0359167648909,-1.09856284097989,-9.47998030170748));
#31732=CARTESIAN_POINT('Ctrl Pts',(95.9907511686297,-1.0811075859529,-9.48327196153446));
#31733=CARTESIAN_POINT('Ctrl Pts',(95.946560001052,-1.06082220612803,-9.48656362136144));
#31734=CARTESIAN_POINT('Ctrl Pts',(95.9037200530682,-1.03784024137568,-9.48985528118843));
#31735=CARTESIAN_POINT('Ctrl Pts',(95.8624358103002,-1.0156928519232,-9.49302740650142));
#31736=CARTESIAN_POINT('Ctrl Pts',(95.8224068712118,-0.991041666390307,
-9.49619953181442));
#31737=CARTESIAN_POINT('Ctrl Pts',(95.7839516601953,-0.964055591295815,
-9.49937165712742));
#31738=CARTESIAN_POINT('Ctrl Pts',(95.7455346679984,-0.937096336387842,
-9.50254062981476));
#31739=CARTESIAN_POINT('Ctrl Pts',(95.7086887626404,-0.907807103671446,
-9.5057096025021));
#31740=CARTESIAN_POINT('Ctrl Pts',(95.6737053268424,-0.876401267668292,
-9.50887857518945));
#31741=CARTESIAN_POINT('Ctrl Pts',(95.638741256333,-0.845012816552093,-9.51204579367315));
#31742=CARTESIAN_POINT('Ctrl Pts',(95.6056380273375,-0.811510454951653,
-9.51521301215685));
#31743=CARTESIAN_POINT('Ctrl Pts',(95.5746535605387,-0.776147472668386,
-9.51838023064056));
#31744=CARTESIAN_POINT('Ctrl Pts',(95.5436726039884,-0.740788496678367,
-9.5215470903082));
#31745=CARTESIAN_POINT('Ctrl Pts',(95.5148102987333,-0.703569739044834,
-9.52471394997584));
#31746=CARTESIAN_POINT('Ctrl Pts',(95.4882854648538,-0.664778912108246,
-9.52788080964348));
#31747=CARTESIAN_POINT('Ctrl Pts',(95.4617337811362,-0.625948819047436,
-9.53105087497377));
#31748=CARTESIAN_POINT('Ctrl Pts',(95.4375246036784,-0.585543943478989,
-9.53422094030406));
#31749=CARTESIAN_POINT('Ctrl Pts',(95.415833276992,-0.543880779824758,-9.53739100563435));
#31750=CARTESIAN_POINT('Ctrl Pts',(95.394128728814,-0.502192221266026,-9.54056300321124));
#31751=CARTESIAN_POINT('Ctrl Pts',(95.3749453127051,-0.459244357691733,
-9.54373500078813));
#31752=CARTESIAN_POINT('Ctrl Pts',(95.3584106800634,-0.415374750742292,
-9.54690699836502));
#31753=CARTESIAN_POINT('Ctrl Pts',(95.3418463265242,-0.371426288452221,
-9.55008469758746));
#31754=CARTESIAN_POINT('Ctrl Pts',(95.3279404156537,-0.326553310719913,
-9.55326239680991));
#31755=CARTESIAN_POINT('Ctrl Pts',(95.3167705471221,-0.281107769043174,
-9.55644009603235));
#31756=CARTESIAN_POINT('Ctrl Pts',(95.3137943969909,-0.268999054026411,
-9.55728677653992));
#31757=CARTESIAN_POINT('Ctrl Pts',(95.311012202266,-0.25684973474927,-9.55813345704749));
#31758=CARTESIAN_POINT('Ctrl Pts',(95.3084248112407,-0.2446665416881,-9.55898013755506));
#31759=CARTESIAN_POINT('Ctrl Pts',(95.298365749979,-0.197301653982104,-9.56227179738204));
#31760=CARTESIAN_POINT('Ctrl Pts',(95.2912094176885,-0.14920650195639,-9.56556345720902));
#31761=CARTESIAN_POINT('Ctrl Pts',(95.2870498501539,-0.100769625416666,
-9.568855117036));
#31762=CARTESIAN_POINT('Ctrl Pts',(95.2830413499848,-0.0540918815927246,
-9.5720272302096));
#31763=CARTESIAN_POINT('Ctrl Pts',(95.2818157192262,-0.00709742288570371,
-9.57519934338319));
#31764=CARTESIAN_POINT('Ctrl Pts',(95.2834054806813,0.0398547741674446,
-9.57837145655678));
#31765=CARTESIAN_POINT('Ctrl Pts',(95.2849936621503,0.0867603077308272,
-9.58154041712241));
#31766=CARTESIAN_POINT('Ctrl Pts',(95.2893916789986,0.133623107969756,-9.58470937768803));
#31767=CARTESIAN_POINT('Ctrl Pts',(95.2965800354207,0.180082549199591,-9.58787833825366));
#31768=CARTESIAN_POINT('Ctrl Pts',(95.3037644127641,0.226516273037512,-9.59104554465697));
#31769=CARTESIAN_POINT('Ctrl Pts',(95.3137359849105,0.27254653004219,-9.59421275106028));
#31770=CARTESIAN_POINT('Ctrl Pts',(95.3264235423979,0.317818910265401,-9.59737995746359));
#31771=CARTESIAN_POINT('Ctrl Pts',(95.3391096627594,0.363086162463311,-9.60054680511584));
#31772=CARTESIAN_POINT('Ctrl Pts',(95.3545110052593,0.407595172278291,-9.6037136527681));
#31773=CARTESIAN_POINT('Ctrl Pts',(95.3725061662152,0.451005469222867,-9.60688050042035));
#31774=CARTESIAN_POINT('Ctrl Pts',(95.3905195439408,0.494459711058102,-9.61005055391968));
#31775=CARTESIAN_POINT('Ctrl Pts',(95.4111317638302,0.536812505535616,-9.61322060741901));
#31776=CARTESIAN_POINT('Ctrl Pts',(95.4341735615615,0.577744067736523,-9.61639066091834));
#31777=CARTESIAN_POINT('Ctrl Pts',(95.4572294046774,0.618700580227455,-9.61956264675912));
#31778=CARTESIAN_POINT('Ctrl Pts',(95.4827174703621,0.658233667833045,-9.6227346325999));
#31779=CARTESIAN_POINT('Ctrl Pts',(95.5104247906683,0.696051978963926,-9.62590661844068));
#31780=CARTESIAN_POINT('Ctrl Pts',(95.5381819171211,0.733938271564354,-9.62908430618227));
#31781=CARTESIAN_POINT('Ctrl Pts',(95.5681658979538,0.770103212244596,-9.63226199392386));
#31782=CARTESIAN_POINT('Ctrl Pts',(95.600124365354,0.804289506635592,-9.63543968166545));
#31783=CARTESIAN_POINT('Ctrl Pts',(95.608640393073,0.81339918724068,-9.63628644557784));
#31784=CARTESIAN_POINT('Ctrl Pts',(95.6172964320316,0.822368583475186,-9.63713320949022));
#31785=CARTESIAN_POINT('Ctrl Pts',(95.6260873072049,0.83119330607807,-9.63797997340261));
#31786=CARTESIAN_POINT('Ctrl Pts',(95.659076697028,0.864309714659412,-9.64115761206124));
#31787=CARTESIAN_POINT('Ctrl Pts',(95.6941138831242,0.895532572162974,-9.64433525071987));
#31788=CARTESIAN_POINT('Ctrl Pts',(95.7309530449706,0.92459942618441,-9.6475128893785));
#31789=CARTESIAN_POINT('Ctrl Pts',(95.7677301303009,0.953617300562,-9.65068517349791));
#31790=CARTESIAN_POINT('Ctrl Pts',(95.8063027412018,0.980486026979274,-9.65385745761732));
#31791=CARTESIAN_POINT('Ctrl Pts',(95.8463891762519,1.00498077416159,-9.65702974173673));
#31792=CARTESIAN_POINT('Ctrl Pts',(95.8709813003456,1.02000774928669,-9.65897586652003));
#31793=CARTESIAN_POINT('Ctrl Pts',(95.8961424522912,1.03414200586854,-9.66092199130333));
#31794=CARTESIAN_POINT('Ctrl Pts',(95.9218016730721,1.04733934308042,-9.66286811608663));
#31795=CARTESIAN_POINT('Origin',(96.460480949577,-7.19464945638997E-16,
0.924367114736168));
#31796=CARTESIAN_POINT('',(95.9218016730721,1.04733934308042,-10.2615611054409));
#31797=CARTESIAN_POINT('',(95.9218016730734,1.04733934308113,-10.1620395986893));
#31798=CARTESIAN_POINT('',(95.9218016730721,1.04733934308042,0.924367114736168));
#31799=CARTESIAN_POINT('',(97.6382305095403,-0.0010180895773768,-9.92436711477234));
#31800=CARTESIAN_POINT('Ctrl Pts',(97.6382305095403,-0.0010180895773768,
-9.92436711477234));
#31801=CARTESIAN_POINT('Ctrl Pts',(97.6381806027097,-0.0587514649425388,
-9.92826204859388));
#31802=CARTESIAN_POINT('Ctrl Pts',(97.6338815978861,-0.116299884304691,
-9.93215698241542));
#31803=CARTESIAN_POINT('Ctrl Pts',(97.625438007886,-0.173118788108036,-9.93605191623696));
#31804=CARTESIAN_POINT('Ctrl Pts',(97.6175259493788,-0.226360891431494,
-9.93970166051365));
#31805=CARTESIAN_POINT('Ctrl Pts',(97.6059752679963,-0.278962733452268,
-9.94335140479035));
#31806=CARTESIAN_POINT('Ctrl Pts',(97.5909097147114,-0.33049337278781,-9.94700114906704));
#31807=CARTESIAN_POINT('Ctrl Pts',(97.5773222760419,-0.376968227599609,
-9.95029280889402));
#31808=CARTESIAN_POINT('Ctrl Pts',(97.5608328375572,-0.422710422349559,
-9.953584468721));
#31809=CARTESIAN_POINT('Ctrl Pts',(97.5415427327874,-0.46733337499266,-9.95687612854798));
#31810=CARTESIAN_POINT('Ctrl Pts',(97.5229495237563,-0.510344229312774,
-9.96004887021799));
#31811=CARTESIAN_POINT('Ctrl Pts',(97.5017548078627,-0.552314770916328,
-9.96322161188801));
#31812=CARTESIAN_POINT('Ctrl Pts',(97.4781001221503,-0.592913384999275,
-9.96639435355802));
#31813=CARTESIAN_POINT('Ctrl Pts',(97.4544689782401,-0.633471594210228,
-9.96956393762711));
#31814=CARTESIAN_POINT('Ctrl Pts',(97.428382989555,-0.672660098913267,-9.97273352169621));
#31815=CARTESIAN_POINT('Ctrl Pts',(97.4000302804033,-0.710170484773801,
-9.9759031057653));
#31816=CARTESIAN_POINT('Ctrl Pts',(97.3716933177888,-0.747660038103485,
-9.97907092950972));
#31817=CARTESIAN_POINT('Ctrl Pts',(97.3410924639987,-0.783472874921223,
-9.98223875325413));
#31818=CARTESIAN_POINT('Ctrl Pts',(97.3084584366074,-0.817330559804014,
-9.98540657699855));
#31819=CARTESIAN_POINT('Ctrl Pts',(97.2758281805692,-0.851184331921751,
-9.98857403465325));
#31820=CARTESIAN_POINT('Ctrl Pts',(97.2411656054994,-0.883083001074866,
-9.99174149230796));
#31821=CARTESIAN_POINT('Ctrl Pts',(97.2047390264875,-0.912784189966875,
-9.99490894996267));
#31822=CARTESIAN_POINT('Ctrl Pts',(97.1682757546935,-0.942515297102116,
-9.9980795982226));
#31823=CARTESIAN_POINT('Ctrl Pts',(97.1300453672153,-0.970044155835744,
-10.0012502464825));
#31824=CARTESIAN_POINT('Ctrl Pts',(97.0903485259946,-0.995169281417913,
-10.0044208947425));
#31825=CARTESIAN_POINT('Ctrl Pts',(97.0506275949758,-1.02030965403694,-10.0075934670919));
#31826=CARTESIAN_POINT('Ctrl Pts',(97.0094389274154,-1.04304312138544,-10.0107660394414));
#31827=CARTESIAN_POINT('Ctrl Pts',(96.9671082056204,-1.06321394175111,-10.0139386117908));
#31828=CARTESIAN_POINT('Ctrl Pts',(96.9247016427121,-1.0834209008219,-10.0171168682253));
#31829=CARTESIAN_POINT('Ctrl Pts',(96.8811494611521,-1.10105584820427,-10.0202951246597));
#31830=CARTESIAN_POINT('Ctrl Pts',(96.8367959098715,-1.11601169938247,-10.0234733810941));
#31831=CARTESIAN_POINT('Ctrl Pts',(96.8250380789157,-1.11997639589215,-10.0243159157009));
#31832=CARTESIAN_POINT('Ctrl Pts',(96.813223998895,-1.12375309656353,-10.0251584503078));
#31833=CARTESIAN_POINT('Ctrl Pts',(96.8013602062103,-1.12734040772835,-10.0260009849146));
#31834=CARTESIAN_POINT('Ctrl Pts',(96.7550100985012,-1.14135550924732,-10.0292926447416));
#31835=CARTESIAN_POINT('Ctrl Pts',(96.707688119695,-1.15253944277112,-10.0325843045686));
#31836=CARTESIAN_POINT('Ctrl Pts',(96.6597734620364,-1.16076593548296,-10.0358759643956));
#31837=CARTESIAN_POINT('Ctrl Pts',(96.6135890375894,-1.16869536354693,-10.039048759987));
#31838=CARTESIAN_POINT('Ctrl Pts',(96.5668546157832,-1.1738772039746,-10.0422215555784));
#31839=CARTESIAN_POINT('Ctrl Pts',(96.5199253123462,-1.17624888107703,-10.0453943511699));
#31840=CARTESIAN_POINT('Ctrl Pts',(96.4730425246999,-1.17861820740015,-10.0485640019225));
#31841=CARTESIAN_POINT('Ctrl Pts',(96.4259657918948,-1.17818285547166,-10.0517336526751));
#31842=CARTESIAN_POINT('Ctrl Pts',(96.3790562392596,-1.17493194656105,-10.0549033034277));
#31843=CARTESIAN_POINT('Ctrl Pts',(96.3321725541524,-1.17168283031254,-10.0580712063267));
#31844=CARTESIAN_POINT('Ctrl Pts',(96.285456421646,-1.16562127115218,-10.0612391092258));
#31845=CARTESIAN_POINT('Ctrl Pts',(96.2392671177305,-1.15678844353658,-10.0644070121248));
#31846=CARTESIAN_POINT('Ctrl Pts',(96.193082973705,-1.14795660265201,-10.0675745611317));
#31847=CARTESIAN_POINT('Ctrl Pts',(96.1474260881076,-1.13635421467634,-10.0707421101386));
#31848=CARTESIAN_POINT('Ctrl Pts',(96.1026460672863,-1.12207364264383,-10.0739096591455));
#31849=CARTESIAN_POINT('Ctrl Pts',(96.0578206994124,-1.10777860921001,-10.0770804158109));
#31850=CARTESIAN_POINT('Ctrl Pts',(96.0138744993386,-1.09080015153705,-10.0802511724763));
#31851=CARTESIAN_POINT('Ctrl Pts',(95.9711404885939,-1.07128006410314,-10.0834219291416));
#31852=CARTESIAN_POINT('Ctrl Pts',(95.928380410353,-1.05174806953027,-10.0865946199499));
#31853=CARTESIAN_POINT('Ctrl Pts',(95.8868344850825,-1.02967162166471,-10.0897673107583));
#31854=CARTESIAN_POINT('Ctrl Pts',(95.8468110831302,-1.00523845803628,-10.0929400015666));
#31855=CARTESIAN_POINT('Ctrl Pts',(95.806715808977,-0.980761418446299,-10.0961183897485));
#31856=CARTESIAN_POINT('Ctrl Pts',(95.7681489670769,-0.953919541638821,
-10.0992967779304));
#31857=CARTESIAN_POINT('Ctrl Pts',(95.7313883121002,-0.924942694699029,
-10.1024751661123));
#31858=CARTESIAN_POINT('Ctrl Pts',(95.7216512258934,-0.917267367454935,
-10.1033170509956));
#31859=CARTESIAN_POINT('Ctrl Pts',(95.7120406676856,-0.909442456523787,
-10.1041589358789));
#31860=CARTESIAN_POINT('Ctrl Pts',(95.7025613640735,-0.901472664261251,
-10.1050008207622));
#31861=CARTESIAN_POINT('Ctrl Pts',(95.6654985262603,-0.87031181847344,-10.1082924805892));
#31862=CARTESIAN_POINT('Ctrl Pts',(95.6302740501501,-0.836788696719137,
-10.1115841404162));
#31863=CARTESIAN_POINT('Ctrl Pts',(95.5972018514032,-0.801151834021637,
-10.1148758002431));
#31864=CARTESIAN_POINT('Ctrl Pts',(95.5653691687261,-0.766850608677182,
-10.1180440916396));
#31865=CARTESIAN_POINT('Ctrl Pts',(95.5355307066674,-0.730591736558892,
-10.1212123830361));
#31866=CARTESIAN_POINT('Ctrl Pts',(95.5079326300622,-0.692637539763356,
-10.1243806744326));
#31867=CARTESIAN_POINT('Ctrl Pts',(95.4803619930838,-0.654721079257014,
-10.127545815728));
#31868=CARTESIAN_POINT('Ctrl Pts',(95.4550276605997,-0.615113080019186,
-10.1307109570233));
#31869=CARTESIAN_POINT('Ctrl Pts',(95.432135823626,-0.574109192081777,-10.1338760983186));
#31870=CARTESIAN_POINT('Ctrl Pts',(95.409256602328,-0.533127901358906,-10.1370394953067));
#31871=CARTESIAN_POINT('Ctrl Pts',(95.3888174824896,-0.490752732971964,
-10.1402028922948));
#31872=CARTESIAN_POINT('Ctrl Pts',(95.3709800685385,-0.447306262773352,
-10.1433662892829));
#31873=CARTESIAN_POINT('Ctrl Pts',(95.3531445804579,-0.403864483404788,
-10.1465293447253));
#31874=CARTESIAN_POINT('Ctrl Pts',(95.3379104508013,-0.359352149587515,
-10.1496924001676));
#31875=CARTESIAN_POINT('Ctrl Pts',(95.325391134186,-0.314111721359853,-10.15285545561));
#31876=CARTESIAN_POINT('Ctrl Pts',(95.3128589183797,-0.268824679970558,
-10.1560217700846));
#31877=CARTESIAN_POINT('Ctrl Pts',(95.3030472442471,-0.222808587547782,
-10.1591880845592));
#31878=CARTESIAN_POINT('Ctrl Pts',(95.296019103629,-0.176419023439901,-10.1623543990338));
#31879=CARTESIAN_POINT('Ctrl Pts',(95.2889866142775,-0.130000755317308,
-10.1655226726977));
#31880=CARTESIAN_POINT('Ctrl Pts',(95.2847411354154,-0.0832091126481367,
-10.1686909463616));
#31881=CARTESIAN_POINT('Ctrl Pts',(95.2832937069446,-0.036404097071164,
-10.1718592200254));
#31882=CARTESIAN_POINT('Ctrl Pts',(95.281843638736,0.0104862788335729,-10.1750332718068));
#31883=CARTESIAN_POINT('Ctrl Pts',(95.2832017799413,0.0573895182780501,
-10.1782073235882));
#31884=CARTESIAN_POINT('Ctrl Pts',(95.2873271589674,0.103948285595506,-10.1813813753695));
#31885=CARTESIAN_POINT('Ctrl Pts',(95.2884619364942,0.116755313142996,-10.1822544691163));
#31886=CARTESIAN_POINT('Ctrl Pts',(95.2898057970335,0.129536330417853,-10.183127562863));
#31887=CARTESIAN_POINT('Ctrl Pts',(95.2913572126147,0.142284047494008,-10.1840006566098));
#31888=CARTESIAN_POINT('Ctrl Pts',(95.2970996509865,0.189468683626648,-10.1872323419777));
#31889=CARTESIAN_POINT('Ctrl Pts',(95.3057158572815,0.23640975042499,-10.1904640273457));
#31890=CARTESIAN_POINT('Ctrl Pts',(95.3171708708936,0.282731544899127,-10.1936957127137));
#31891=CARTESIAN_POINT('Ctrl Pts',(95.3284350764437,0.328281749558332,-10.1968735673624));
#31892=CARTESIAN_POINT('Ctrl Pts',(95.3424441166781,0.373232591477927,-10.200051422011));
#31893=CARTESIAN_POINT('Ctrl Pts',(95.3591127838168,0.417232819838045,-10.2032292766597));
#31894=CARTESIAN_POINT('Ctrl Pts',(95.3757644930239,0.461188284399328,-10.2064038983059));
#31895=CARTESIAN_POINT('Ctrl Pts',(95.3950702767673,0.504194532880133,-10.2095785199522));
#31896=CARTESIAN_POINT('Ctrl Pts',(95.4168951568967,0.5459155207683,-10.2127531415984));
#31897=CARTESIAN_POINT('Ctrl Pts',(95.4387073502604,0.587612256317345,-10.2159259178425));
#31898=CARTESIAN_POINT('Ctrl Pts',(95.463035481669,0.628024720293765,-10.2190986940865));
#31899=CARTESIAN_POINT('Ctrl Pts',(95.4896976141636,0.666839394594824,-10.2222714703306));
#31900=CARTESIAN_POINT('Ctrl Pts',(95.5172115161952,0.706894073129085,-10.2255456065898));
#31901=CARTESIAN_POINT('Ctrl Pts',(95.5472108300608,0.745246560407001,-10.228819742849));
#31902=CARTESIAN_POINT('Ctrl Pts',(95.5794474925356,0.781584998623714,-10.2320938791082));
#31903=CARTESIAN_POINT('Ctrl Pts',(95.6107103637616,0.816825740912519,-10.2352691116661));
#31904=CARTESIAN_POINT('Ctrl Pts',(95.6440768495125,0.850172045732689,-10.238444344224));
#31905=CARTESIAN_POINT('Ctrl Pts',(95.6792821897892,0.881375947145148,-10.2416195767818));
#31906=CARTESIAN_POINT('Ctrl Pts',(95.7161324198789,0.914037780199677,-10.2449431648917));
#31907=CARTESIAN_POINT('Ctrl Pts',(95.7549970966545,0.944351592302617,-10.2482667530015));
#31908=CARTESIAN_POINT('Ctrl Pts',(95.7955356627768,0.972081698244651,-10.2515903411114));
#31909=CARTESIAN_POINT('Ctrl Pts',(95.8360742288991,0.999811804186684,-10.2549139292212));
#31910=CARTESIAN_POINT('Ctrl Pts',(95.8782860580672,1.02495790561954,-10.258237517331));
#31911=CARTESIAN_POINT('Ctrl Pts',(95.9218016730721,1.04733934308042,-10.2615611054409));
#31912=CARTESIAN_POINT('Ctrl Pts',(97.6382305277127,-0.000996845613527347,
-9.92470885738545));
#31913=CARTESIAN_POINT('Ctrl Pts',(97.6382801538142,0.0576352226910313,
-9.92106407212053));
#31914=CARTESIAN_POINT('Ctrl Pts',(97.6339515452507,0.116183996103659,-9.91737201317258));
#31915=CARTESIAN_POINT('Ctrl Pts',(97.6238067638071,0.184031654702508,-9.91289245550959));
#31916=CARTESIAN_POINT('Ctrl Pts',(97.6222061158262,0.193879417203326,-9.91223740586212));
#31917=CARTESIAN_POINT('Ctrl Pts',(97.6193519863662,0.210132245002773,-9.91114761288391));
#31918=CARTESIAN_POINT('Ctrl Pts',(97.6181700119439,0.216549468599535,-9.91071506970433));
#31919=CARTESIAN_POINT('Ctrl Pts',(97.6159496139914,0.228066461839842,-9.90993456331032));
#31920=CARTESIAN_POINT('Ctrl Pts',(97.6149305902757,0.23316983313823,-9.90958721204438));
#31921=CARTESIAN_POINT('Ctrl Pts',(97.612781071909,0.243575201327294,-9.90887584716385));
#31922=CARTESIAN_POINT('Ctrl Pts',(97.6116477269105,0.248876474805634,-9.90851175165997));
#31923=CARTESIAN_POINT('Ctrl Pts',(97.6091280253929,0.260276926404082,-9.90772506175124));
#31924=CARTESIAN_POINT('Ctrl Pts',(97.6077296053299,0.266373239017963,-9.9073020952274));
#31925=CARTESIAN_POINT('Ctrl Pts',(97.6038060038904,0.282873650352228,-9.90615091679084));
#31926=CARTESIAN_POINT('Ctrl Pts',(97.6011874598654,0.293254712049666,-9.90541976628536));
#31927=CARTESIAN_POINT('Ctrl Pts',(97.5865027625952,0.348295873656591,-9.90150522238407));
#31928=CARTESIAN_POINT('Ctrl Pts',(97.5719561322038,0.392246196541245,-9.89824351155558));
#31929=CARTESIAN_POINT('Ctrl Pts',(97.5366792409662,0.480951256307829,-9.89137881289994));
#31930=CARTESIAN_POINT('Ctrl Pts',(97.5156464724481,0.525492147390015,-9.88777371580748));
#31931=CARTESIAN_POINT('Ctrl Pts',(97.4705037390419,0.60738098579193,-9.88091039758668));
#31932=CARTESIAN_POINT('Ctrl Pts',(97.4469431123053,0.644942230630121,-9.87765930526512));
#31933=CARTESIAN_POINT('Ctrl Pts',(97.4063947070613,0.702145596063801,-9.87262071329951));
#31934=CARTESIAN_POINT('Ctrl Pts',(97.3907787047892,0.722708512700614,-9.87079041578914));
#31935=CARTESIAN_POINT('Ctrl Pts',(97.3707439113849,0.747363259811054,-9.8685875323534));
#31936=CARTESIAN_POINT('Ctrl Pts',(97.3669545463751,0.751954868190861,-9.86817691037815));
#31937=CARTESIAN_POINT('Ctrl Pts',(97.3609182142219,0.75915720110132,-9.86753249685616));
#31938=CARTESIAN_POINT('Ctrl Pts',(97.3586943954495,0.761787063403281,-9.86729712777962));
#31939=CARTESIAN_POINT('Ctrl Pts',(97.3544644337586,0.766745092457972,-9.86685332409398));
#31940=CARTESIAN_POINT('Ctrl Pts',(97.3524607296352,0.769075145214535,-9.86664473566317));
#31941=CARTESIAN_POINT('Ctrl Pts',(97.3477769109046,0.774478901664052,-9.86616088602439));
#31942=CARTESIAN_POINT('Ctrl Pts',(97.3450899226037,0.777546563358099,-9.86588612819152));
#31943=CARTESIAN_POINT('Ctrl Pts',(97.3361954144138,0.787595395004082,-9.86498558587274));
#31944=CARTESIAN_POINT('Ctrl Pts',(97.3299205775717,0.79451688268189,-9.86436448864603));
#31945=CARTESIAN_POINT('Ctrl Pts',(97.2679616180738,0.861247814878739,-9.85835974938475));
#31946=CARTESIAN_POINT('Ctrl Pts',(97.2062692065016,0.915192176240851,-9.85336299830011));
#31947=CARTESIAN_POINT('Ctrl Pts',(97.0969737343874,0.992309519403442,-9.84508316506271));
#31948=CARTESIAN_POINT('Ctrl Pts',(97.0525303908639,1.01944990511408,-9.84184905581689));
#31949=CARTESIAN_POINT('Ctrl Pts',(96.9889517237128,1.05271236413513,-9.83726348600444));
#31950=CARTESIAN_POINT('Ctrl Pts',(96.9712354578083,1.06142095652103,-9.8359902521145));
#31951=CARTESIAN_POINT('Ctrl Pts',(96.9399081945275,1.07585421641041,-9.83374015045288));
#31952=CARTESIAN_POINT('Ctrl Pts',(96.9263926018372,1.0817758912957,-9.83276982234651));
#31953=CARTESIAN_POINT('Ctrl Pts',(96.9064821015594,1.09005706697645,-9.83133925015582));
#31954=CARTESIAN_POINT('Ctrl Pts',(96.9001719515042,1.09261761673607,-9.83088570534459));
#31955=CARTESIAN_POINT('Ctrl Pts',(96.8887371588211,1.09714256089942,-9.83006336162246));
#31956=CARTESIAN_POINT('Ctrl Pts',(96.883620281411,1.09912614554078,-9.82969521096513));
#31957=CARTESIAN_POINT('Ctrl Pts',(96.8729364203986,1.103182139054,-9.82892608882737));
#31958=CARTESIAN_POINT('Ctrl Pts',(96.8673672593067,1.10524833230617,-9.82852492460978));
#31959=CARTESIAN_POINT('Ctrl Pts',(96.8528274858839,1.11051789247242,-9.82747681654377));
#31960=CARTESIAN_POINT('Ctrl Pts',(96.8438333698294,1.11365466222764,-9.8268277167494));
#31961=CARTESIAN_POINT('Ctrl Pts',(96.8060362470582,1.12632458584874,-9.82409612623462));
#31962=CARTESIAN_POINT('Ctrl Pts',(96.7769107040048,1.13485129356437,-9.82198164721496));
#31963=CARTESIAN_POINT('Ctrl Pts',(96.6664565976677,1.16260491853207,-9.81392200863383));
#31964=CARTESIAN_POINT('Ctrl Pts',(96.5834940684395,1.17428296453015,-9.8077649385387));
#31965=CARTESIAN_POINT('Ctrl Pts',(96.4477045517467,1.17884292769989,-9.79781929621551));
#31966=CARTESIAN_POINT('Ctrl Pts',(96.3953347810975,1.17711136635979,-9.79402209813135));
#31967=CARTESIAN_POINT('Ctrl Pts',(96.3363194618872,1.17120770129634,-9.78989694955664));
#31968=CARTESIAN_POINT('Ctrl Pts',(96.3293964913265,1.17045308546199,-9.7894154967316));
#31969=CARTESIAN_POINT('Ctrl Pts',(96.3188416492059,1.16920776426879,-9.78868563083916));
#31970=CARTESIAN_POINT('Ctrl Pts',(96.315204843989,1.16876145620009,-9.78843490215801));
#31971=CARTESIAN_POINT('Ctrl Pts',(96.308551238925,1.16791339028995,-9.78797764555098));
#31972=CARTESIAN_POINT('Ctrl Pts',(96.3055339004876,1.16751691064055,-9.78777084096204));
#31973=CARTESIAN_POINT('Ctrl Pts',(96.2987258050736,1.16659546546901,-9.78730546124991));
#31974=CARTESIAN_POINT('Ctrl Pts',(96.2949360477026,1.16606371752286,-9.78704726413025));
#31975=CARTESIAN_POINT('Ctrl Pts',(96.2851469566983,1.16464150575536,-9.7863823947235));
#31976=CARTESIAN_POINT('Ctrl Pts',(96.2791516997647,1.1637231427491,-9.78597720705927));
#31977=CARTESIAN_POINT('Ctrl Pts',(96.2389314744389,1.15724377140681,-9.78327080496709));
#31978=CARTESIAN_POINT('Ctrl Pts',(96.2049558135718,1.15021942579944,-9.78104224921283));
#31979=CARTESIAN_POINT('Ctrl Pts',(96.144034545726,1.134790700971,-9.77707133712284));
#31980=CARTESIAN_POINT('Ctrl Pts',(96.1169884396967,1.12689896503417,-9.77531763904385));
#31981=CARTESIAN_POINT('Ctrl Pts',(96.0447474830146,1.10297701717483,-9.77059927321858));
#31982=CARTESIAN_POINT('Ctrl Pts',(96.0002077029332,1.08514564095304,-9.76765156992421));
#31983=CARTESIAN_POINT('Ctrl Pts',(95.9450885397877,1.05907310395355,-9.76383858890257));
#31984=CARTESIAN_POINT('Ctrl Pts',(95.933394606705,1.05330195059611,-9.76301990498141));
#31985=CARTESIAN_POINT('Ctrl Pts',(95.9218016501122,1.04733933127145,-9.76219702307975));
#31986=CARTESIAN_POINT('',(97.6382307323089,0.000715384519801949,-9.8256328852061));
#31987=CARTESIAN_POINT('Ctrl Pts',(95.9218016730721,1.04733934308042,-9.66286811608663));
#31988=CARTESIAN_POINT('Ctrl Pts',(95.9635682821251,1.06882121225243,-9.66603590647616));
#31989=CARTESIAN_POINT('Ctrl Pts',(96.0066556356306,1.08781817527742,-9.6692036968657));
#31990=CARTESIAN_POINT('Ctrl Pts',(96.0507368574096,1.10417609167826,-9.67237148725523));
#31991=CARTESIAN_POINT('Ctrl Pts',(96.0948048958174,1.12052911591698,-9.67553833025368));
#31992=CARTESIAN_POINT('Ctrl Pts',(96.1398656906136,1.13424446519297,-9.67870517325213));
#31993=CARTESIAN_POINT('Ctrl Pts',(96.1855734795076,1.14521654956608,-9.68187201625059));
#31994=CARTESIAN_POINT('Ctrl Pts',(96.2313214648289,1.15619828302968,-9.68504164423989));
#31995=CARTESIAN_POINT('Ctrl Pts',(96.2777170379303,1.16443180029753,-9.6882112722292));
#31996=CARTESIAN_POINT('Ctrl Pts',(96.3244022900723,1.16986224014941,-9.69138090021851));
#31997=CARTESIAN_POINT('Ctrl Pts',(96.3711082203464,1.17529508528663,-9.69455193211983));
#31998=CARTESIAN_POINT('Ctrl Pts',(96.418103527799,1.17792234517528,-9.69772296402114));
#31999=CARTESIAN_POINT('Ctrl Pts',(96.4650268891008,1.1777412266427,-9.70089399592246));
#32000=CARTESIAN_POINT('Ctrl Pts',(96.5120406832511,1.17755975905019,-9.70407113918151));
#32001=CARTESIAN_POINT('Ctrl Pts',(96.5589816965096,1.1745591380844,-9.70724828244057));
#32002=CARTESIAN_POINT('Ctrl Pts',(96.6054919617845,1.16878863308921,-9.71042542569963));
#32003=CARTESIAN_POINT('Ctrl Pts',(96.6374752134872,1.16482048729125,-9.71261022021648));
#32004=CARTESIAN_POINT('Ctrl Pts',(96.6692548903594,1.15954362425323,-9.71479501473333));
#32005=CARTESIAN_POINT('Ctrl Pts',(96.7007181266502,1.15298792762625,-9.71697980925018));
#32006=CARTESIAN_POINT('Ctrl Pts',(96.7481213355683,1.14311096983527,-9.72027146907716));
#32007=CARTESIAN_POINT('Ctrl Pts',(96.795023380856,1.13028308657472,-9.72356312890414));
#32008=CARTESIAN_POINT('Ctrl Pts',(96.841030772512,1.11457475961201,-9.72685478873112));
#32009=CARTESIAN_POINT('Ctrl Pts',(96.8853676900685,1.09943678346448,-9.73002693227416));
#32010=CARTESIAN_POINT('Ctrl Pts',(96.9288732279279,1.08162415454859,-9.73319907581719));
#32011=CARTESIAN_POINT('Ctrl Pts',(96.9712057273268,1.06125174388191,-9.73637121936022));
#32012=CARTESIAN_POINT('Ctrl Pts',(97.0134961557979,1.04089957974523,-9.73954021036031));
#32013=CARTESIAN_POINT('Ctrl Pts',(97.0546153529805,1.01799290967789,-9.7427092013604));
#32014=CARTESIAN_POINT('Ctrl Pts',(97.0942411095978,0.99269487863614,-9.74587819236049));
#32015=CARTESIAN_POINT('Ctrl Pts',(97.1338449318395,0.967410851024522,-9.74904542920256));
#32016=CARTESIAN_POINT('Ctrl Pts',(97.1719564818968,0.939738384116108,-9.75221266604463));
#32017=CARTESIAN_POINT('Ctrl Pts',(97.2082800752212,0.909885448936166,-9.7553799028867));
#32018=CARTESIAN_POINT('Ctrl Pts',(97.2445995535471,0.880035895711941,-9.75854678092135));
#32019=CARTESIAN_POINT('Ctrl Pts',(97.2791310481007,0.848006720107118,-9.761713658956));
#32020=CARTESIAN_POINT('Ctrl Pts',(97.3116118558093,0.814046216720059,-9.76488053699065));
#32021=CARTESIAN_POINT('Ctrl Pts',(97.3441255408362,0.780051338255487,-9.76805062056311));
#32022=CARTESIAN_POINT('Ctrl Pts',(97.3745840125977,0.744121636176582,-9.77122070413557));
#32023=CARTESIAN_POINT('Ctrl Pts',(97.4027627835324,0.706540874895221,-9.77439078770804));
#32024=CARTESIAN_POINT('Ctrl Pts',(97.4309587296713,0.66893720781536,-9.77756280347381));
#32025=CARTESIAN_POINT('Ctrl Pts',(97.4568719028352,0.629680944506121,-9.78073481923959));
#32026=CARTESIAN_POINT('Ctrl Pts',(97.4803214470516,0.589084393114236,-9.78390683500536));
#32027=CARTESIAN_POINT('Ctrl Pts',(97.5038131395076,0.548414873431017,-9.78708455215617));
#32028=CARTESIAN_POINT('Ctrl Pts',(97.5248321236364,0.506400759705283,-9.79026226930698));
#32029=CARTESIAN_POINT('Ctrl Pts',(97.5432445882813,0.463376699025593,-9.79343998645779));
#32030=CARTESIAN_POINT('Ctrl Pts',(97.5481497211905,0.451914966987065,-9.79428653933777));
#32031=CARTESIAN_POINT('Ctrl Pts',(97.5528701407934,0.440381647634523,-9.79513309221775));
#32032=CARTESIAN_POINT('Ctrl Pts',(97.5574039162688,0.428783240862008,-9.79597964509773));
#32033=CARTESIAN_POINT('Ctrl Pts',(97.5766340932484,0.379588167985355,-9.79957033056353));
#32034=CARTESIAN_POINT('Ctrl Pts',(97.5925738799491,0.329038825425604,-9.80316101602933));
#32035=CARTESIAN_POINT('Ctrl Pts',(97.6050574650756,0.277560196478159,-9.80675170149513));
#32036=CARTESIAN_POINT('Ctrl Pts',(97.6174476028956,0.22646691670523,-9.81031550847352));
#32037=CARTESIAN_POINT('Ctrl Pts',(97.6264329545018,0.174458471699299,-9.81387931545191));
#32038=CARTESIAN_POINT('Ctrl Pts',(97.6318980705591,0.121971271904094,-9.8174431224303));
#32039=CARTESIAN_POINT('Ctrl Pts',(97.6360844181291,0.0817654173506131,
-9.82017304335557));
#32040=CARTESIAN_POINT('Ctrl Pts',(97.6382060932456,0.0412790962920784,
-9.82290296428083));
#32041=CARTESIAN_POINT('Ctrl Pts',(97.6382307323089,0.000715384519801949,
-9.8256328852061));
#32042=CARTESIAN_POINT('Ctrl Pts',(95.9218016730735,1.04733934308113,-10.1620395986893));
#32043=CARTESIAN_POINT('Ctrl Pts',(95.888261773431,1.03008872703891,-10.1593489153631));
#32044=CARTESIAN_POINT('Ctrl Pts',(95.8555669796334,1.01123548773281,-10.1567049044136));
#32045=CARTESIAN_POINT('Ctrl Pts',(95.8152007394698,0.985298798942619,-10.1534117848218));
#32046=CARTESIAN_POINT('Ctrl Pts',(95.8066439065627,0.979641467820415,-10.1527119137219));
#32047=CARTESIAN_POINT('Ctrl Pts',(95.7931180721235,0.970442712425622,-10.1516024355852));
#32048=CARTESIAN_POINT('Ctrl Pts',(95.7881009549726,0.966973326194928,-10.1511901840541));
#32049=CARTESIAN_POINT('Ctrl Pts',(95.7791000189668,0.960645162991395,-10.1504491972815));
#32050=CARTESIAN_POINT('Ctrl Pts',(95.7751067001287,0.957800209444742,-10.1501199537778));
#32051=CARTESIAN_POINT('Ctrl Pts',(95.7657386763271,0.951037575232609,-10.1493463161735));
#32052=CARTESIAN_POINT('Ctrl Pts',(95.7603791214077,0.947099112546189,-10.1489027235269));
#32053=CARTESIAN_POINT('Ctrl Pts',(95.7447527531734,0.935410961680217,-10.1476062117876));
#32054=CARTESIAN_POINT('Ctrl Pts',(95.7345789796638,0.92753806905986,-10.1467580444287));
#32055=CARTESIAN_POINT('Ctrl Pts',(95.7117338453776,0.909253385134437,-10.1448423971243));
#32056=CARTESIAN_POINT('Ctrl Pts',(95.6991467431417,0.898740346372868,-10.1437789092505));
#32057=CARTESIAN_POINT('Ctrl Pts',(95.6575631723686,0.862508015541709,-10.1402313511631));
#32058=CARTESIAN_POINT('Ctrl Pts',(95.6296165622779,0.835620584606594,-10.1377903359856));
#32059=CARTESIAN_POINT('Ctrl Pts',(95.5598933337758,0.761576684689437,-10.1314499105702));
#32060=CARTESIAN_POINT('Ctrl Pts',(95.5204864392328,0.712367189311339,-10.1276048056369));
#32061=CARTESIAN_POINT('Ctrl Pts',(95.4796709869745,0.652076839046914,-10.1230383661827));
#32062=CARTESIAN_POINT('Ctrl Pts',(95.4742434635255,0.643838489605852,-10.1224171507759));
#32063=CARTESIAN_POINT('Ctrl Pts',(95.4511054372985,0.607738466445831,-10.1197026822154));
#32064=CARTESIAN_POINT('Ctrl Pts',(95.4344690216764,0.579209847484569,-10.1175772682531));
#32065=CARTESIAN_POINT('Ctrl Pts',(95.4162608407933,0.544734070495049,-10.1149863272038));
#32066=CARTESIAN_POINT('Ctrl Pts',(95.4135077266959,0.539423683243594,-10.1145866235292));
#32067=CARTESIAN_POINT('Ctrl Pts',(95.4090715302349,0.530704949517532,-10.1139289987079));
#32068=CARTESIAN_POINT('Ctrl Pts',(95.4073642468499,0.527308941652815,-10.113672509593));
#32069=CARTESIAN_POINT('Ctrl Pts',(95.4043211380382,0.521182076564831,-10.1132090510234));
#32070=CARTESIAN_POINT('Ctrl Pts',(95.4029794111144,0.518454241117204,-10.1130024474001));
#32071=CARTESIAN_POINT('Ctrl Pts',(95.4000367101134,0.512412550330849,-10.1125442644445));
#32072=CARTESIAN_POINT('Ctrl Pts',(95.398440721472,0.509096414939712,-10.1122923984972));
#32073=CARTESIAN_POINT('Ctrl Pts',(95.3938304133719,0.499401117595293,-10.1115550329371));
#32074=CARTESIAN_POINT('Ctrl Pts',(95.3908579078187,0.493002418947527,-10.1110671402633));
#32075=CARTESIAN_POINT('Ctrl Pts',(95.3635579726657,0.432826586599409,-10.1064697672331));
#32076=CARTESIAN_POINT('Ctrl Pts',(95.343250749446,0.377324657832871,-10.1021662847394));
#32077=CARTESIAN_POINT('Ctrl Pts',(95.3002693628489,0.225362255868542,-10.090584592765));
#32078=CARTESIAN_POINT('Ctrl Pts',(95.2854404327732,0.127148103675182,-10.083342344266));
#32079=CARTESIAN_POINT('Ctrl Pts',(95.2827266604897,0.0139346068543939,
-10.0755098723727));
#32080=CARTESIAN_POINT('Ctrl Pts',(95.2826442712784,-0.000359380236713434,
-10.0745292631217));
#32081=CARTESIAN_POINT('Ctrl Pts',(95.2829082815413,-0.0215794457754825,
-10.0730851979032));
#32082=CARTESIAN_POINT('Ctrl Pts',(95.2830555977114,-0.0285062330002688,
-10.0726156634369));
#32083=CARTESIAN_POINT('Ctrl Pts',(95.2834277714089,-0.0408717785347733,
-10.0717806325756));
#32084=CARTESIAN_POINT('Ctrl Pts',(95.283629225366,-0.0463109862119375,
-10.0714144253475));
#32085=CARTESIAN_POINT('Ctrl Pts',(95.2841356235354,-0.0578249888279326,
-10.0706414539736));
#32086=CARTESIAN_POINT('Ctrl Pts',(95.2844499354126,-0.0638992292770024,
-10.0702349898058));
#32087=CARTESIAN_POINT('Ctrl Pts',(95.2854172200213,-0.0801518116237249,
-10.0691507884375));
#32088=CARTESIAN_POINT('Ctrl Pts',(95.2861553823033,-0.0903247152776928,
-10.068475690877));
#32089=CARTESIAN_POINT('Ctrl Pts',(95.2906289953621,-0.142566142722666,
-10.0650251361004));
#32090=CARTESIAN_POINT('Ctrl Pts',(95.2964933534475,-0.184423914363375,
-10.0623163953557));
#32091=CARTESIAN_POINT('Ctrl Pts',(95.3258637503889,-0.334719792393613,
-10.0526567048008));
#32092=CARTESIAN_POINT('Ctrl Pts',(95.3623944572716,-0.439992172540652,
-10.046062538312));
#32093=CARTESIAN_POINT('Ctrl Pts',(95.4200956534769,-0.55220270225605,-10.0378572284002));
#32094=CARTESIAN_POINT('Ctrl Pts',(95.4273602683316,-0.56567746326182,-10.0368499613925));
#32095=CARTESIAN_POINT('Ctrl Pts',(95.4374233055472,-0.583502166092287,
-10.035482718913));
#32096=CARTESIAN_POINT('Ctrl Pts',(95.4399911069541,-0.587981461865471,
-10.035136140243));
#32097=CARTESIAN_POINT('Ctrl Pts',(95.4440694523484,-0.594988572672264,
-10.0345890214545));
#32098=CARTESIAN_POINT('Ctrl Pts',(95.4455602050996,-0.597527920064433,
-10.0343897177194));
#32099=CARTESIAN_POINT('Ctrl Pts',(95.4486397775407,-0.602728889068124,
-10.0339793373284));
#32100=CARTESIAN_POINT('Ctrl Pts',(95.4502295895196,-0.605389841116122,
-10.0337681917898));
#32101=CARTESIAN_POINT('Ctrl Pts',(95.4540610766905,-0.611745682069473,
-10.0332610625066));
#32102=CARTESIAN_POINT('Ctrl Pts',(95.4563126085743,-0.615434546903135,
-10.032964457346));
#32103=CARTESIAN_POINT('Ctrl Pts',(95.4641120340017,-0.628056224711486,
-10.0319419969388));
#32104=CARTESIAN_POINT('Ctrl Pts',(95.4697590395076,-0.636926773730438,
-10.0312102471663));
#32105=CARTESIAN_POINT('Ctrl Pts',(95.4839014940081,-0.658499140600936,
-10.029400354284));
#32106=CARTESIAN_POINT('Ctrl Pts',(95.4925266734307,-0.671113271764405,
-10.0283157031952));
#32107=CARTESIAN_POINT('Ctrl Pts',(95.5292590425077,-0.722651923900813,
-10.0237843863106));
#32108=CARTESIAN_POINT('Ctrl Pts',(95.5594867214393,-0.760005873761361,
-10.0202613152457));
#32109=CARTESIAN_POINT('Ctrl Pts',(95.6514427378895,-0.860420361980952,
-10.0102684222191));
#32110=CARTESIAN_POINT('Ctrl Pts',(95.7181000901939,-0.918554465293736,
-10.0038521042937));
#32111=CARTESIAN_POINT('Ctrl Pts',(95.8018228052623,-0.976447435199542,
-9.99680235943189));
#32112=CARTESIAN_POINT('Ctrl Pts',(95.8131462367423,-0.983990823712108,
-9.99586726028539));
#32113=CARTESIAN_POINT('Ctrl Pts',(95.8304001477105,-0.995058167986903,
-9.9944692739616));
#32114=CARTESIAN_POINT('Ctrl Pts',(95.8362347074016,-0.998728795613086,
-9.99400105322965));
#32115=CARTESIAN_POINT('Ctrl Pts',(95.8464380625732,-1.00502356268872,-9.99318994388906));
#32116=CARTESIAN_POINT('Ctrl Pts',(95.850792235726,-1.00767092954312,-9.99284621911854));
#32117=CARTESIAN_POINT('Ctrl Pts',(95.8599331017923,-1.01314769925201,-9.99212957445861));
#32118=CARTESIAN_POINT('Ctrl Pts',(95.864722935638,-1.01597163769923,-9.99175685755465));
#32119=CARTESIAN_POINT('Ctrl Pts',(95.8761752479715,-1.02261472716414,-9.9908722483766));
#32120=CARTESIAN_POINT('Ctrl Pts',(95.8828554903665,-1.02640287736543,-9.99036146787082));
#32121=CARTESIAN_POINT('Ctrl Pts',(95.9057764301352,-1.03910595056267,-9.98862612915265));
#32122=CARTESIAN_POINT('Ctrl Pts',(95.9221907267037,-1.04770319137999,-9.98741267845175));
#32123=CARTESIAN_POINT('Ctrl Pts',(96.0027687103406,-1.08751326578403,-9.98158374131929));
#32124=CARTESIAN_POINT('Ctrl Pts',(96.0694775105861,-1.11324006429486,-9.97715581258178));
#32125=CARTESIAN_POINT('Ctrl Pts',(96.2113855190697,-1.15362494479511,-9.96802786074716));
#32126=CARTESIAN_POINT('Ctrl Pts',(96.2865000091455,-1.16731586352173,-9.96334830735557));
#32127=CARTESIAN_POINT('Ctrl Pts',(96.3718587889917,-1.17444936888773,-9.95770514904642));
#32128=CARTESIAN_POINT('Ctrl Pts',(96.3813291240349,-1.17512560262499,-9.95707448747302));
#32129=CARTESIAN_POINT('Ctrl Pts',(96.3946503808759,-1.17591505991703,-9.95617966354205));
#32130=CARTESIAN_POINT('Ctrl Pts',(96.3984955613975,-1.17612401664654,-9.95592047000262));
#32131=CARTESIAN_POINT('Ctrl Pts',(96.4054558151129,-1.17646802715395,-9.95544955249841));
#32132=CARTESIAN_POINT('Ctrl Pts',(96.4085705675512,-1.17660957680288,-9.95523818191956));
#32133=CARTESIAN_POINT('Ctrl Pts',(96.414953207416,-1.17687424195171,-9.954803688138));
#32134=CARTESIAN_POINT('Ctrl Pts',(96.4182210942268,-1.1769961175118,-9.95458050267244));
#32135=CARTESIAN_POINT('Ctrl Pts',(96.4266433346419,-1.17727510402364,-9.95400349326213));
#32136=CARTESIAN_POINT('Ctrl Pts',(96.4317982212409,-1.17741197266356,-9.95364859493921));
#32137=CARTESIAN_POINT('Ctrl Pts',(96.4536926575093,-1.17784943243337,-9.95213431927845));
#32138=CARTESIAN_POINT('Ctrl Pts',(96.470435786317,-1.17782689578065,-9.95095918858546));
#32139=CARTESIAN_POINT('Ctrl Pts',(96.516446127152,-1.17678392128936,-9.94769264404571));
#32140=CARTESIAN_POINT('Ctrl Pts',(96.5456838042588,-1.17502882621059,-9.94557558481078));
#32141=CARTESIAN_POINT('Ctrl Pts',(96.6690472386191,-1.16299515942741,-9.93653961912611));
#32142=CARTESIAN_POINT('Ctrl Pts',(96.7618363369293,-1.14247424365495,-9.92952377618136));
#32143=CARTESIAN_POINT('Ctrl Pts',(96.8786796636577,-1.1013878588755,-9.92077063703396));
#32144=CARTESIAN_POINT('Ctrl Pts',(96.9058218443952,-1.0906957066487,-9.91873992702453));
#32145=CARTESIAN_POINT('Ctrl Pts',(96.9411448422072,-1.07524205382913,-9.91609879669278));
#32146=CARTESIAN_POINT('Ctrl Pts',(96.9497033041997,-1.07137516706136,-9.91545896774468));
#32147=CARTESIAN_POINT('Ctrl Pts',(96.9635704411533,-1.06490889063338,-9.9144221716096));
#32148=CARTESIAN_POINT('Ctrl Pts',(96.9689072742165,-1.06237124231196,-9.91402313230847));
#32149=CARTESIAN_POINT('Ctrl Pts',(96.9790714965607,-1.05744404901172,-9.91326300862201));
#32150=CARTESIAN_POINT('Ctrl Pts',(96.9839020198036,-1.0550613522902,-9.91290170191342));
#32151=CARTESIAN_POINT('Ctrl Pts',(96.9950258677392,-1.04947921939243,-9.91206944042876));
#32152=CARTESIAN_POINT('Ctrl Pts',(97.0013071531924,-1.04625614577938,-9.91159931353711));
#32153=CARTESIAN_POINT('Ctrl Pts',(97.0144949258753,-1.03933869178777,-9.91061166562369));
#32154=CARTESIAN_POINT('Ctrl Pts',(97.0213943273127,-1.03563149317603,-9.91009460965194));
#32155=CARTESIAN_POINT('Ctrl Pts',(97.0397990658844,-1.02550434216245,-9.90871391134123));
#32156=CARTESIAN_POINT('Ctrl Pts',(97.0512347126509,-1.01895959120846,-9.90785454178366));
#32157=CARTESIAN_POINT('Ctrl Pts',(97.0866156254206,-0.997914792268039,
-9.90518802772534));
#32158=CARTESIAN_POINT('Ctrl Pts',(97.1101561097657,-0.982751706818436,
-9.90340288499774));
#32159=CARTESIAN_POINT('Ctrl Pts',(97.2248076452797,-0.902979497191556,
-9.89459247192391));
#32160=CARTESIAN_POINT('Ctrl Pts',(97.3069268645222,-0.826492477722364,
-9.88795467212626));
#32161=CARTESIAN_POINT('Ctrl Pts',(97.3862070410129,-0.728244019838939,
-9.87973277799941));
#32162=CARTESIAN_POINT('Ctrl Pts',(97.3951614703776,-0.716715023836339,
-9.87877121204384));
#32163=CARTESIAN_POINT('Ctrl Pts',(97.4069342223431,-0.700961465935517,
-9.8774570661882));
#32164=CARTESIAN_POINT('Ctrl Pts',(97.4099432926679,-0.696880212795816,
-9.87711659122189));
#32165=CARTESIAN_POINT('Ctrl Pts',(97.4146481318012,-0.690411923224071,
-9.87657672374598));
#32166=CARTESIAN_POINT('Ctrl Pts',(97.4163615572294,-0.688037716119957,
-9.8763785097204));
#32167=CARTESIAN_POINT('Ctrl Pts',(97.4198774149365,-0.683127488093659,
-9.87596840541136));
#32168=CARTESIAN_POINT('Ctrl Pts',(97.4216786600278,-0.680590701696456,
-9.87575643427933));
#32169=CARTESIAN_POINT('Ctrl Pts',(97.4259958715206,-0.674459227935635,
-9.8752439086207));
#32170=CARTESIAN_POINT('Ctrl Pts',(97.4285018271635,-0.670857580754674,
-9.87494269864116));
#32171=CARTESIAN_POINT('Ctrl Pts',(97.4371788796961,-0.658236769065402,
-9.87388691498471));
#32172=CARTESIAN_POINT('Ctrl Pts',(97.4432442978418,-0.649146108972023,
-9.87312593198335));
#32173=CARTESIAN_POINT('Ctrl Pts',(97.457924697957,-0.626466194525916,-9.871228631374));
#32174=CARTESIAN_POINT('Ctrl Pts',(97.4663891999685,-0.612782556946642,
-9.87008501300763));
#32175=CARTESIAN_POINT('Ctrl Pts',(97.5013283491712,-0.553624750344249,
-9.86515846798755));
#32176=CARTESIAN_POINT('Ctrl Pts',(97.5250188312985,-0.506578954432693,
-9.8612870786669));
#32177=CARTESIAN_POINT('Ctrl Pts',(97.5640175224767,-0.414213121392992,
-9.85393150416985));
#32178=CARTESIAN_POINT('Ctrl Pts',(97.5798717704727,-0.369229324892786,
-9.85045156034064));
#32179=CARTESIAN_POINT('Ctrl Pts',(97.6032868372855,-0.287236289973137,
-9.84434327526376));
#32180=CARTESIAN_POINT('Ctrl Pts',(97.611878053243,-0.250589743660362,-9.84169282201664));
#32181=CARTESIAN_POINT('Ctrl Pts',(97.6208371737923,-0.202007991339479,
-9.83828343368103));
#32182=CARTESIAN_POINT('Ctrl Pts',(97.6227994493443,-0.190393062337546,
-9.83747592967094));
#32183=CARTESIAN_POINT('Ctrl Pts',(97.6256590064557,-0.171770275114602,
-9.83619297917899));
#32184=CARTESIAN_POINT('Ctrl Pts',(97.6266680158628,-0.164780647625684,
-9.83571408758776));
#32185=CARTESIAN_POINT('Ctrl Pts',(97.6283480070159,-0.152353561576563,
-9.83486719100818));
#32186=CARTESIAN_POINT('Ctrl Pts',(97.6290440236013,-0.146919758176085,
-9.83449841766919));
#32187=CARTESIAN_POINT('Ctrl Pts',(97.6303123227838,-0.136438350955213,
-9.83378996016001));
#32188=CARTESIAN_POINT('Ctrl Pts',(97.6308899097117,-0.131391524674615,
-9.83345011919794));
#32189=CARTESIAN_POINT('Ctrl Pts',(97.6320625746442,-0.120523033875581,
-9.83272094112819));
#32190=CARTESIAN_POINT('Ctrl Pts',(97.6326469538532,-0.11470033288722,-9.83233194156775));
#32191=CARTESIAN_POINT('Ctrl Pts',(97.6339571437997,-0.100587900798589,
-9.83139296842295));
#32192=CARTESIAN_POINT('Ctrl Pts',(97.6346385516883,-0.0922942865073925,
-9.83084435762351));
#32193=CARTESIAN_POINT('Ctrl Pts',(97.6372463631197,-0.0558210827748878,
-9.82844486236497));
#32194=CARTESIAN_POINT('Ctrl Pts',(97.6382466819176,-0.0275837207897224,
-9.82662194597954));
#32195=CARTESIAN_POINT('Ctrl Pts',(97.638230762545,0.00066374236820414,
-9.82482230235678));
#32196=CARTESIAN_POINT('Origin',(96.460480949577,-8.32667268468867E-16,
1.18130019239114E-14));
#32197=CARTESIAN_POINT('',(97.9254959686812,0.00102976170736319,-0.160655045842894));
#32198=CARTESIAN_POINT('',(97.9240238517789,0.00148269405508262,-0.0893449541570721));
#32199=CARTESIAN_POINT('',(97.923980949577,-1.01189432752408E-15,1.19922289829666E-14));
#32200=CARTESIAN_POINT('',(95.825530156632,1.3210310846968,-3.74994559417826E-5));
#32201=CARTESIAN_POINT('Ctrl Pts',(97.9254959686812,0.00102976170736319,
-0.160655045842894));
#32202=CARTESIAN_POINT('Ctrl Pts',(97.9259403980951,0.0599082620416902,
-0.157443865218363));
#32203=CARTESIAN_POINT('Ctrl Pts',(97.8960926319347,0.60114388017442,-0.127899405977983));
#32204=CARTESIAN_POINT('Ctrl Pts',(97.2508483847669,1.50956313647968,-0.0743602238489917));
#32205=CARTESIAN_POINT('Ctrl Pts',(96.2230516351132,1.50901544022077,-0.0240322223445412));
#32206=CARTESIAN_POINT('Ctrl Pts',(95.825530156632,1.3210310846968,-3.74994559417826E-5));
#32207=CARTESIAN_POINT('',(97.0944880441522,1.31904027763685,1.17291095544168E-14));
#32208=CARTESIAN_POINT('Origin',(96.460480949577,-8.32667268468867E-16,
1.18130019239114E-14));
#32209=CARTESIAN_POINT('Ctrl Pts',(97.0944880441522,1.31904027763685,1.12063136548102E-14));
#32210=CARTESIAN_POINT('Ctrl Pts',(97.53097659376,1.10923861968598,-0.0263332786158426));
#32211=CARTESIAN_POINT('Ctrl Pts',(97.8934559885557,0.609749393684391,-0.0561149300015368));
#32212=CARTESIAN_POINT('Ctrl Pts',(97.9256366870345,0.0646804841820412,
-0.0858965813872315));
#32213=CARTESIAN_POINT('Ctrl Pts',(97.9251323125163,0.00148381702055458,
-0.0893449541570721));
#32214=CARTESIAN_POINT('Origin',(96.460480949577,-8.32667268468867E-16,
1.18130019239114E-14));
#32215=CARTESIAN_POINT('',(97.9237766744537,0.000379231245023859,-0.660655020925316));
#32216=CARTESIAN_POINT('',(97.9239809152273,0.0003170831650837,-0.589344954125679));
#32217=CARTESIAN_POINT('',(97.923980949577,-1.01189432752408E-15,1.19922289829666E-14));
#32218=CARTESIAN_POINT('Ctrl Pts',(97.9217394295534,0.000383291797303924,
-0.660654772361549));
#32219=CARTESIAN_POINT('Ctrl Pts',(97.9222492769024,0.219624290680771,-0.648776687925926));
#32220=CARTESIAN_POINT('Ctrl Pts',(97.7733939631201,0.924254639301895,-0.610565324874444));
#32221=CARTESIAN_POINT('Ctrl Pts',(96.6848024105838,1.71234718119464,-0.546020683207117));
#32222=CARTESIAN_POINT('Ctrl Pts',(95.1488986503746,1.12351576042364,-0.467020847359552));
#32223=CARTESIAN_POINT('Ctrl Pts',(94.8028899975499,-0.484641598927434,
-0.38802101151199));
#32224=CARTESIAN_POINT('Ctrl Pts',(95.9606267756977,-1.65300325887114,-0.309021175664427));
#32225=CARTESIAN_POINT('Ctrl Pts',(97.506407164997,-1.33544801236195,-0.233232520441395));
#32226=CARTESIAN_POINT('Ctrl Pts',(97.9222958558073,-0.42292473151319,-0.183777143834217));
#32227=CARTESIAN_POINT('Ctrl Pts',(97.9254959686812,0.00102976170736319,
-0.160655045842894));
#32228=CARTESIAN_POINT('Ctrl Pts',(97.9239801985517,0.00148264983063222,
-0.0893449541570721));
#32229=CARTESIAN_POINT('Ctrl Pts',(97.9240347313566,-0.052345784526501,
-0.0922844814261104));
#32230=CARTESIAN_POINT('Ctrl Pts',(97.9211153199247,-0.106304899557918,
-0.0952240086951486));
#32231=CARTESIAN_POINT('Ctrl Pts',(97.9152052727089,-0.160029352584068,
-0.0981635359641869));
#32232=CARTESIAN_POINT('Ctrl Pts',(97.9093025720355,-0.213687022899094,
-0.101099409224866));
#32233=CARTESIAN_POINT('Ctrl Pts',(97.9004166445377,-0.267110062615521,
-0.104035282485545));
#32234=CARTESIAN_POINT('Ctrl Pts',(97.8885827988832,-0.319933364950077,
-0.106971155746224));
#32235=CARTESIAN_POINT('Ctrl Pts',(97.8767585287381,-0.372713924625424,
-0.109904653407031));
#32236=CARTESIAN_POINT('Ctrl Pts',(97.8619911791886,-0.424895168884155,
-0.112838151067839));
#32237=CARTESIAN_POINT('Ctrl Pts',(97.8443675010344,-0.476120008711344,
-0.115771648728646));
#32238=CARTESIAN_POINT('Ctrl Pts',(97.8267504432777,-0.527325605744948,
-0.118704044410605));
#32239=CARTESIAN_POINT('Ctrl Pts',(97.8062793621778,-0.57757498729588,-0.121636440092565));
#32240=CARTESIAN_POINT('Ctrl Pts',(97.7830907012564,-0.626526691181278,
-0.124568835774524));
#32241=CARTESIAN_POINT('Ctrl Pts',(97.7598840200597,-0.675516436210291,
-0.127503510267565));
#32242=CARTESIAN_POINT('Ctrl Pts',(97.7339557736685,-0.723205985975424,
-0.130438184760606));
#32243=CARTESIAN_POINT('Ctrl Pts',(97.7054896108962,-0.769276077387165,
-0.133372859253647));
#32244=CARTESIAN_POINT('Ctrl Pts',(97.677013067021,-0.815362969741224,-0.13630860397024));
#32245=CARTESIAN_POINT('Ctrl Pts',(97.6459970808003,-0.859828773056688,
-0.139244348686834));
#32246=CARTESIAN_POINT('Ctrl Pts',(97.6126681478676,-0.902384014760494,
-0.142180093403427));
#32247=CARTESIAN_POINT('Ctrl Pts',(97.5792764156735,-0.945019440181892,
-0.145121369728251));
#32248=CARTESIAN_POINT('Ctrl Pts',(97.5435634017889,-0.985736700446781,
-0.148062646053075));
#32249=CARTESIAN_POINT('Ctrl Pts',(97.5057943185634,-1.02428131419951,-0.151003922377899));
#32250=CARTESIAN_POINT('Ctrl Pts',(97.4758500575231,-1.0548404349761,-0.15333583881697));
#32251=CARTESIAN_POINT('Ctrl Pts',(97.444614229094,-1.08403456024074,-0.155667755256041));
#32252=CARTESIAN_POINT('Ctrl Pts',(97.4122330415994,-1.11175546112038,-0.157999671695112));
#32253=CARTESIAN_POINT('Ctrl Pts',(97.3703895406663,-1.14757686334716,-0.161013012317983));
#32254=CARTESIAN_POINT('Ctrl Pts',(97.3264338721171,-1.18110717537137,-0.164026352940854));
#32255=CARTESIAN_POINT('Ctrl Pts',(97.2806465605239,-1.21208936164794,-0.167039693563725));
#32256=CARTESIAN_POINT('Ctrl Pts',(97.2349409306402,-1.24301627763567,-0.170047658574781));
#32257=CARTESIAN_POINT('Ctrl Pts',(97.1874105755345,-1.27140379677066,-0.173055623585837));
#32258=CARTESIAN_POINT('Ctrl Pts',(97.1383689528339,-1.29703512097412,-0.176063588596893));
#32259=CARTESIAN_POINT('Ctrl Pts',(97.0893760987136,-1.32264095655748,-0.179068562389984));
#32260=CARTESIAN_POINT('Ctrl Pts',(97.0388754189467,-1.34549578440673,-0.182073536183075));
#32261=CARTESIAN_POINT('Ctrl Pts',(96.9872076383996,-1.36542712924639,-0.185078509976165));
#32262=CARTESIAN_POINT('Ctrl Pts',(96.9355709566339,-1.38534647743104,-0.188081675078766));
#32263=CARTESIAN_POINT('Ctrl Pts',(96.882769057068,-1.40234564142863,-0.191084840181366));
#32264=CARTESIAN_POINT('Ctrl Pts',(96.829163356026,-1.41629994463567,-0.194088005283967));
#32265=CARTESIAN_POINT('Ctrl Pts',(96.7755688796258,-1.43025132591364,-0.197090541545751));
#32266=CARTESIAN_POINT('Ctrl Pts',(96.7211714455109,-1.44115897994903,-0.200093077807535));
#32267=CARTESIAN_POINT('Ctrl Pts',(96.6663461461169,-1.44894850524564,-0.203095614069319));
#32268=CARTESIAN_POINT('Ctrl Pts',(96.6114718367766,-1.45674499382784,-0.206100834386511));
#32269=CARTESIAN_POINT('Ctrl Pts',(96.5561694206087,-1.46141771019846,-0.209106054703702));
#32270=CARTESIAN_POINT('Ctrl Pts',(96.5008211789853,-1.46294392096597,-0.212111275020894));
#32271=CARTESIAN_POINT('Ctrl Pts',(96.445448437896,-1.46447080729872,-0.215117825575331));
#32272=CARTESIAN_POINT('Ctrl Pts',(96.3900303584181,-1.46284842623924,-0.218124376129769));
#32273=CARTESIAN_POINT('Ctrl Pts',(96.3349480076539,-1.45810621372112,-0.221130926684206));
#32274=CARTESIAN_POINT('Ctrl Pts',(96.2797635962515,-1.45335521448221,-0.224143047997052));
#32275=CARTESIAN_POINT('Ctrl Pts',(96.2249166790471,-1.4454729104902,-0.227155169309899));
#32276=CARTESIAN_POINT('Ctrl Pts',(96.1707808295434,-1.4345403760273,-0.230167290622745));
#32277=CARTESIAN_POINT('Ctrl Pts',(96.1298497792372,-1.42627450189439,-0.232444696262722));
#32278=CARTESIAN_POINT('Ctrl Pts',(96.0893250666734,-1.41626602279057,-0.234722101902699));
#32279=CARTESIAN_POINT('Ctrl Pts',(96.049361832311,-1.40456873146829,-0.236999507542675));
#32280=CARTESIAN_POINT('Ctrl Pts',(95.9964555305478,-1.38908298727408,-0.240014506502302));
#32281=CARTESIAN_POINT('Ctrl Pts',(95.9443183765915,-1.37057251816803,-0.243029505461928));
#32282=CARTESIAN_POINT('Ctrl Pts',(95.8933191205839,-1.34913294738997,-0.246044504421554));
#32283=CARTESIAN_POINT('Ctrl Pts',(95.8424077195759,-1.32773030996411,-0.249054309526341));
#32284=CARTESIAN_POINT('Ctrl Pts',(95.7926308073448,-1.3034087877203,-0.252064114631127));
#32285=CARTESIAN_POINT('Ctrl Pts',(95.744341288851,-1.27631353371154,-0.255073919735913));
#32286=CARTESIAN_POINT('Ctrl Pts',(95.6960979979698,-1.24924421802115,-0.258080843550752));
#32287=CARTESIAN_POINT('Ctrl Pts',(95.6493397364313,-1.21940668764572,-0.26108776736559));
#32288=CARTESIAN_POINT('Ctrl Pts',(95.6043970392579,-1.18699308696079,-0.264094691180428));
#32289=CARTESIAN_POINT('Ctrl Pts',(95.5594797858355,-1.15459783683422,-0.267099912662611));
#32290=CARTESIAN_POINT('Ctrl Pts',(95.5163764850673,-1.11962971469893,-0.270105134144794));
#32291=CARTESIAN_POINT('Ctrl Pts',(95.4753888178461,-1.0823242314583,-0.273110355626977));
#32292=CARTESIAN_POINT('Ctrl Pts',(95.4344083235427,-1.04502527674649,-0.276115051189821));
#32293=CARTESIAN_POINT('Ctrl Pts',(95.3955431160815,-1.00539012750951,-0.279119746752666));
#32294=CARTESIAN_POINT('Ctrl Pts',(95.3590601363147,-0.963693126525499,
-0.28212444231551));
#32295=CARTESIAN_POINT('Ctrl Pts',(95.3225428291779,-0.921956892222702,
-0.285131965040406));
#32296=CARTESIAN_POINT('Ctrl Pts',(95.2884125745901,-0.878155327439156,
-0.288139487765303));
#32297=CARTESIAN_POINT('Ctrl Pts',(95.2568968923074,-0.832596941554766,
-0.291147010490199));
#32298=CARTESIAN_POINT('Ctrl Pts',(95.2253664007609,-0.787017147720452,
-0.294155946454275));
#32299=CARTESIAN_POINT('Ctrl Pts',(95.1964532052038,-0.739679336939152,
-0.297164882418351));
#32300=CARTESIAN_POINT('Ctrl Pts',(95.1703404015189,-0.690919399247418,
-0.300173818382427));
#32301=CARTESIAN_POINT('Ctrl Pts',(95.1441783218411,-0.642067449438771,
-0.30318843233915));
#32302=CARTESIAN_POINT('Ctrl Pts',(95.1208274126701,-0.591788490069951,
-0.306203046295873));
#32303=CARTESIAN_POINT('Ctrl Pts',(95.1004233833001,-0.540440252398773,
-0.309217660252597));
#32304=CARTESIAN_POINT('Ctrl Pts',(95.085123064707,-0.50193587753671,-0.311478221298477));
#32305=CARTESIAN_POINT('Ctrl Pts',(95.0714787848521,-0.462830705618857,
-0.313738782344358));
#32306=CARTESIAN_POINT('Ctrl Pts',(95.0595291290122,-0.423280340266479,
-0.315999343390238));
#32307=CARTESIAN_POINT('Ctrl Pts',(95.0436353007261,-0.370675752821941,
-0.319006038275412));
#32308=CARTESIAN_POINT('Ctrl Pts',(95.0306743464371,-0.317061713014208,
-0.322012733160585));
#32309=CARTESIAN_POINT('Ctrl Pts',(95.0207691273365,-0.262796725438043,
-0.325019428045759));
#32310=CARTESIAN_POINT('Ctrl Pts',(95.0108817741184,-0.208629614736458,
-0.328020699804321));
#32311=CARTESIAN_POINT('Ctrl Pts',(95.0040393134213,-0.153814402670927,
-0.331021971562884));
#32312=CARTESIAN_POINT('Ctrl Pts',(95.0003145610086,-0.0987236936862529,
-0.334023243321446));
#32313=CARTESIAN_POINT('Ctrl Pts',(94.9965935503585,-0.0436883269982326,
-0.337021500102074));
#32314=CARTESIAN_POINT('Ctrl Pts',(94.9959840799632,0.0116214628037488,
-0.340019756882702));
#32315=CARTESIAN_POINT('Ctrl Pts',(94.9985074346293,0.0668258302716808,
-0.343018013663329));
#32316=CARTESIAN_POINT('Ctrl Pts',(95.001029257557,0.121996687328589,-0.346014450428228));
#32317=CARTESIAN_POINT('Ctrl Pts',(95.0066801125293,0.177061721004989,-0.349010887193128));
#32318=CARTESIAN_POINT('Ctrl Pts',(95.0154292000922,0.231641298802641,-0.352007323958027));
#32319=CARTESIAN_POINT('Ctrl Pts',(95.0241764546891,0.286209441977913,-0.355003132958398));
#32320=CARTESIAN_POINT('Ctrl Pts',(95.0360205692775,0.340291808672809,-0.357998941958769));
#32321=CARTESIAN_POINT('Ctrl Pts',(95.0508792097159,0.393516435464501,-0.36099475095914));
#32322=CARTESIAN_POINT('Ctrl Pts',(95.0657514420968,0.446789749487463,-0.363993300376015));
#32323=CARTESIAN_POINT('Ctrl Pts',(95.0836435670714,0.499203244850938,-0.366991849792889));
#32324=CARTESIAN_POINT('Ctrl Pts',(95.1044230501465,0.550399149156465,-0.369990399209764));
#32325=CARTESIAN_POINT('Ctrl Pts',(95.125211897677,0.601618125343098,-0.372990299949104));
#32326=CARTESIAN_POINT('Ctrl Pts',(95.14889047002,0.651617937283341,-0.375990200688444));
#32327=CARTESIAN_POINT('Ctrl Pts',(95.175278973966,0.700062948516415,-0.378990101427784));
#32328=CARTESIAN_POINT('Ctrl Pts',(95.2017175231805,0.748599834741826,-0.381995691418719));
#32329=CARTESIAN_POINT('Ctrl Pts',(95.2308759905254,0.795575578942978,-0.385001281409655));
#32330=CARTESIAN_POINT('Ctrl Pts',(95.2625303434212,0.840682220111097,-0.38800687140059));
#32331=CARTESIAN_POINT('Ctrl Pts',(95.2870776015305,0.875661433454824,-0.39033764067966));
#32332=CARTESIAN_POINT('Ctrl Pts',(95.3131248754419,0.909517177915923,-0.392668409958731));
#32333=CARTESIAN_POINT('Ctrl Pts',(95.3405517846923,0.942120435847087,-0.394999179237801));
#32334=CARTESIAN_POINT('Ctrl Pts',(95.3759806229821,0.98423584675321,-0.398009961354197));
#32335=CARTESIAN_POINT('Ctrl Pts',(95.413862643576,1.02443824365443,-0.401020743470594));
#32336=CARTESIAN_POINT('Ctrl Pts',(95.4539634038702,1.06242867063366,-0.40403152558699));
#32337=CARTESIAN_POINT('Ctrl Pts',(95.4939929335618,1.10035161557538,-0.407036959679479));
#32338=CARTESIAN_POINT('Ctrl Pts',(95.5362330015292,1.13607002794812,-0.410042393771969));
#32339=CARTESIAN_POINT('Ctrl Pts',(95.5804100992899,1.16931926712725,-0.413047827864458));
#32340=CARTESIAN_POINT('Ctrl Pts',(95.6245435093959,1.20253562543929,-0.416050289820401));
#32341=CARTESIAN_POINT('Ctrl Pts',(95.6706097348918,1.23328733190982,-0.419052751776343));
#32342=CARTESIAN_POINT('Ctrl Pts',(95.7183011377446,1.26134903056547,-0.422055213732285));
#32343=CARTESIAN_POINT('Ctrl Pts',(95.7659641912214,1.28939404840236,-0.425055890923721));
#32344=CARTESIAN_POINT('Ctrl Pts',(95.815250053192,1.31475196071634,-0.428056568115158));
#32345=CARTESIAN_POINT('Ctrl Pts',(95.8658228891346,1.33724120529953,-0.431057245306594));
#32346=CARTESIAN_POINT('Ctrl Pts',(95.9163856120044,1.3597259526983,-0.434057322451254));
#32347=CARTESIAN_POINT('Ctrl Pts',(95.9682343157003,1.37934295726238,-0.437057399595914));
#32348=CARTESIAN_POINT('Ctrl Pts',(96.0210115009846,1.39595804154492,-0.440057476740574));
#32349=CARTESIAN_POINT('Ctrl Pts',(96.0738370533894,1.41258835255428,-0.443060303275749));
#32350=CARTESIAN_POINT('Ctrl Pts',(96.1275922828073,1.42621108810601,-0.446063129810924));
#32351=CARTESIAN_POINT('Ctrl Pts',(96.1819042023455,1.43674188562243,-0.449065956346099));
#32352=CARTESIAN_POINT('Ctrl Pts',(96.236240774168,1.44727746308802,-0.45207014586999));
#32353=CARTESIAN_POINT('Ctrl Pts',(96.2911340158551,1.45471823372441,-0.455074335393881));
#32354=CARTESIAN_POINT('Ctrl Pts',(96.3462036908734,1.45903151375945,-0.458078524917772));
#32355=CARTESIAN_POINT('Ctrl Pts',(96.4013770235376,1.46335291268123,-0.461088369227421));
#32356=CARTESIAN_POINT('Ctrl Pts',(96.4567269239329,1.46453504965939,-0.46409821353707));
#32357=CARTESIAN_POINT('Ctrl Pts',(96.511872186207,1.46259741241315,-0.467108057846719));
#32358=CARTESIAN_POINT('Ctrl Pts',(96.5539567156322,1.46111868970258,-0.469405043592934));
#32359=CARTESIAN_POINT('Ctrl Pts',(96.5959220275134,1.45782406683853,-0.471702029339148));
#32360=CARTESIAN_POINT('Ctrl Pts',(96.6376020196412,1.45274236413044,-0.473999015085362));
#32361=CARTESIAN_POINT('Ctrl Pts',(96.692231930419,1.44608178308497,-0.477009671277152));
#32362=CARTESIAN_POINT('Ctrl Pts',(96.7465999137415,1.43632147318516,-0.480020327468943));
#32363=CARTESIAN_POINT('Ctrl Pts',(96.8003275092147,1.42349449099827,-0.483030983660733));
#32364=CARTESIAN_POINT('Ctrl Pts',(96.8539599582826,1.41069022416342,-0.486036308269905));
#32365=CARTESIAN_POINT('Ctrl Pts',(96.9069537607428,1.39483018417317,-0.489041632879076));
#32366=CARTESIAN_POINT('Ctrl Pts',(96.9589378579191,1.37599889553953,-0.492046957488248));
#32367=CARTESIAN_POINT('Ctrl Pts',(97.0108707209289,1.35718616653143,-0.495049320128088));
#32368=CARTESIAN_POINT('Ctrl Pts',(97.0617953560977,1.33540816888856,-0.498051682767928));
#32369=CARTESIAN_POINT('Ctrl Pts',(97.1113549683908,1.31079947422679,-0.501054045407768));
#32370=CARTESIAN_POINT('Ctrl Pts',(97.1608852907622,1.28620532339832,-0.504054633639725));
#32371=CARTESIAN_POINT('Ctrl Pts',(97.2090517174039,1.25878402582337,-0.507055221871683));
#32372=CARTESIAN_POINT('Ctrl Pts',(97.255518735269,1.22871769309386,-0.510055810103641));
#32373=CARTESIAN_POINT('Ctrl Pts',(97.3019766243376,1.19865726712249,-0.513055808847379));
#32374=CARTESIAN_POINT('Ctrl Pts',(97.3467353247295,1.16595312463451,-0.516055807591117));
#32375=CARTESIAN_POINT('Ctrl Pts',(97.3894871816032,1.13083140691108,-0.519055806334855));
#32376=CARTESIAN_POINT('Ctrl Pts',(97.4322784630212,1.09567730094023,-0.522058571591961));
#32377=CARTESIAN_POINT('Ctrl Pts',(97.4730587948287,1.05810150152605,-0.525061336849067));
#32378=CARTESIAN_POINT('Ctrl Pts',(97.5115537886237,1.01837033392487,-0.528064102106173));
#32379=CARTESIAN_POINT('Ctrl Pts',(97.5500663765137,0.97862100723683,-0.531068239773867));
#32380=CARTESIAN_POINT('Ctrl Pts',(97.5862911984259,0.936714748696337,-0.534072377441562));
#32381=CARTESIAN_POINT('Ctrl Pts',(97.6199931960324,0.892952182549568,-0.537076515109257));
#32382=CARTESIAN_POINT('Ctrl Pts',(97.6537588140523,0.849107004310048,-0.540086323790365));
#32383=CARTESIAN_POINT('Ctrl Pts',(97.6849917955423,0.803398955181929,-0.543096132471473));
#32384=CARTESIAN_POINT('Ctrl Pts',(97.7135002540531,0.756157968026738,-0.546105941152582));
#32385=CARTESIAN_POINT('Ctrl Pts',(97.7352631248655,0.720095004463755,-0.54840357774603));
#32386=CARTESIAN_POINT('Ctrl Pts',(97.7554391613811,0.683139338022428,-0.550701214339477));
#32387=CARTESIAN_POINT('Ctrl Pts',(97.7739617263499,0.645445969115977,-0.552998850932925));
#32388=CARTESIAN_POINT('Ctrl Pts',(97.7999214270754,0.592618049343745,-0.556219029047693));
#32389=CARTESIAN_POINT('Ctrl Pts',(97.8227287513135,0.538143597802004,-0.55943920716246));
#32390=CARTESIAN_POINT('Ctrl Pts',(97.8421887872528,0.482406158029926,-0.562659385277227));
#32391=CARTESIAN_POINT('Ctrl Pts',(97.8616014987721,0.426804264873654,-0.565871732313862));
#32392=CARTESIAN_POINT('Ctrl Pts',(97.8776829711369,0.369945875263667,-0.569084079350498));
#32393=CARTESIAN_POINT('Ctrl Pts',(97.8902854901268,0.312235849676686,-0.572296426387133));
#32394=CARTESIAN_POINT('Ctrl Pts',(97.9028432269035,0.254730892827498,-0.575497358562217));
#32395=CARTESIAN_POINT('Ctrl Pts',(97.9119465324078,0.196380723927314,-0.578698290737302));
#32396=CARTESIAN_POINT('Ctrl Pts',(97.917497523185,0.137604339435666,-0.581899222912386));
#32397=CARTESIAN_POINT('Ctrl Pts',(97.9218016011884,0.0920308276505253,
-0.584381133316817));
#32398=CARTESIAN_POINT('Ctrl Pts',(97.9239709738696,0.046201501282702,-0.586863043721248));
#32399=CARTESIAN_POINT('Ctrl Pts',(97.9239809152272,0.000317083165083229,
-0.589344954125678));
#32400=CARTESIAN_POINT('Origin',(96.460480949577,-8.32667268468867E-16,
1.18130019239114E-14));
#32401=CARTESIAN_POINT('',(97.923980378536,-0.00129284060398358,-1.16065504579921));
#32402=CARTESIAN_POINT('',(97.9239803891082,-0.00128081692310598,-1.08934495412119));
#32403=CARTESIAN_POINT('',(97.923980949577,-1.01189432752408E-15,1.19922289829666E-14));
#32404=CARTESIAN_POINT('Ctrl Pts',(97.923980378536,-0.00129284060398456,
-1.16065504579921));
#32405=CARTESIAN_POINT('Ctrl Pts',(97.9240284830895,0.0531616577923571,
-1.15769184059285));
#32406=CARTESIAN_POINT('Ctrl Pts',(97.9210330828335,0.10770563227362,-1.1547286353865));
#32407=CARTESIAN_POINT('Ctrl Pts',(97.9149908304708,0.161966837291652,-1.15176543018014));
#32408=CARTESIAN_POINT('Ctrl Pts',(97.9089535018915,0.216183825285511,-1.14880463966613));
#32409=CARTESIAN_POINT('Ctrl Pts',(97.8998742957547,0.270117961430168,-1.14584384915211));
#32410=CARTESIAN_POINT('Ctrl Pts',(97.8878018665388,0.323399520722398,-1.1428830586381));
#32411=CARTESIAN_POINT('Ctrl Pts',(97.875734196129,0.376660077065522,-1.13992343523206));
#32412=CARTESIAN_POINT('Ctrl Pts',(97.8606757609156,0.429268036549174,-1.13696381182601));
#32413=CARTESIAN_POINT('Ctrl Pts',(97.842726312339,0.480863813488882,-1.13400418841997));
#32414=CARTESIAN_POINT('Ctrl Pts',(97.8247633560666,0.532498418365578,-1.131042337776));
#32415=CARTESIAN_POINT('Ctrl Pts',(97.80390521258,0.58311880194702,-1.12808048713203));
#32416=CARTESIAN_POINT('Ctrl Pts',(97.7803010259489,0.632382175591351,-1.12511863648806));
#32417=CARTESIAN_POINT('Ctrl Pts',(97.756689115767,0.681661668756108,-1.12215581669382));
#32418=CARTESIAN_POINT('Ctrl Pts',(97.7303296319005,0.729582788236327,-1.11919299689958));
#32419=CARTESIAN_POINT('Ctrl Pts',(97.7014176884102,0.775827468071288,-1.11623017710534));
#32420=CARTESIAN_POINT('Ctrl Pts',(97.6724504556885,0.822160583082206,-1.11326169141633));
#32421=CARTESIAN_POINT('Ctrl Pts',(97.6409213252783,0.866810407157974,-1.11029320572732));
#32422=CARTESIAN_POINT('Ctrl Pts',(97.6070680237593,0.909489049586677,-1.1073247200383));
#32423=CARTESIAN_POINT('Ctrl Pts',(97.5754965996013,0.949290943704698,-1.10455632473889));
#32424=CARTESIAN_POINT('Ctrl Pts',(97.541904427265,0.987378510028894,-1.10178792943947));
#32425=CARTESIAN_POINT('Ctrl Pts',(97.5065125074113,1.02354786405657,-1.09901953414006));
#32426=CARTESIAN_POINT('Ctrl Pts',(97.4680301976465,1.0628754928328,-1.09600940510767));
#32427=CARTESIAN_POINT('Ctrl Pts',(97.4272460484989,1.10011250778398,-1.09299927607529));
#32428=CARTESIAN_POINT('Ctrl Pts',(97.384416116279,1.13497843932444,-1.08998914704291));
#32429=CARTESIAN_POINT('Ctrl Pts',(97.3416623051393,1.16978240409934,-1.08698436787361));
#32430=CARTESIAN_POINT('Ctrl Pts',(97.2968703327355,1.2022233176518,-1.08397958870431));
#32431=CARTESIAN_POINT('Ctrl Pts',(97.2503326451425,1.23205785132527,-1.08097480953501));
#32432=CARTESIAN_POINT('Ctrl Pts',(97.2038409990339,1.2618628685727,-1.07797300310674));
#32433=CARTESIAN_POINT('Ctrl Pts',(97.1556075014537,1.28906633038001,-1.07497119667846));
#32434=CARTESIAN_POINT('Ctrl Pts',(97.1059556912606,1.31346663750871,-1.07196939025018));
#32435=CARTESIAN_POINT('Ctrl Pts',(97.0563333922172,1.33785244202183,-1.0689693679816));
#32436=CARTESIAN_POINT('Ctrl Pts',(97.0052949244536,1.35943816169359,-1.06596934571303));
#32437=CARTESIAN_POINT('Ctrl Pts',(96.9531886625336,1.37806798075895,-1.06296932344445));
#32438=CARTESIAN_POINT('Ctrl Pts',(96.9010927911103,1.39669408485678,-1.05996989940956));
#32439=CARTESIAN_POINT('Ctrl Pts',(96.8479300454059,1.41236528124363,-1.05697047537467));
#32440=CARTESIAN_POINT('Ctrl Pts',(96.7940668498442,1.42497463035062,-1.05397105133977));
#32441=CARTESIAN_POINT('Ctrl Pts',(96.7401541352334,1.43759557184408,-1.05096886978883));
#32442=CARTESIAN_POINT('Ctrl Pts',(96.6855401995404,1.44714892160775,-1.04796668823788));
#32443=CARTESIAN_POINT('Ctrl Pts',(96.6306031734235,1.45357857680743,-1.04496450668694));
#32444=CARTESIAN_POINT('Ctrl Pts',(96.575641141385,1.46001115862082,-1.04196095862015));
#32445=CARTESIAN_POINT('Ctrl Pts',(96.5203562538571,1.46331717997922,-1.03895741055337));
#32446=CARTESIAN_POINT('Ctrl Pts',(96.4651299873959,1.46349261578163,-1.03595386248658));
#32447=CARTESIAN_POINT('Ctrl Pts',(96.4097994910381,1.46366838268837,-1.03294464574935));
#32448=CARTESIAN_POINT('Ctrl Pts',(96.3545283654123,1.46070178940425,-1.02993542901212));
#32449=CARTESIAN_POINT('Ctrl Pts',(96.2996951330034,1.45464090798684,-1.0269262122749));
#32450=CARTESIAN_POINT('Ctrl Pts',(96.2577455140603,1.45000409095543,-1.02462404094743));
#32451=CARTESIAN_POINT('Ctrl Pts',(96.2160521425861,1.44355731388188,-1.02232186961996));
#32452=CARTESIAN_POINT('Ctrl Pts',(96.1747796245323,1.43534212049522,-1.02001969829249));
#32453=CARTESIAN_POINT('Ctrl Pts',(96.1208150390998,1.42460060225827,-1.01700956643865));
#32454=CARTESIAN_POINT('Ctrl Pts',(96.0673436858459,1.41078892254573,-1.01399943458481));
#32455=CARTESIAN_POINT('Ctrl Pts',(96.014740374309,1.39396828857753,-1.01098930273097));
#32456=CARTESIAN_POINT('Ctrl Pts',(95.9622305532285,1.37717754947145,-1.00798452070383));
#32457=CARTESIAN_POINT('Ctrl Pts',(95.9105862112277,1.35738862827198,-1.0049797386767));
#32458=CARTESIAN_POINT('Ctrl Pts',(95.8601709344612,1.33471350324768,-1.00197495664956));
#32459=CARTESIAN_POINT('Ctrl Pts',(95.8098055350403,1.31206081140475,-0.998973147343418));
#32460=CARTESIAN_POINT('Ctrl Pts',(95.7606672713862,1.28652778772483,-0.995971338037275));
#32461=CARTESIAN_POINT('Ctrl Pts',(95.7131017690514,1.2582752522866,-0.992969528731132));
#32462=CARTESIAN_POINT('Ctrl Pts',(95.6655645375839,1.23003950892752,-0.989969503569977));
#32463=CARTESIAN_POINT('Ctrl Pts',(95.6195986677897,1.19908772670014,-0.986969478408821));
#32464=CARTESIAN_POINT('Ctrl Pts',(95.575525010414,1.16562654213948,-0.983969453247666));
#32465=CARTESIAN_POINT('Ctrl Pts',(95.5314601416081,1.13217202995358,-0.980970026310765));
#32466=CARTESIAN_POINT('Ctrl Pts',(95.4892871562698,1.09620942835326,-0.977970599373865));
#32467=CARTESIAN_POINT('Ctrl Pts',(95.4492958323556,1.0579871968554,-0.974971172436964));
#32468=CARTESIAN_POINT('Ctrl Pts',(95.4092677426307,1.01972982595246,-0.971968987992874));
#32469=CARTESIAN_POINT('Ctrl Pts',(95.3714257040584,0.979209040496911,-0.968966803548784));
#32470=CARTESIAN_POINT('Ctrl Pts',(95.336023313683,0.936710881264692,-0.965964619104694));
#32471=CARTESIAN_POINT('Ctrl Pts',(95.300604809071,0.894193377988669,-0.962961068145243));
#32472=CARTESIAN_POINT('Ctrl Pts',(95.2676284812852,0.849697131787614,-0.959957517185793));
#32473=CARTESIAN_POINT('Ctrl Pts',(95.2373061390484,0.803539440779607,-0.956953966226342));
#32474=CARTESIAN_POINT('Ctrl Pts',(95.2069265691368,0.757294635876738,-0.95394474663363));
#32475=CARTESIAN_POINT('Ctrl Pts',(95.179211255907,0.709382580456583,-0.950935527040919));
#32476=CARTESIAN_POINT('Ctrl Pts',(95.1543267612167,0.660146564202886,-0.947926307448207));
#32477=CARTESIAN_POINT('Ctrl Pts',(95.1352893343227,0.622479451743986,-0.945624159113781));
#32478=CARTESIAN_POINT('Ctrl Pts',(95.1179077774405,0.584038014560071,-0.943322010779356));
#32479=CARTESIAN_POINT('Ctrl Pts',(95.1022372350482,0.544982808850793,-0.94101986244493));
#32480=CARTESIAN_POINT('Ctrl Pts',(95.0817475827641,0.49391708535329,-0.938009742074009));
#32481=CARTESIAN_POINT('Ctrl Pts',(95.0640987500391,0.441586937083567,-0.934999621703088));
#32482=CARTESIAN_POINT('Ctrl Pts',(95.0494442690851,0.388339717652553,-0.931989501332166));
#32483=CARTESIAN_POINT('Ctrl Pts',(95.0348158332484,0.335187133444637,-0.928984730788258));
#32484=CARTESIAN_POINT('Ctrl Pts',(95.0231713270365,0.281121217675837,-0.925979960244349));
#32485=CARTESIAN_POINT('Ctrl Pts',(95.014615628215,0.226507665395155,-0.92297518970044));
#32486=CARTESIAN_POINT('Ctrl Pts',(95.0060683938113,0.171948143993042,-0.919973391869084));
#32487=CARTESIAN_POINT('Ctrl Pts',(95.0006039946378,0.116842578536681,-0.916971594037727));
#32488=CARTESIAN_POINT('Ctrl Pts',(94.9982765885658,0.0615683087298558,
-0.91396979620637));
#32489=CARTESIAN_POINT('Ctrl Pts',(94.995950565786,0.00632689114651344,
-0.910969782491449));
#32490=CARTESIAN_POINT('Ctrl Pts',(94.9967578627805,-0.049082505448643,
-0.907969768776527));
#32491=CARTESIAN_POINT('Ctrl Pts',(95.0007007280563,-0.104278256874737,
-0.904969755061606));
#32492=CARTESIAN_POINT('Ctrl Pts',(95.0046428071603,-0.159463002767406,
-0.901970339522275));
#32493=CARTESIAN_POINT('Ctrl Pts',(95.0117191753086,-0.214433661608961,
-0.898970923982944));
#32494=CARTESIAN_POINT('Ctrl Pts',(95.0218800750811,-0.268811781549082,
-0.895971508443614));
#32495=CARTESIAN_POINT('Ctrl Pts',(95.0320503168185,-0.323239896912986,
-0.89296933523169));
#32496=CARTESIAN_POINT('Ctrl Pts',(95.0453106587844,-0.377073864721718,
-0.889967162019767));
#32497=CARTESIAN_POINT('Ctrl Pts',(95.0615600991256,-0.429945001334288,
-0.886964988807844));
#32498=CARTESIAN_POINT('Ctrl Pts',(95.0778169362157,-0.482840204900062,
-0.883961449006003));
#32499=CARTESIAN_POINT('Ctrl Pts',(95.0970654001508,-0.534771207526567,
-0.880957909204163));
#32500=CARTESIAN_POINT('Ctrl Pts',(95.1191554772583,-0.585387245598138,
-0.877954369402322));
#32501=CARTESIAN_POINT('Ctrl Pts',(95.141287247273,-0.636098816599104,-0.874945160706456));
#32502=CARTESIAN_POINT('Ctrl Pts',(95.1662711054648,-0.685489992710375,
-0.871935952010591));
#32503=CARTESIAN_POINT('Ctrl Pts',(95.1939105468442,-0.73323370416353,-0.868926743314725));
#32504=CARTESIAN_POINT('Ctrl Pts',(95.2150565037084,-0.769760725425008,
-0.866624504408938));
#32505=CARTESIAN_POINT('Ctrl Pts',(95.237755862403,-0.805323924891907,-0.864322265503151));
#32506=CARTESIAN_POINT('Ctrl Pts',(95.2619042701106,-0.839789374450085,
-0.862020026597364));
#32507=CARTESIAN_POINT('Ctrl Pts',(95.2934778596986,-0.884852302511112,
-0.859009892462434));
#32508=CARTESIAN_POINT('Ctrl Pts',(95.3276626704499,-0.928226826378056,
-0.855999758327504));
#32509=CARTESIAN_POINT('Ctrl Pts',(95.364251671266,-0.96959456443078,-0.852989624192575));
#32510=CARTESIAN_POINT('Ctrl Pts',(95.4007756417765,-1.0108887788402,-0.849984840024524));
#32511=CARTESIAN_POINT('Ctrl Pts',(95.4396949754759,-1.05018289318898,-0.846980055856473));
#32512=CARTESIAN_POINT('Ctrl Pts',(95.4807606953364,-1.08718925373214,-0.843975271688422));
#32513=CARTESIAN_POINT('Ctrl Pts',(95.5217857864876,-1.12415900172672,-0.840973460328415));
#32514=CARTESIAN_POINT('Ctrl Pts',(95.5649526667679,-1.15884512781821,-0.837971648968408));
#32515=CARTESIAN_POINT('Ctrl Pts',(95.6099748933604,-1.19099609501409,-0.834969837608402));
#32516=CARTESIAN_POINT('Ctrl Pts',(95.6549703593724,-1.22312795212576,-0.831969810482988));
#32517=CARTESIAN_POINT('Ctrl Pts',(95.7018185569693,-1.25272733074513,-0.828969783357574));
#32518=CARTESIAN_POINT('Ctrl Pts',(95.7502010919244,-1.2795838283649,-0.82596975623216));
#32519=CARTESIAN_POINT('Ctrl Pts',(95.79857397761,-1.3064349698043,-0.822970327423273));
#32520=CARTESIAN_POINT('Ctrl Pts',(95.8484801314558,-1.33054406046041,-0.819970898614386));
#32521=CARTESIAN_POINT('Ctrl Pts',(95.8995754002831,-1.35174598751809,-0.816971469805499));
#32522=CARTESIAN_POINT('Ctrl Pts',(95.9507176405937,-1.37296740534246,-0.813969283645031));
#32523=CARTESIAN_POINT('Ctrl Pts',(96.003050691011,-1.39127611735242,-0.810967097484562));
#32524=CARTESIAN_POINT('Ctrl Pts',(96.0562105796949,-1.40655526661251,-0.807964911324094));
#32525=CARTESIAN_POINT('Ctrl Pts',(96.1093946638648,-1.42184137010918,-0.804961358731997));
#32526=CARTESIAN_POINT('Ctrl Pts',(96.1634058205693,-1.43409504507892,-0.801957806139899));
#32527=CARTESIAN_POINT('Ctrl Pts',(96.217868306426,-1.44325027468672,-0.798954253547802));
#32528=CARTESIAN_POINT('Ctrl Pts',(96.2724335770256,-1.45242278257159,-0.795945032478112));
#32529=CARTESIAN_POINT('Ctrl Pts',(96.3274513521043,-1.45848510569075,-0.792935811408423));
#32530=CARTESIAN_POINT('Ctrl Pts',(96.3825403296723,-1.46142311113821,-0.789926590338733));
#32531=CARTESIAN_POINT('Ctrl Pts',(96.4246848451709,-1.46367076251207,-0.787624457142423));
#32532=CARTESIAN_POINT('Ctrl Pts',(96.4668709014751,-1.46409093676975,-0.785322323946113));
#32533=CARTESIAN_POINT('Ctrl Pts',(96.5089293361716,-1.46269785117651,-0.783020190749803));
#32534=CARTESIAN_POINT('Ctrl Pts',(96.5639227450316,-1.46087632533612,-0.780010041821803));
#32535=CARTESIAN_POINT('Ctrl Pts',(96.618928819811,-1.45594525965707,-0.776999892893803));
#32536=CARTESIAN_POINT('Ctrl Pts',(96.6735677828057,-1.44790408919395,-0.773989743965802));
#32537=CARTESIAN_POINT('Ctrl Pts',(96.7281096409166,-1.43987720957533,-0.770984944703056));
#32538=CARTESIAN_POINT('Ctrl Pts',(96.7822851637495,-1.42875127042837,-0.76798014544031));
#32539=CARTESIAN_POINT('Ctrl Pts',(96.8357173904326,-1.41457762722801,-0.764975346177563));
#32540=CARTESIAN_POINT('Ctrl Pts',(96.8890967568334,-1.40041800595463,-0.76197351955038));
#32541=CARTESIAN_POINT('Ctrl Pts',(96.9417337758131,-1.38321678810163,-0.758971692923197));
#32542=CARTESIAN_POINT('Ctrl Pts',(96.9932612645381,-1.36307644172656,-0.755969866296014));
#32543=CARTESIAN_POINT('Ctrl Pts',(97.0447581286649,-1.34294806546747,-0.752969823759938));
#32544=CARTESIAN_POINT('Ctrl Pts',(97.095146278689,-1.31988421488643,-0.749969781223863));
#32545=CARTESIAN_POINT('Ctrl Pts',(97.1440755252397,-1.29403659381197,-0.746969738687787));
#32546=CARTESIAN_POINT('Ctrl Pts',(97.1929950154074,-1.26819412669574,-0.743970294353529));
#32547=CARTESIAN_POINT('Ctrl Pts',(97.2404557131263,-1.23956923798579,-0.740970850019272));
#32548=CARTESIAN_POINT('Ctrl Pts',(97.2861312860237,-1.20835995130818,-0.737971405685014));
#32549=CARTESIAN_POINT('Ctrl Pts',(97.3318488486723,-1.17712197379864,-0.734969203948634));
#32550=CARTESIAN_POINT('Ctrl Pts',(97.3757775708721,-1.14329515026359,-0.731967002212255));
#32551=CARTESIAN_POINT('Ctrl Pts',(97.41762070718,-1.1071204696941,-0.728964800475876));
#32552=CARTESIAN_POINT('Ctrl Pts',(97.4594828888301,-1.07092932383948,-0.7259612322559));
#32553=CARTESIAN_POINT('Ctrl Pts',(97.499257212345,-1.03238855880676,-0.722957664035924));
#32554=CARTESIAN_POINT('Ctrl Pts',(97.5366830803905,-0.991776801317935,
-0.719954095815949));
#32555=CARTESIAN_POINT('Ctrl Pts',(97.5741795789177,-0.951088400904303,
-0.716944859231256));
#32556=CARTESIAN_POINT('Ctrl Pts',(97.6093184322226,-0.908321609442644,
-0.713935622646564));
#32557=CARTESIAN_POINT('Ctrl Pts',(97.64187946,-0.863788058247059,-0.710926386061871));
#32558=CARTESIAN_POINT('Ctrl Pts',(97.6667880446296,-0.82972071441527,-0.708624375675328));
#32559=CARTESIAN_POINT('Ctrl Pts',(97.6901889246574,-0.794620167352733,
-0.706322365288784));
#32560=CARTESIAN_POINT('Ctrl Pts',(97.7120015906264,-0.758635838216996,
-0.70402035490224));
#32561=CARTESIAN_POINT('Ctrl Pts',(97.741399837912,-0.710137584594984,-0.700917796476155));
#32562=CARTESIAN_POINT('Ctrl Pts',(97.7680288183907,-0.659840015559768,
-0.69781523805007));
#32563=CARTESIAN_POINT('Ctrl Pts',(97.7916721500935,-0.60808078218895,-0.694712679623984));
#32564=CARTESIAN_POINT('Ctrl Pts',(97.8152569502764,-0.556449684168549,
-0.691617801903065));
#32565=CARTESIAN_POINT('Ctrl Pts',(97.8358705995206,-0.503364553578691,
-0.688522924182145));
#32566=CARTESIAN_POINT('Ctrl Pts',(97.8533420610875,-0.449188350296177,
-0.685428046461226));
#32567=CARTESIAN_POINT('Ctrl Pts',(97.870787851703,-0.395091748521366,-0.68233771606769));
#32568=CARTESIAN_POINT('Ctrl Pts',(97.8851004704575,-0.339907713157234,
-0.679247385674154));
#32569=CARTESIAN_POINT('Ctrl Pts',(97.8961568904179,-0.284019088954735,
-0.676157055280619));
#32570=CARTESIAN_POINT('Ctrl Pts',(97.9071974005993,-0.228210886413188,
-0.6730711717581));
#32571=CARTESIAN_POINT('Ctrl Pts',(97.9149909322888,-0.171700582918234,
-0.669985288235581));
#32572=CARTESIAN_POINT('Ctrl Pts',(97.9194648072646,-0.114884085090813,
-0.666899404713062));
#32573=CARTESIAN_POINT('Ctrl Pts',(97.9224824714857,-0.0765609058358133,
-0.664817951756339));
#32574=CARTESIAN_POINT('Ctrl Pts',(97.9239908603876,-0.0380987204141508,
-0.662736498799616));
#32575=CARTESIAN_POINT('Ctrl Pts',(97.923980900548,0.000378824190018902,
-0.660655045842893));
#32576=CARTESIAN_POINT('Ctrl Pts',(97.9239809152274,0.000317082584714552,
-0.589344954157071));
#32577=CARTESIAN_POINT('Ctrl Pts',(97.9239933057583,-0.0568716200036579,
-0.592438318784791));
#32578=CARTESIAN_POINT('Ctrl Pts',(97.9206492531944,-0.114020603425716,
-0.595531683412511));
#32579=CARTESIAN_POINT('Ctrl Pts',(97.9139886755651,-0.170726507880078,
-0.598625048040231));
#32580=CARTESIAN_POINT('Ctrl Pts',(97.9073139831515,-0.227552580832559,
-0.601724967981458));
#32581=CARTESIAN_POINT('Ctrl Pts',(97.8973087906183,-0.283933222963652,
-0.604824887922686));
#32582=CARTESIAN_POINT('Ctrl Pts',(97.8840645854727,-0.339472946801535,
-0.607924807863914));
#32583=CARTESIAN_POINT('Ctrl Pts',(97.8708054908208,-0.395075109951672,
-0.611028212821915));
#32584=CARTESIAN_POINT('Ctrl Pts',(97.854300269648,-0.449834012993639,-0.614131617779916));
#32585=CARTESIAN_POINT('Ctrl Pts',(97.8346900561714,-0.503370222950273,
-0.617235022737918));
#32586=CARTESIAN_POINT('Ctrl Pts',(97.8150310332347,-0.557039683547313,
-0.620346152013692));
#32587=CARTESIAN_POINT('Ctrl Pts',(97.7922517696555,-0.609479930850509,
-0.623457281289467));
#32588=CARTESIAN_POINT('Ctrl Pts',(97.7665410147506,-0.660332761688246,
-0.626568410565242));
#32589=CARTESIAN_POINT('Ctrl Pts',(97.7515821912859,-0.689919544417623,
-0.62837850263699));
#32590=CARTESIAN_POINT('Ctrl Pts',(97.7356318962316,-0.718969462504072,
-0.630188594708739));
#32591=CARTESIAN_POINT('Ctrl Pts',(97.7187340105644,-0.747416540167404,
-0.631998686780487));
#32592=CARTESIAN_POINT('Ctrl Pts',(97.6906322104425,-0.794725067771984,
-0.635008935908942));
#32593=CARTESIAN_POINT('Ctrl Pts',(97.659799592515,-0.840545848997746,-0.638019185037397));
#32594=CARTESIAN_POINT('Ctrl Pts',(97.6264187277055,-0.884545842527611,
-0.641029434165853));
#32595=CARTESIAN_POINT('Ctrl Pts',(97.5930971746869,-0.928467655985254,
-0.644034334623197));
#32596=CARTESIAN_POINT('Ctrl Pts',(97.557236676801,-0.970574684766163,-0.647039235080541));
#32597=CARTESIAN_POINT('Ctrl Pts',(97.5190639381818,-1.0105613817263,-0.650044135537886));
#32598=CARTESIAN_POINT('Ctrl Pts',(97.4809289557043,-1.050508528383,-0.653046063888656));
#32599=CARTESIAN_POINT('Ctrl Pts',(97.4404866258037,-1.08833911758349,-0.656047992239426));
#32600=CARTESIAN_POINT('Ctrl Pts',(97.3980037229298,-1.12378080578237,-0.659049920590196));
#32601=CARTESIAN_POINT('Ctrl Pts',(97.3555460634466,-1.15920143448855,-0.66205006519162));
#32602=CARTESIAN_POINT('Ctrl Pts',(97.3110506389538,-1.19223563811482,-0.665050209793043));
#32603=CARTESIAN_POINT('Ctrl Pts',(97.2648191723575,-1.22264969364665,-0.668050354394467));
#32604=CARTESIAN_POINT('Ctrl Pts',(97.2185969215074,-1.25305768646333,-0.671049900949303));
#32605=CARTESIAN_POINT('Ctrl Pts',(97.1706397567342,-1.28084627838922,-0.67404944750414));
#32606=CARTESIAN_POINT('Ctrl Pts',(97.1212784867775,-1.30582497480703,-0.677048994058976));
#32607=CARTESIAN_POINT('Ctrl Pts',(97.0718718499882,-1.33082662858267,-0.680051297429556));
#32608=CARTESIAN_POINT('Ctrl Pts',(97.0210590019866,-1.35301298838269,-0.683053600800137));
#32609=CARTESIAN_POINT('Ctrl Pts',(96.9691941368395,-1.37224019147716,-0.686055904170717));
#32610=CARTESIAN_POINT('Ctrl Pts',(96.9173056685843,-1.39147614465225,-0.689059573855287));
#32611=CARTESIAN_POINT('Ctrl Pts',(96.8643647344388,-1.40775010116467,-0.692063243539857));
#32612=CARTESIAN_POINT('Ctrl Pts',(96.8107410842013,-1.42096801093233,-0.695066913224427));
#32613=CARTESIAN_POINT('Ctrl Pts',(96.7570162660442,-1.43421085798841,-0.698076249718543));
#32614=CARTESIAN_POINT('Ctrl Pts',(96.7026066790907,-1.4443860432448,-0.701085586212659));
#32615=CARTESIAN_POINT('Ctrl Pts',(96.6478915120193,-1.45145083660628,-0.704094922706775));
#32616=CARTESIAN_POINT('Ctrl Pts',(96.6060515445464,-1.45685319102222,-0.706396122680534));
#32617=CARTESIAN_POINT('Ctrl Pts',(96.5640331021084,-1.46043782114926,-0.708697322654292));
#32618=CARTESIAN_POINT('Ctrl Pts',(96.5220057229805,-1.46220619348218,-0.71099852262805));
#32619=CARTESIAN_POINT('Ctrl Pts',(96.4670300437293,-1.46451938721895,-0.71400870394974));
#32620=CARTESIAN_POINT('Ctrl Pts',(96.4118082692967,-1.46373268471372,-0.717018885271431));
#32621=CARTESIAN_POINT('Ctrl Pts',(96.3567190720768,-1.45981701688178,-0.720029066593121));
#32622=CARTESIAN_POINT('Ctrl Pts',(96.3017277439178,-1.45590830545424,-0.723033900158189));
#32623=CARTESIAN_POINT('Ctrl Pts',(96.2468690480662,-1.44888169729207,-0.726038733723258));
#32624=CARTESIAN_POINT('Ctrl Pts',(96.1925227449652,-1.4387601087677,-0.729043567288326));
#32625=CARTESIAN_POINT('Ctrl Pts',(96.1382301851588,-1.42864852952606,-0.732045429360466));
#32626=CARTESIAN_POINT('Ctrl Pts',(96.084449530955,-1.4154481291282,-0.735047291432605));
#32627=CARTESIAN_POINT('Ctrl Pts',(96.0315546285661,-1.39923352630791,-0.738049153504745));
#32628=CARTESIAN_POINT('Ctrl Pts',(95.9786911441165,-1.3830285544612,-0.741049232563472));
#32629=CARTESIAN_POINT('Ctrl Pts',(95.9267128725939,-1.36381308324272,-0.744049311622199));
#32630=CARTESIAN_POINT('Ctrl Pts',(95.8759804102237,-1.3417121038046,-0.747049390680926));
#32631=CARTESIAN_POINT('Ctrl Pts',(95.8252580465204,-1.31961552372768,-0.750048872552027));
#32632=CARTESIAN_POINT('Ctrl Pts',(95.7757814833515,-1.29463478692838,-0.753048354423129));
#32633=CARTESIAN_POINT('Ctrl Pts',(95.7278910040907,-1.2669428644467,-0.75604783629423));
#32634=CARTESIAN_POINT('Ctrl Pts',(95.6799564790391,-1.23922547317367,-0.759050076846242));
#32635=CARTESIAN_POINT('Ctrl Pts',(95.6336114104374,-1.2087921793971,-0.762052317398254));
#32636=CARTESIAN_POINT('Ctrl Pts',(95.5891698035265,-1.17586101932509,-0.765054557950266));
#32637=CARTESIAN_POINT('Ctrl Pts',(95.5447079574132,-1.14291486203625,-0.768058165756041));
#32638=CARTESIAN_POINT('Ctrl Pts',(95.5021517074917,-1.10746890938361,-0.771061773561816));
#32639=CARTESIAN_POINT('Ctrl Pts',(95.4617818382794,-1.06978144267575,-0.774065381367591));
#32640=CARTESIAN_POINT('Ctrl Pts',(95.4213357732141,-1.03202284299844,-0.777074658313824));
#32641=CARTESIAN_POINT('Ctrl Pts',(95.3830846983588,-0.992014660367753,
-0.780083935260056));
#32642=CARTESIAN_POINT('Ctrl Pts',(95.3472715729962,-0.950051121725918,
-0.783093212206289));
#32643=CARTESIAN_POINT('Ctrl Pts',(95.3198790715849,-0.91795433375132,-0.785394927629397));
#32644=CARTESIAN_POINT('Ctrl Pts',(95.2939120705789,-0.884714360878225,
-0.787696643052505));
#32645=CARTESIAN_POINT('Ctrl Pts',(95.2694620343073,-0.850474099235069,
-0.789998358475612));
#32646=CARTESIAN_POINT('Ctrl Pts',(95.2374875008111,-0.805696399085065,
-0.793008426684806));
#32647=CARTESIAN_POINT('Ctrl Pts',(95.2079744710546,-0.759018892219084,
-0.796018494894));
#32648=CARTESIAN_POINT('Ctrl Pts',(95.1811542053125,-0.710742802573144,
-0.799028563103194));
#32649=CARTESIAN_POINT('Ctrl Pts',(95.154381620755,-0.66255253836869,-0.802033280000075));
#32650=CARTESIAN_POINT('Ctrl Pts',(95.1302925543921,-0.612769789221488,
-0.805037996896956));
#32651=CARTESIAN_POINT('Ctrl Pts',(95.1090753245261,-0.561725098763481,
-0.808042713793837));
#32652=CARTESIAN_POINT('Ctrl Pts',(95.0878790920242,-0.510730924039845,
-0.811044457110523));
#32653=CARTESIAN_POINT('Ctrl Pts',(95.069549267728,-0.458477767230515,-0.814046200427208));
#32654=CARTESIAN_POINT('Ctrl Pts',(95.0542276384143,-0.405319472569289,
-0.817047943743894));
#32655=CARTESIAN_POINT('Ctrl Pts',(95.0389151195809,-0.352192786661084,
-0.820047902177077));
#32656=CARTESIAN_POINT('Ctrl Pts',(95.0266073963545,-0.298162536132881,
-0.823047860610261));
#32657=CARTESIAN_POINT('Ctrl Pts',(95.0173968287886,-0.243598994924626,
-0.826047819043444));
#32658=CARTESIAN_POINT('Ctrl Pts',(95.00818809981,-0.189046345535501,-0.829047178633446));
#32659=CARTESIAN_POINT('Ctrl Pts',(95.0020753865468,-0.133961137359882,
-0.832046538223447));
#32660=CARTESIAN_POINT('Ctrl Pts',(94.999099766334,-0.078722850959899,-0.835045897813449));
#32661=CARTESIAN_POINT('Ctrl Pts',(94.9961214108576,-0.0234337881634231,
-0.838048014488828));
#32662=CARTESIAN_POINT('Ctrl Pts',(94.9962859381515,0.032008105474783,-0.841050131164208));
#32663=CARTESIAN_POINT('Ctrl Pts',(94.99958232411,0.0872207321028154,-0.844052247839588));
#32664=CARTESIAN_POINT('Ctrl Pts',(95.0028802101587,0.142458484404836,-0.847055730691683));
#32665=CARTESIAN_POINT('Ctrl Pts',(95.0093127344966,0.197466236235169,-0.850059213543777));
#32666=CARTESIAN_POINT('Ctrl Pts',(95.0188170147424,0.251867721229272,-0.853062696395872));
#32667=CARTESIAN_POINT('Ctrl Pts',(95.0283392338549,0.306371886380417,-0.856071848175772));
#32668=CARTESIAN_POINT('Ctrl Pts',(95.0409446702839,0.360266983256315,-0.859080999955672));
#32669=CARTESIAN_POINT('Ctrl Pts',(95.0565196682152,0.413188783048457,-0.862090151735572));
#32670=CARTESIAN_POINT('Ctrl Pts',(95.0684380599395,0.453685914634258,-0.864392832598106));
#32671=CARTESIAN_POINT('Ctrl Pts',(95.0820942802859,0.493613346500161,-0.866695513460641));
#32672=CARTESIAN_POINT('Ctrl Pts',(95.0974185321669,0.532816193676603,-0.868998194323175));
#32673=CARTESIAN_POINT('Ctrl Pts',(95.1174509546978,0.584063589318232,-0.87200834296538));
#32674=CARTESIAN_POINT('Ctrl Pts',(95.1404196226556,0.634287332484554,-0.875018491607585));
#32675=CARTESIAN_POINT('Ctrl Pts',(95.1661985880499,0.683129137601182,-0.878028640249789));
#32676=CARTESIAN_POINT('Ctrl Pts',(95.1919317396107,0.731884142092216,-0.881033439319335));
#32677=CARTESIAN_POINT('Ctrl Pts',(95.220465032665,0.779261619118995,-0.88403823838888));
#32678=CARTESIAN_POINT('Ctrl Pts',(95.2516245008862,0.824923230645582,-0.887043037458425));
#32679=CARTESIAN_POINT('Ctrl Pts',(95.28275314376,0.870539670186896,-0.89004486394915));
#32680=CARTESIAN_POINT('Ctrl Pts',(95.3165025190425,0.914443172754508,-0.893046690439876));
#32681=CARTESIAN_POINT('Ctrl Pts',(95.3526537221496,0.956321642634158,-0.896048516930601));
#32682=CARTESIAN_POINT('Ctrl Pts',(95.3887834400069,0.998175223455973,-0.899048559386872));
#32683=CARTESIAN_POINT('Ctrl Pts',(95.4273118119942,1.03800575806257,-0.902048601843144));
#32684=CARTESIAN_POINT('Ctrl Pts',(95.4679791679586,1.07553357152821,-0.905048644299415));
#32685=CARTESIAN_POINT('Ctrl Pts',(95.5086384157101,1.11305390273951,-0.908048088610508));
#32686=CARTESIAN_POINT('Ctrl Pts',(95.5514354125987,1.14827206664514,-0.911047532921601));
#32687=CARTESIAN_POINT('Ctrl Pts',(95.5960747582377,1.18094630969162,-0.914046977232694));
#32688=CARTESIAN_POINT('Ctrl Pts',(95.6407551423232,1.21365059126475,-0.917049179033462));
#32689=CARTESIAN_POINT('Ctrl Pts',(95.6872808319539,1.24380596694346,-0.920051380834231));
#32690=CARTESIAN_POINT('Ctrl Pts',(95.7353257677288,1.27121289021105,-0.923053582634999));
#32691=CARTESIAN_POINT('Ctrl Pts',(95.7833925724393,1.29863228847165,-0.92605715096809));
#32692=CARTESIAN_POINT('Ctrl Pts',(95.8329795281481,1.32330050484317,-0.929060719301182));
#32693=CARTESIAN_POINT('Ctrl Pts',(95.8837371250765,1.34506461216572,-0.932064287634273));
#32694=CARTESIAN_POINT('Ctrl Pts',(95.9345905135792,1.36686979349945,-0.935073524410251));
#32695=CARTESIAN_POINT('Ctrl Pts',(95.9866184590551,1.38575973648157,-0.938082761186229));
#32696=CARTESIAN_POINT('Ctrl Pts',(96.0394537917025,1.40163061550898,-0.941091997962207));
#32697=CARTESIAN_POINT('Ctrl Pts',(96.0798718485249,1.41377154579581,-0.943394008698384));
#32698=CARTESIAN_POINT('Ctrl Pts',(96.1207620034452,1.42414674519917,-0.945696019434562));
#32699=CARTESIAN_POINT('Ctrl Pts',(96.1619565525049,1.43273006332412,-0.947998030170739));
#32700=CARTESIAN_POINT('Ctrl Pts',(96.2158229736495,1.44395369944809,-0.951008163370999));
#32701=CARTESIAN_POINT('Ctrl Pts',(96.2704364123061,1.45215886524671,-0.95401829657126));
#32702=CARTESIAN_POINT('Ctrl Pts',(96.3254279810839,1.45725527815177,-0.95702842977152));
#32703=CARTESIAN_POINT('Ctrl Pts',(96.3803218186441,1.46234263369313,-0.960033213352021));
#32704=CARTESIAN_POINT('Ctrl Pts',(96.4355919311008,1.46433215217651,-0.963037996932523));
#32705=CARTESIAN_POINT('Ctrl Pts',(96.4908599002698,1.46318466686704,-0.966042780513024));
#32706=CARTESIAN_POINT('Ctrl Pts',(96.5460731935169,1.46203831675066,-0.969044591498098));
#32707=CARTESIAN_POINT('Ctrl Pts',(96.6012838222717,1.45776112143561,-0.972046402483172));
#32708=CARTESIAN_POINT('Ctrl Pts',(96.6561107926275,1.45036588987332,-0.975048213468245));
#32709=CARTESIAN_POINT('Ctrl Pts',(96.7109051784694,1.4429750534112,-0.978048240430755));
#32710=CARTESIAN_POINT('Ctrl Pts',(96.7653158355214,1.43246992411588,-0.981048267393265));
#32711=CARTESIAN_POINT('Ctrl Pts',(96.8189666488126,1.41891516781079,-0.984048294355775));
#32712=CARTESIAN_POINT('Ctrl Pts',(96.87260676593,1.40536311386977,-0.987047723213468));
#32713=CARTESIAN_POINT('Ctrl Pts',(96.9254868283957,1.38876276965795,-0.99004715207116));
#32714=CARTESIAN_POINT('Ctrl Pts',(96.9772429584354,1.36922944614868,-0.993046580928853));
#32715=CARTESIAN_POINT('Ctrl Pts',(97.0290466731114,1.34967816368277,-0.996048767464354));
#32716=CARTESIAN_POINT('Ctrl Pts',(97.0797238957159,1.32718870137387,-0.999050953999855));
#32717=CARTESIAN_POINT('Ctrl Pts',(97.1289293459707,1.30192510973508,-1.00205314053536));
#32718=CARTESIAN_POINT('Ctrl Pts',(97.1781571948424,1.27665001795743,-1.00505669368422));
#32719=CARTESIAN_POINT('Ctrl Pts',(97.2259114796891,1.24859854749759,-1.00806024683309));
#32720=CARTESIAN_POINT('Ctrl Pts',(97.2718731520585,1.21797986180077,-1.01106379998196));
#32721=CARTESIAN_POINT('Ctrl Pts',(97.3179215703662,1.1873033878103,-1.01407302189835));
#32722=CARTESIAN_POINT('Ctrl Pts',(97.3621701943197,1.15405033751025,-1.01708224381475));
#32723=CARTESIAN_POINT('Ctrl Pts',(97.4043314500332,1.11847149395439,-1.02009146573115));
#32724=CARTESIAN_POINT('Ctrl Pts',(97.4365859127766,1.09125274858017,-1.0223935991602));
#32725=CARTESIAN_POINT('Ctrl Pts',(97.4676193537472,1.06267367304437,-1.02469573258925));
#32726=CARTESIAN_POINT('Ctrl Pts',(97.4973182204881,1.03286045700743,-1.0269978660183));
#32727=CARTESIAN_POINT('Ctrl Pts',(97.5355982365663,0.994433051706249,-1.02996517468524));
#32728=CARTESIAN_POINT('Ctrl Pts',(97.5718303382193,0.953782712209917,-1.03293248335217));
#32729=CARTESIAN_POINT('Ctrl Pts',(97.6057410346534,0.911159474258424,-1.0358997920191));
#32730=CARTESIAN_POINT('Ctrl Pts',(97.6396034125982,0.868596969075096,-1.03886287264335));
#32731=CARTESIAN_POINT('Ctrl Pts',(97.6711505948298,0.824067549603088,-1.0418259532676));
#32732=CARTESIAN_POINT('Ctrl Pts',(97.7001459760191,0.777857874046635,-1.04478903389186));
#32733=CARTESIAN_POINT('Ctrl Pts',(97.7291122718648,0.731694551537961,-1.04774914224209));
#32734=CARTESIAN_POINT('Ctrl Pts',(97.7555315468684,0.683854768797007,-1.05070925059233));
#32735=CARTESIAN_POINT('Ctrl Pts',(97.779209119628,0.634656019835896,-1.05366935894257));
#32736=CARTESIAN_POINT('Ctrl Pts',(97.8029895413964,0.585243564739738,-1.05664232520746));
#32737=CARTESIAN_POINT('Ctrl Pts',(97.8240040853246,0.534460775308565,-1.05961529147234));
#32738=CARTESIAN_POINT('Ctrl Pts',(97.8421020126223,0.482654626155905,-1.06258825773722));
#32739=CARTESIAN_POINT('Ctrl Pts',(97.8601149766387,0.431091688302801,-1.0655472669912));
#32740=CARTESIAN_POINT('Ctrl Pts',(97.8752384986032,0.378515507001031,-1.06850627624518));
#32741=CARTESIAN_POINT('Ctrl Pts',(97.8873731861014,0.32528571340656,-1.07146528549916));
#32742=CARTESIAN_POINT('Ctrl Pts',(97.8995937286703,0.271679309562145,-1.07444523026949));
#32743=CARTESIAN_POINT('Ctrl Pts',(97.9087828366365,0.217410549822793,-1.07742517503983));
#32744=CARTESIAN_POINT('Ctrl Pts',(97.9148914798562,0.162856560853815,-1.08040511981017));
#32745=CARTESIAN_POINT('Ctrl Pts',(97.9210001230758,0.108302571884838,-1.08338506458051));
#32746=CARTESIAN_POINT('Ctrl Pts',(97.9240283002846,0.0534639155643919,
-1.08636500935085));
#32747=CARTESIAN_POINT('Ctrl Pts',(97.9239803891082,-0.00128081692310628,
-1.08934495412119));
#32748=CARTESIAN_POINT('Origin',(96.460480949577,-8.32667268468867E-16,
1.18130019239114E-14));
#32749=CARTESIAN_POINT('',(97.9239806916945,0.000868804938495186,-1.66065504587772));
#32750=CARTESIAN_POINT('',(97.9239806575939,0.000924464373925031,-1.58934495419106));
#32751=CARTESIAN_POINT('',(97.923980949577,-1.01189432752408E-15,1.19922289829666E-14));
#32752=CARTESIAN_POINT('Ctrl Pts',(97.9239806916941,0.00086880557632569,
-1.66065504584289));
#32753=CARTESIAN_POINT('Ctrl Pts',(97.9239493983902,0.0535822589773747,
-1.65777615891959));
#32754=CARTESIAN_POINT('Ctrl Pts',(97.9210702361685,0.106209644580605,-1.65489727199629));
#32755=CARTESIAN_POINT('Ctrl Pts',(97.9153700635578,0.158524181184318,-1.65201838507299));
#32756=CARTESIAN_POINT('Ctrl Pts',(97.9094100334058,0.213223615190671,-1.64900825642623));
#32757=CARTESIAN_POINT('Ctrl Pts',(97.9003483914511,0.267701392550938,-1.64599812777947));
#32758=CARTESIAN_POINT('Ctrl Pts',(97.8882131864674,0.32157877688655,-1.64298799913271));
#32759=CARTESIAN_POINT('Ctrl Pts',(97.876099549162,0.375360405930611,-1.63998322033264));
#32760=CARTESIAN_POINT('Ctrl Pts',(97.8609233044749,0.428543248510851,-1.63697844153257));
#32761=CARTESIAN_POINT('Ctrl Pts',(97.8427640618136,0.48075528871314,-1.63397366273249));
#32762=CARTESIAN_POINT('Ctrl Pts',(97.824622784714,0.532915673752846,-1.63097185666317));
#32763=CARTESIAN_POINT('Ctrl Pts',(97.8035045284219,0.584106662660049,-1.62797005059385));
#32764=CARTESIAN_POINT('Ctrl Pts',(97.7795391329655,0.633969840635917,-1.62496824452453));
#32765=CARTESIAN_POINT('Ctrl Pts',(97.7555879815453,0.683803382008644,-1.62196822260413));
#32766=CARTESIAN_POINT('Ctrl Pts',(97.728793273371,0.732310201644931,-1.61896820068373));
#32767=CARTESIAN_POINT('Ctrl Pts',(97.6993326639567,0.779152539480246,-1.61596817876332));
#32768=CARTESIAN_POINT('Ctrl Pts',(97.6698779291648,0.825985536672102,-1.61296875506531));
#32769=CARTESIAN_POINT('Ctrl Pts',(97.6377586298672,0.8711542644181,-1.60996933136729));
#32770=CARTESIAN_POINT('Ctrl Pts',(97.6031968122026,0.914348241811566,-1.60696990766928));
#32771=CARTESIAN_POINT('Ctrl Pts',(97.5686032199489,0.95758192981558,-1.60396772643529));
#32772=CARTESIAN_POINT('Ctrl Pts',(97.5315629536859,0.998836827095143,-1.60096554520131));
#32773=CARTESIAN_POINT('Ctrl Pts',(97.4923386735164,1.03783519286378,-1.59796336396732));
#32774=CARTESIAN_POINT('Ctrl Pts',(97.4530965393233,1.07685130982479,-1.59495981620693));
#32775=CARTESIAN_POINT('Ctrl Pts',(97.4116688052513,1.11360849666281,-1.59195626844654));
#32776=CARTESIAN_POINT('Ctrl Pts',(97.3683529384007,1.14786789392742,-1.58895272068615));
#32777=CARTESIAN_POINT('Ctrl Pts',(97.3249553201348,1.18219195004367,-1.58594350423441));
#32778=CARTESIAN_POINT('Ctrl Pts',(97.2796628835873,1.21400849500905,-1.58293428778266));
#32779=CARTESIAN_POINT('Ctrl Pts',(97.2328029612089,1.24312145840578,-1.57992507133092));
#32780=CARTESIAN_POINT('Ctrl Pts',(97.1969531982159,1.2653940697295,-1.57762289729576));
#32781=CARTESIAN_POINT('Ctrl Pts',(97.1601866391868,1.28608518851574,-1.57532072326059));
#32782=CARTESIAN_POINT('Ctrl Pts',(97.1226583816472,1.30512577878795,-1.57301854922542));
#32783=CARTESIAN_POINT('Ctrl Pts',(97.0735895963715,1.3300216491759,-1.57000842057024));
#32784=CARTESIAN_POINT('Ctrl Pts',(97.023011745983,1.35219872387494,-1.56699829191506));
#32785=CARTESIAN_POINT('Ctrl Pts',(96.9712573581323,1.37147355441633,-1.56398816325988));
#32786=CARTESIAN_POINT('Ctrl Pts',(96.9195949524165,1.39071412815095,-1.56098338445177));
#32787=CARTESIAN_POINT('Ctrl Pts',(96.8667606498236,1.40706251119664,-1.55797860564366));
#32788=CARTESIAN_POINT('Ctrl Pts',(96.8131095219622,1.42038211053843,-1.55497382683554));
#32789=CARTESIAN_POINT('Ctrl Pts',(96.7595114730062,1.43368853234262,-1.55197202075842));
#32790=CARTESIAN_POINT('Ctrl Pts',(96.7050987096523,1.44397197970206,-1.5489702146813));
#32791=CARTESIAN_POINT('Ctrl Pts',(96.650242358023,1.4511453606943,-1.54596840860417));
#32792=CARTESIAN_POINT('Ctrl Pts',(96.5954186107365,1.45831447812607,-1.54296838667622));
#32793=CARTESIAN_POINT('Ctrl Pts',(96.5401523203595,1.46237712468802,-1.53996836474827));
#32794=CARTESIAN_POINT('Ctrl Pts',(96.484823440313,1.46329754087976,-1.53696834282032));
#32795=CARTESIAN_POINT('Ctrl Pts',(96.4295055931821,1.46421777353491,-1.53396891911501));
#32796=CARTESIAN_POINT('Ctrl Pts',(96.374125708915,1.46199701140134,-1.5309694954097));
#32797=CARTESIAN_POINT('Ctrl Pts',(96.3190651487667,1.45665157854621,-1.52797007170439));
#32798=CARTESIAN_POINT('Ctrl Pts',(96.2639539684111,1.45130123134007,-1.52496789046357));
#32799=CARTESIAN_POINT('Ctrl Pts',(96.2091632254679,1.44282052530776,-1.52196570922275));
#32800=CARTESIAN_POINT('Ctrl Pts',(96.1550690517712,1.43127768887756,-1.51896352798193));
#32801=CARTESIAN_POINT('Ctrl Pts',(96.1009502556092,1.4197295984048,-1.51595998021495));
#32802=CARTESIAN_POINT('Ctrl Pts',(96.0475291710268,1.40511673864792,-1.51295643244796));
#32803=CARTESIAN_POINT('Ctrl Pts',(95.9951683840998,1.38755773444171,-1.50995288468098));
#32804=CARTESIAN_POINT('Ctrl Pts',(95.9427087750004,1.36996559057045,-1.50694366822311));
#32805=CARTESIAN_POINT('Ctrl Pts',(95.8913139527062,1.34941639113035,-1.50393445176525));
#32806=CARTESIAN_POINT('Ctrl Pts',(95.8413269846373,1.32607715375067,-1.50092523530739));
#32807=CARTESIAN_POINT('Ctrl Pts',(95.80308490446,1.3082216801816,-1.49862306133088));
#32808=CARTESIAN_POINT('Ctrl Pts',(95.7656664330478,1.28873424402576,-1.49632088735437));
#32809=CARTESIAN_POINT('Ctrl Pts',(95.7292141345577,1.26770702264027,-1.49401871337787));
#32810=CARTESIAN_POINT('Ctrl Pts',(95.6815521802114,1.24021359953075,-1.49100858464771));
#32811=CARTESIAN_POINT('Ctrl Pts',(95.6353427432839,1.20997075436495,-1.48799845591755));
#32812=CARTESIAN_POINT('Ctrl Pts',(95.5909211586164,1.177156752495,-1.4849883271874));
#32813=CARTESIAN_POINT('Ctrl Pts',(95.5465785236169,1.14440107034893,-1.48198354830384));
#32814=CARTESIAN_POINT('Ctrl Pts',(95.5040178564245,1.10908361128876,-1.47897876942029));
#32815=CARTESIAN_POINT('Ctrl Pts',(95.4635475671057,1.07142712347335,-1.47597399053673));
#32816=CARTESIAN_POINT('Ctrl Pts',(95.4231173164316,1.0338078905123,-1.47297218438394));
#32817=CARTESIAN_POINT('Ctrl Pts',(95.3847737315916,0.993854570862867,-1.46997037823114));
#32818=CARTESIAN_POINT('Ctrl Pts',(95.3487925362772,0.95183040597314,-1.46696857207835));
#32819=CARTESIAN_POINT('Ctrl Pts',(95.312832726693,0.909831218504103,-1.46396855007464));
#32820=CARTESIAN_POINT('Ctrl Pts',(95.2792328663936,0.865764025730836,-1.46096852807092));
#32821=CARTESIAN_POINT('Ctrl Pts',(95.2482305099858,0.819927510034295,-1.4579685060672));
#32822=CARTESIAN_POINT('Ctrl Pts',(95.217234335637,0.774100134418602,-1.45496908228618));
#32823=CARTESIAN_POINT('Ctrl Pts',(95.188834932249,0.726504573758012,-1.45196965850515));
#32824=CARTESIAN_POINT('Ctrl Pts',(95.1632270022737,0.677469147788982,-1.44897023472413));
#32825=CARTESIAN_POINT('Ctrl Pts',(95.1375955295234,0.628388640862618,-1.44596805340826));
#32826=CARTESIAN_POINT('Ctrl Pts',(95.1147609024247,0.577866093083683,-1.44296587209239));
#32827=CARTESIAN_POINT('Ctrl Pts',(95.0948714947951,0.526253804746486,-1.43996369077653));
#32828=CARTESIAN_POINT('Ctrl Pts',(95.0749730339511,0.474618023647986,-1.43696014293476));
#32829=CARTESIAN_POINT('Ctrl Pts',(95.0580226268801,0.421892016848949,-1.43395659509298));
#32830=CARTESIAN_POINT('Ctrl Pts',(95.0441190377038,0.368444276105352,-1.43095304725121));
#32831=CARTESIAN_POINT('Ctrl Pts',(95.0301892078499,0.314895661773628,-1.42794383071992));
#32832=CARTESIAN_POINT('Ctrl Pts',(95.0193177870982,0.260623111488979,-1.42493461418863));
#32833=CARTESIAN_POINT('Ctrl Pts',(95.0115523443857,0.206005211240961,-1.42192539765733));
#32834=CARTESIAN_POINT('Ctrl Pts',(95.0056114640013,0.164220289990292,-1.41962322428166));
#32835=CARTESIAN_POINT('Ctrl Pts',(95.0014874118531,0.122233465416819,-1.41732105090598));
#32836=CARTESIAN_POINT('Ctrl Pts',(94.9991808834234,0.0802145040471148,
-1.41501887753031));
#32837=CARTESIAN_POINT('Ctrl Pts',(94.996165060584,0.0252740395133446,-1.41200874899372));
#32838=CARTESIAN_POINT('Ctrl Pts',(94.9962456021385,-0.029952176063699,
-1.40899862045712));
#32839=CARTESIAN_POINT('Ctrl Pts',(94.999456431718,-0.0850858872831129,
-1.40598849192053));
#32840=CARTESIAN_POINT('Ctrl Pts',(95.0026615547491,-0.140121610370722,
-1.40298371323007));
#32841=CARTESIAN_POINT('Ctrl Pts',(95.0089858947382,-0.195064632407521,
-1.39997893453962));
#32842=CARTESIAN_POINT('Ctrl Pts',(95.0184114081778,-0.249534942981575,
-1.39697415584916));
#32843=CARTESIAN_POINT('Ctrl Pts',(95.0278275966346,-0.303951364214357,
-1.39397234988903));
#32844=CARTESIAN_POINT('Ctrl Pts',(95.0403387911852,-0.357895482590965,
-1.3909705439289));
#32845=CARTESIAN_POINT('Ctrl Pts',(95.0558751743951,-0.410992538041389,
-1.38796873796877));
#32846=CARTESIAN_POINT('Ctrl Pts',(95.0714023234266,-0.464058034815733,
-1.38496871615696));
#32847=CARTESIAN_POINT('Ctrl Pts',(95.0899509492582,-0.516276960700702,
-1.38196869434514));
#32848=CARTESIAN_POINT('Ctrl Pts',(95.1114006962819,-0.567287158473805,
-1.37896867253333));
#32849=CARTESIAN_POINT('Ctrl Pts',(95.1328461661028,-0.61828718452033,-1.3759692489431));
#32850=CARTESIAN_POINT('Ctrl Pts',(95.1571914036437,-0.668078474571037,
-1.37296982535288));
#32851=CARTESIAN_POINT('Ctrl Pts',(95.1842678169643,-0.716318567501113,
-1.36997040176265));
#32852=CARTESIAN_POINT('Ctrl Pts',(95.2113691231477,-0.764603010249576,
-1.36696822063438));
#32853=CARTESIAN_POINT('Ctrl Pts',(95.2412063625633,-0.811332945188495,
-1.36396603950611));
#32854=CARTESIAN_POINT('Ctrl Pts',(95.2735655451241,-0.856191609788615,
-1.36096385837785));
#32855=CARTESIAN_POINT('Ctrl Pts',(95.3059394568793,-0.901070693074843,
-1.35796031072218));
#32856=CARTESIAN_POINT('Ctrl Pts',(95.3408372667544,-0.944076397294422,
-1.35495676306652));
#32857=CARTESIAN_POINT('Ctrl Pts',(95.3780043173352,-0.984924662423716,
-1.35195321541085));
#32858=CARTESIAN_POINT('Ctrl Pts',(95.4152415145129,-1.02585002182717,-1.34894399906092));
#32859=CARTESIAN_POINT('Ctrl Pts',(95.4547561300347,-1.06460943735449,-1.34593478271099));
#32860=CARTESIAN_POINT('Ctrl Pts',(95.4962570794472,-1.1009562108785,-1.34292556636105));
#32861=CARTESIAN_POINT('Ctrl Pts',(95.5280070211773,-1.12876299500753,-1.34062339146828));
#32862=CARTESIAN_POINT('Ctrl Pts',(95.5609187717421,-1.15515845393747,-1.33832121657551));
#32863=CARTESIAN_POINT('Ctrl Pts',(95.5948505268175,-1.18004924524072,-1.33601904168274));
#32864=CARTESIAN_POINT('Ctrl Pts',(95.6392168123026,-1.21259433318144,-1.33300891302001));
#32865=CARTESIAN_POINT('Ctrl Pts',(95.6855142634369,-1.2427022656769,-1.32999878435727));
#32866=CARTESIAN_POINT('Ctrl Pts',(95.7334446168608,-1.27013795349584,-1.32698865569453));
#32867=CARTESIAN_POINT('Ctrl Pts',(95.7812897845072,-1.2975248803474,-1.32398387688074));
#32868=CARTESIAN_POINT('Ctrl Pts',(95.8307616405166,-1.3222487273719,-1.32097909806695));
#32869=CARTESIAN_POINT('Ctrl Pts',(95.8815320570206,-1.34411697028485,-1.31797431925316));
#32870=CARTESIAN_POINT('Ctrl Pts',(95.9322522445866,-1.36596357818489,-1.3149725131715));
#32871=CARTESIAN_POINT('Ctrl Pts',(95.9842679650452,-1.38495997056511,-1.31197070708984));
#32872=CARTESIAN_POINT('Ctrl Pts',(96.0372271987598,-1.40095985396412,-1.30896890100819));
#32873=CARTESIAN_POINT('Ctrl Pts',(96.0901549556799,-1.41695022768923,-1.30596887907684));
#32874=CARTESIAN_POINT('Ctrl Pts',(96.1440246098036,-1.42994747006617,-1.3029688571455));
#32875=CARTESIAN_POINT('Ctrl Pts',(96.198467082858,-1.43985450086005,-1.29996883521415));
#32876=CARTESIAN_POINT('Ctrl Pts',(96.2528986997311,-1.44975955612791,-1.29696941150659));
#32877=CARTESIAN_POINT('Ctrl Pts',(96.3079023893993,-1.45657552907886,-1.29396998779902));
#32878=CARTESIAN_POINT('Ctrl Pts',(96.3630992134576,-1.4602565005746,-1.29097056409146));
#32879=CARTESIAN_POINT('Ctrl Pts',(96.4183467829659,-1.46394085618814,-1.28796838285013));
#32880=CARTESIAN_POINT('Ctrl Pts',(96.4737873135262,-1.46448441691325,-1.28496620160881));
#32881=CARTESIAN_POINT('Ctrl Pts',(96.5290385846283,-1.461893327393,-1.28196402036748));
#32882=CARTESIAN_POINT('Ctrl Pts',(96.5843150048629,-1.45930105846724,-1.27896047260096));
#32883=CARTESIAN_POINT('Ctrl Pts',(96.6394014677138,-1.45357134975605,-1.27595692483444));
#32884=CARTESIAN_POINT('Ctrl Pts',(96.6939209214289,-1.44476227440427,-1.27295337706792));
#32885=CARTESIAN_POINT('Ctrl Pts',(96.7485432714083,-1.43593657341001,-1.26994416061208));
#32886=CARTESIAN_POINT('Ctrl Pts',(96.8025959574962,-1.42402000981103,-1.26693494415624));
#32887=CARTESIAN_POINT('Ctrl Pts',(96.8557133159405,-1.40912157977184,-1.26392572770041));
#32888=CARTESIAN_POINT('Ctrl Pts',(96.8963502727589,-1.39772367001324,-1.26162355374533));
#32889=CARTESIAN_POINT('Ctrl Pts',(96.9364400149676,-1.38458157295015,-1.25932137979025));
#32890=CARTESIAN_POINT('Ctrl Pts',(96.9758268846356,-1.36976305148684,-1.25701920583518));
#32891=CARTESIAN_POINT('Ctrl Pts',(97.0273258444945,-1.35038759848846,-1.2540090766957));
#32892=CARTESIAN_POINT('Ctrl Pts',(97.0778388018055,-1.32806308923919,-1.25099894755622));
#32893=CARTESIAN_POINT('Ctrl Pts',(97.1270058930076,-1.30291087561076,-1.24798881841674));
#32894=CARTESIAN_POINT('Ctrl Pts',(97.1760856004827,-1.27780336452865,-1.24498403912199));
#32895=CARTESIAN_POINT('Ctrl Pts',(97.2238237223901,-1.24987836102905,-1.24197925982723));
#32896=CARTESIAN_POINT('Ctrl Pts',(97.2698797266185,-1.21930548662905,-1.23897448053247));
#32897=CARTESIAN_POINT('Ctrl Pts',(97.3158901660822,-1.18876285900914,-1.23597267396764));
#32898=CARTESIAN_POINT('Ctrl Pts',(97.3602213466864,-1.15557784048893,-1.23297086740281));
#32899=CARTESIAN_POINT('Ctrl Pts',(97.4025584015194,-1.11996532291928,-1.22996906083797));
#32900=CARTESIAN_POINT('Ctrl Pts',(97.4448702929678,-1.08437397194896,-1.22696903842212));
#32901=CARTESIAN_POINT('Ctrl Pts',(97.485190004498,-1.04635832094007,-1.22396901600626));
#32902=CARTESIAN_POINT('Ctrl Pts',(97.523234565834,-1.00617443871958,-1.22096899359041));
#32903=CARTESIAN_POINT('Ctrl Pts',(97.5612715408454,-0.965998569417716,
-1.21796956939787));
#32904=CARTESIAN_POINT('Ctrl Pts',(97.5970339037676,-0.923655710838852,
-1.21497014520534));
#32905=CARTESIAN_POINT('Ctrl Pts',(97.6302761455861,-0.879438144154546,
-1.2119707210128));
#32906=CARTESIAN_POINT('Ctrl Pts',(97.6635489487699,-0.835179925903617,
-1.20896853928968));
#32907=CARTESIAN_POINT('Ctrl Pts',(97.6942966839872,-0.789043979217203,
-1.20596635756657));
#32908=CARTESIAN_POINT('Ctrl Pts',(97.7223156537142,-0.741353781561064,
-1.20296417584345));
#32909=CARTESIAN_POINT('Ctrl Pts',(97.7503473770328,-0.69364187642226,-1.19996062759616));
#32910=CARTESIAN_POINT('Ctrl Pts',(97.775647617204,-0.644374780652279,-1.19695707934888));
#32911=CARTESIAN_POINT('Ctrl Pts',(97.7980589924109,-0.593900016272528,
-1.19395353110159));
#32912=CARTESIAN_POINT('Ctrl Pts',(97.8205126652406,-0.543329989441457,
-1.19094431417269));
#32913=CARTESIAN_POINT('Ctrl Pts',(97.8400663943914,-0.491548236086386,
-1.18793509724379));
#32914=CARTESIAN_POINT('Ctrl Pts',(97.8566116698041,-0.438920564610642,
-1.1849258803149));
#32915=CARTESIAN_POINT('Ctrl Pts',(97.869269460652,-0.398658311989629,-1.1826237102058));
#32916=CARTESIAN_POINT('Ctrl Pts',(97.880167457635,-0.357901350998972,-1.18032154009671));
#32917=CARTESIAN_POINT('Ctrl Pts',(97.8892773632463,-0.316817073854785,
-1.17801936998761));
#32918=CARTESIAN_POINT('Ctrl Pts',(97.9055044705775,-0.243635308500493,
-1.17391860725207));
#32919=CARTESIAN_POINT('Ctrl Pts',(97.9161139965923,-0.169166208287235,
-1.16981784451653));
#32920=CARTESIAN_POINT('Ctrl Pts',(97.9209501091143,-0.0941386426520588,
-1.16571708178099));
#32921=CARTESIAN_POINT('Ctrl Pts',(97.9229400296052,-0.0632669684386882,
-1.16402973646829));
#32922=CARTESIAN_POINT('Ctrl Pts',(97.9239529862227,-0.0323010019033244,
-1.16234239115559));
#32923=CARTESIAN_POINT('Ctrl Pts',(97.9239803785352,-0.00129284140671581,
-1.16065504584289));
#32924=CARTESIAN_POINT('Ctrl Pts',(97.9239803891076,-0.00128081758231612,
-1.08934495415707));
#32925=CARTESIAN_POINT('Ctrl Pts',(97.923913186341,-0.0780686541499415,
-1.09352478117624));
#32926=CARTESIAN_POINT('Ctrl Pts',(97.9177989441704,-0.154598277700433,
-1.09770460819541));
#32927=CARTESIAN_POINT('Ctrl Pts',(97.9057798266317,-0.230094341487387,
-1.10188443521458));
#32928=CARTESIAN_POINT('Ctrl Pts',(97.9018372523638,-0.254858958145268,
-1.10325552409834));
#32929=CARTESIAN_POINT('Ctrl Pts',(97.8972596717829,-0.279512589571985,
-1.1046266129821));
#32930=CARTESIAN_POINT('Ctrl Pts',(97.8920531495257,-0.304028430140903,
-1.10599770186586));
#32931=CARTESIAN_POINT('Ctrl Pts',(97.8806225864053,-0.357851279488796,
-1.1090078336305));
#32932=CARTESIAN_POINT('Ctrl Pts',(97.8661284184552,-0.411141685375522,
-1.11201796539513));
#32933=CARTESIAN_POINT('Ctrl Pts',(97.8486366398626,-0.463525651423493,
-1.11502809715977));
#32934=CARTESIAN_POINT('Ctrl Pts',(97.8311759487617,-0.515816517384617,
-1.11803287912846));
#32935=CARTESIAN_POINT('Ctrl Pts',(97.8107283854768,-0.567203643637056,
-1.12103766109716));
#32936=CARTESIAN_POINT('Ctrl Pts',(97.7874105676034,-0.617324905381474,
-1.12404244306586));
#32937=CARTESIAN_POINT('Ctrl Pts',(97.7641158186009,-0.667396580971582,
-1.12704425233241));
#32938=CARTESIAN_POINT('Ctrl Pts',(97.7379566618143,-0.716204396420274,
-1.13004606159897));
#32939=CARTESIAN_POINT('Ctrl Pts',(97.7090983230289,-0.763404810512815,
-1.13304787086552));
#32940=CARTESIAN_POINT('Ctrl Pts',(97.6802571362052,-0.81057717102601,-1.13604789600589));
#32941=CARTESIAN_POINT('Ctrl Pts',(97.6487202220611,-0.856143574095053,
-1.13904792114627));
#32942=CARTESIAN_POINT('Ctrl Pts',(97.6146983023442,-0.899785837058556,
-1.14204794628664));
#32943=CARTESIAN_POINT('Ctrl Pts',(97.5806831666032,-0.943419397748199,
-1.14504737322154));
#32944=CARTESIAN_POINT('Ctrl Pts',(97.5441843338644,-0.98512916401779,-1.14804680015645));
#32945=CARTESIAN_POINT('Ctrl Pts',(97.5054539481688,-1.02462855816834,-1.15104622709135));
#32946=CARTESIAN_POINT('Ctrl Pts',(97.4666879555246,-1.06416426625868,-1.15404841156246));
#32947=CARTESIAN_POINT('Ctrl Pts',(97.4256866816569,-1.10148516443139,-1.15705059603356));
#32948=CARTESIAN_POINT('Ctrl Pts',(97.3827393862181,-1.13634133342247,-1.16005278050466));
#32949=CARTESIAN_POINT('Ctrl Pts',(97.3397725420696,-1.17121336821187,-1.16305633150727));
#32950=CARTESIAN_POINT('Ctrl Pts',(97.2948583396211,-1.20361812786644,-1.16605988250989));
#32951=CARTESIAN_POINT('Ctrl Pts',(97.2483167590414,-1.23334787765881,-1.1690634335125));
#32952=CARTESIAN_POINT('Ctrl Pts',(97.2016873396489,-1.26313373697509,-1.17207265317422));
#32953=CARTESIAN_POINT('Ctrl Pts',(97.1534248681767,-1.29023424186537,-1.17508187283594));
#32954=CARTESIAN_POINT('Ctrl Pts',(97.1038747357487,-1.31448723307444,-1.17809109249765));
#32955=CARTESIAN_POINT('Ctrl Pts',(97.0659673141667,-1.33304153994176,-1.18039324090291));
#32956=CARTESIAN_POINT('Ctrl Pts',(97.0273068012296,-1.34993021255995,-1.18269538930817));
#32957=CARTESIAN_POINT('Ctrl Pts',(96.9880544450365,-1.36510016368348,-1.18499753771342));
#32958=CARTESIAN_POINT('Ctrl Pts',(96.9367307977058,-1.38493533530114,-1.18800766664105));
#32959=CARTESIAN_POINT('Ctrl Pts',(96.8841791451047,-1.40191373683725,-1.19101779556867));
#32960=CARTESIAN_POINT('Ctrl Pts',(96.8307487774288,-1.41588628980505,-1.1940279244963));
#32961=CARTESIAN_POINT('Ctrl Pts',(96.7774133701589,-1.42983400971704,-1.19703270359989));
#32962=CARTESIAN_POINT('Ctrl Pts',(96.7232028538547,-1.4407863501921,-1.20003748270348));
#32963=CARTESIAN_POINT('Ctrl Pts',(96.6684842364518,-1.44864311776547,-1.20304226180707));
#32964=CARTESIAN_POINT('Ctrl Pts',(96.6138197538003,-1.45649211240562,-1.20604406819356));
#32965=CARTESIAN_POINT('Ctrl Pts',(96.5586486860187,-1.46125152620207,-1.20904587458005));
#32966=CARTESIAN_POINT('Ctrl Pts',(96.5033490361798,-1.46287203033998,-1.21204768096654));
#32967=CARTESIAN_POINT('Ctrl Pts',(96.4480822539129,-1.46449157132466,-1.21504770321718));
#32968=CARTESIAN_POINT('Ctrl Pts',(96.3926875679001,-1.46297588500113,-1.21804772546782));
#32969=CARTESIAN_POINT('Ctrl Pts',(96.3375466016096,-1.45832760245764,-1.22104774771846));
#32970=CARTESIAN_POINT('Ctrl Pts',(96.2824166305276,-1.45368024679009,-1.22404717175923));
#32971=CARTESIAN_POINT('Ctrl Pts',(96.2275408046486,-1.44590157975849,-1.22704659580001));
#32972=CARTESIAN_POINT('Ctrl Pts',(96.1732969104484,-1.43504619356653,-1.23004601984078));
#32973=CARTESIAN_POINT('Ctrl Pts',(96.1190031465407,-1.42418082735853,-1.23304820143431));
#32974=CARTESIAN_POINT('Ctrl Pts',(96.0653429939818,-1.41023319464078,-1.23605038302783));
#32975=CARTESIAN_POINT('Ctrl Pts',(96.0126838166709,-1.39330900297137,-1.23905256462135));
#32976=CARTESIAN_POINT('Ctrl Pts',(95.9600006698984,-1.37637710773,-1.24205611275116));
#32977=CARTESIAN_POINT('Ctrl Pts',(95.9083199002972,-1.35646614288436,-1.24505966088096));
#32978=CARTESIAN_POINT('Ctrl Pts',(95.8579903266545,-1.33373059471938,-1.24806320901076));
#32979=CARTESIAN_POINT('Ctrl Pts',(95.8075657642202,-1.3109521369469,-1.25107242584362));
#32980=CARTESIAN_POINT('Ctrl Pts',(95.7584979614032,-1.2853386914663,-1.25408164267648));
#32981=CARTESIAN_POINT('Ctrl Pts',(95.7111114507522,-1.25709092918178,-1.25709085950934));
#32982=CARTESIAN_POINT('Ctrl Pts',(95.6748588729945,-1.23548026014044,-1.25939303085989));
#32983=CARTESIAN_POINT('Ctrl Pts',(95.6395898415557,-1.21232872962806,-1.26169520221044));
#32984=CARTESIAN_POINT('Ctrl Pts',(95.605436927778,-1.18774238401507,-1.26399737356099));
#32985=CARTESIAN_POINT('Ctrl Pts',(95.5607814193552,-1.15559532415497,-1.26700750127086));
#32986=CARTESIAN_POINT('Ctrl Pts',(95.5178475527745,-1.12085885059954,-1.27001762898074));
#32987=CARTESIAN_POINT('Ctrl Pts',(95.476951036042,-1.0837440468957,-1.27302775669062));
#32988=CARTESIAN_POINT('Ctrl Pts',(95.4361272043169,-1.04669520699502,-1.27603253452789));
#32989=CARTESIAN_POINT('Ctrl Pts',(95.3973339245293,-1.00727677746951,-1.27903731236516));
#32990=CARTESIAN_POINT('Ctrl Pts',(95.3608556431135,-0.965741391566654,
-1.28204209020243));
#32991=CARTESIAN_POINT('Ctrl Pts',(95.3244134511082,-0.924247098268254,
-1.28504389529383));
#32992=CARTESIAN_POINT('Ctrl Pts',(95.2902820672444,-0.880640392334413,
-1.28804570038522));
#32993=CARTESIAN_POINT('Ctrl Pts',(95.2587093451839,-0.835210908019247,
-1.29104750547661));
#32994=CARTESIAN_POINT('Ctrl Pts',(95.2271553887851,-0.789808425314378,
-1.29404752640575));
#32995=CARTESIAN_POINT('Ctrl Pts',(95.1981573807067,-0.742585744386444,
-1.29704754733489));
#32996=CARTESIAN_POINT('Ctrl Pts',(95.1719216349935,-0.693863922394019,
-1.30004756826402));
#32997=CARTESIAN_POINT('Ctrl Pts',(95.1456911209483,-0.645151816016436,
-1.30304699095921));
#32998=CARTESIAN_POINT('Ctrl Pts',(95.1222220256048,-0.594941626990456,
-1.3060464136544));
#32999=CARTESIAN_POINT('Ctrl Pts',(95.1016750476782,-0.543579590276448,
-1.30904583634959));
#33000=CARTESIAN_POINT('Ctrl Pts',(95.0811091798411,-0.492170333757866,
-1.31204801657082));
#33001=CARTESIAN_POINT('Ctrl Pts',(95.0634709931864,-0.439607605289542,
-1.31505019679204));
#33002=CARTESIAN_POINT('Ctrl Pts',(95.0488726811017,-0.386256839903434,
-1.31805237701327));
#33003=CARTESIAN_POINT('Ctrl Pts',(95.0342677242209,-0.332881790548091,
-1.32105592375382));
#33004=CARTESIAN_POINT('Ctrl Pts',(95.0227055106196,-0.278718506621066,
-1.32405947049438));
#33005=CARTESIAN_POINT('Ctrl Pts',(95.0142472472189,-0.224143543657761,
-1.32706301723493));
#33006=CARTESIAN_POINT('Ctrl Pts',(95.0057730202597,-0.169465579573552,
-1.33007223266795));
#33007=CARTESIAN_POINT('Ctrl Pts',(95.0004144973922,-0.11437491124949,-1.33308144810096));
#33008=CARTESIAN_POINT('Ctrl Pts',(94.9981809347718,-0.0592529889609269,
-1.33609066353397));
#33009=CARTESIAN_POINT('Ctrl Pts',(94.9964721612787,-0.0170822976898624,
-1.33839284549217));
#33010=CARTESIAN_POINT('Ctrl Pts',(94.9965913237324,0.0251065685188833,
-1.34069502745036));
#33011=CARTESIAN_POINT('Ctrl Pts',(94.998522041667,0.0671446318229337,-1.34299720940855));
#33012=CARTESIAN_POINT('Ctrl Pts',(95.0010464773481,0.12210987820601,-1.34600733852977));
#33013=CARTESIAN_POINT('Ctrl Pts',(95.0066803182552,0.177048047429061,-1.34901746765098));
#33014=CARTESIAN_POINT('Ctrl Pts',(95.0154192774912,0.231579389990714,-1.35202759677219));
#33015=CARTESIAN_POINT('Ctrl Pts',(95.0241427051611,0.286013815159483,-1.35503237605507));
#33016=CARTESIAN_POINT('Ctrl Pts',(95.0359602164494,0.340042331308619,-1.35803715533795));
#33017=CARTESIAN_POINT('Ctrl Pts',(95.0508156442684,0.393288668803274,-1.36104193462083));
#33018=CARTESIAN_POINT('Ctrl Pts',(95.0656563751288,0.446482327962045,-1.3640437411777));
#33019=CARTESIAN_POINT('Ctrl Pts',(95.0835289275258,0.498894835207535,-1.36704554773457));
#33020=CARTESIAN_POINT('Ctrl Pts',(95.1043261508944,0.550160351179653,-1.37004735429144));
#33021=CARTESIAN_POINT('Ctrl Pts',(95.1251110132854,0.60139539712783,-1.37304737670324));
#33022=CARTESIAN_POINT('Ctrl Pts',(95.1488169030918,0.651484314618733,-1.37604739911504));
#33023=CARTESIAN_POINT('Ctrl Pts',(95.1752876551499,0.700078885526163,-1.37904742152684));
#33024=CARTESIAN_POINT('Ctrl Pts',(95.2017531288081,0.748663766433972,-1.38204684571922));
#33025=CARTESIAN_POINT('Ctrl Pts',(95.230982117318,0.795754429021658,-1.3850462699116));
#33026=CARTESIAN_POINT('Ctrl Pts',(95.2627724444077,0.841027102206065,-1.38804569410398));
#33027=CARTESIAN_POINT('Ctrl Pts',(95.2945919981039,0.886341397063631,-1.39104787583296));
#33028=CARTESIAN_POINT('Ctrl Pts',(95.328977290781,0.929833930189806,-1.39405005756194));
#33029=CARTESIAN_POINT('Ctrl Pts',(95.3656835624845,0.971211064195376,-1.39705223929092));
#33030=CARTESIAN_POINT('Ctrl Pts',(95.4024065420808,1.01260703216817,-1.40005578754742));
#33031=CARTESIAN_POINT('Ctrl Pts',(95.4414522337086,1.05188530638393,-1.40305933580393));
#33032=CARTESIAN_POINT('Ctrl Pts',(95.4825387048994,1.0887888758042,-1.40606288406043));
#33033=CARTESIAN_POINT('Ctrl Pts',(95.5237027198233,1.12576209444113,-1.4090721010039));
#33034=CARTESIAN_POINT('Ctrl Pts',(95.5669147952189,1.16035132425278,-1.41208131794738));
#33035=CARTESIAN_POINT('Ctrl Pts',(95.6118605134582,1.19234038990616,-1.41509053489085));
#33036=CARTESIAN_POINT('Ctrl Pts',(95.6462457676871,1.2168132918449,-1.4173927050126));
#33037=CARTESIAN_POINT('Ctrl Pts',(95.6816450099557,1.23976519443698,-1.41969487513436));
#33038=CARTESIAN_POINT('Ctrl Pts',(95.717907768993,1.26111748916484,-1.42199704525611));
#33039=CARTESIAN_POINT('Ctrl Pts',(95.765321975675,1.28903599680838,-1.42500717390786));
#33040=CARTESIAN_POINT('Ctrl Pts',(95.8144124710483,1.31433550009617,-1.42801730255961));
#33041=CARTESIAN_POINT('Ctrl Pts',(95.8648588624843,1.33681209575889,-1.43102743121136));
#33042=CARTESIAN_POINT('Ctrl Pts',(95.9152155965013,1.35924874419255,-1.43403221001829));
#33043=CARTESIAN_POINT('Ctrl Pts',(95.966922965802,1.37887222827389,-1.43703698882523));
#33044=CARTESIAN_POINT('Ctrl Pts',(96.0196351450947,1.39552399716749,-1.44004176763216));
#33045=CARTESIAN_POINT('Ctrl Pts',(96.0722951744402,1.41215929190123,-1.44304357370949));
#33046=CARTESIAN_POINT('Ctrl Pts',(96.1259575434175,1.42582853718202,-1.44604537978682));
#33047=CARTESIAN_POINT('Ctrl Pts',(96.1802573051872,1.43642158126537,-1.44904718586414));
#33048=CARTESIAN_POINT('Ctrl Pts',(96.2345247934531,1.44700832928704,-1.45204720779368));
#33049=CARTESIAN_POINT('Ctrl Pts',(96.2894284063168,1.45452239913185,-1.45504722972322));
#33050=CARTESIAN_POINT('Ctrl Pts',(96.3445911738028,1.45890431827142,-1.45804725165275));
#33051=CARTESIAN_POINT('Ctrl Pts',(96.3997429415224,1.46328536363165,-1.46104667536103));
#33052=CARTESIAN_POINT('Ctrl Pts',(96.4551532350738,1.46453545685652,-1.4640460990693));
#33053=CARTESIAN_POINT('Ctrl Pts',(96.5104404192415,1.46264701872695,-1.46704552277757));
#33054=CARTESIAN_POINT('Ctrl Pts',(96.5657784320038,1.4607568444508,-1.47004770402349));
#33055=CARTESIAN_POINT('Ctrl Pts',(96.6209925803185,1.45572239217891,-1.4730498852694));
#33056=CARTESIAN_POINT('Ctrl Pts',(96.6757031991877,1.44758821260485,-1.47605206651532));
#33057=CARTESIAN_POINT('Ctrl Pts',(96.7304387211361,1.43945033052985,-1.47905561428859));
#33058=CARTESIAN_POINT('Ctrl Pts',(96.7846697387265,1.42821001593459,-1.48205916206186));
#33059=CARTESIAN_POINT('Ctrl Pts',(96.8380269515981,1.41396296498808,-1.48506270983512));
#33060=CARTESIAN_POINT('Ctrl Pts',(96.8914848672617,1.39968902512196,-1.48807192630116));
#33061=CARTESIAN_POINT('Ctrl Pts',(96.9440651808393,1.38239717817992,-1.49108114276719));
#33062=CARTESIAN_POINT('Ctrl Pts',(96.9954150432075,1.36223263999644,-1.49409035923323));
#33063=CARTESIAN_POINT('Ctrl Pts',(97.0346997929637,1.34680594165778,-1.49639253319004));
#33064=CARTESIAN_POINT('Ctrl Pts',(97.0732647016424,1.32969892729858,-1.49869470714686));
#33065=CARTESIAN_POINT('Ctrl Pts',(97.1109617148245,1.31099466972333,-1.50099688110367));
#33066=CARTESIAN_POINT('Ctrl Pts',(97.160251150663,1.28653855965416,-1.50400700965113));
#33067=CARTESIAN_POINT('Ctrl Pts',(97.2082630176524,1.25924749917942,-1.50701713819859));
#33068=CARTESIAN_POINT('Ctrl Pts',(97.2546514800504,1.22927841375647,-1.51002726674605));
#33069=CARTESIAN_POINT('Ctrl Pts',(97.300957497026,1.19936259187746,-1.51303204544342));
#33070=CARTESIAN_POINT('Ctrl Pts',(97.3456453951994,1.16677847478941,-1.51603682414079));
#33071=CARTESIAN_POINT('Ctrl Pts',(97.3883934264001,1.13172906888357,-1.51904160283817));
#33072=CARTESIAN_POINT('Ctrl Pts',(97.4310991654771,1.09671433858191,-1.52204340880279));
#33073=CARTESIAN_POINT('Ctrl Pts',(97.4718684329952,1.05923948419602,-1.52504521476742));
#33074=CARTESIAN_POINT('Ctrl Pts',(97.5104095683821,1.01954997200432,-1.52804702073204));
#33075=CARTESIAN_POINT('Ctrl Pts',(97.548927796494,0.97988404963583,-1.53104704254594));
#33076=CARTESIAN_POINT('Ctrl Pts',(97.5852201501666,0.938006456577654,-1.53404706435984));
#33077=CARTESIAN_POINT('Ctrl Pts',(97.6190308446368,0.89420041973649,-1.53704708617374));
#33078=CARTESIAN_POINT('Ctrl Pts',(97.6528347970331,0.850403118105972,-1.54004650976364));
#33079=CARTESIAN_POINT('Ctrl Pts',(97.6841577504972,0.804678554218957,-1.54304593335354));
#33080=CARTESIAN_POINT('Ctrl Pts',(97.7127848332375,0.757342216549942,-1.54604535694344));
#33081=CARTESIAN_POINT('Ctrl Pts',(97.7414382344224,0.709962359993977,-1.54904753806766));
#33082=CARTESIAN_POINT('Ctrl Pts',(97.7673905393589,0.660968222103689,-1.55204971919189));
#33083=CARTESIAN_POINT('Ctrl Pts',(97.7904716129776,0.610702124826206,-1.55505190031612));
#33084=CARTESIAN_POINT('Ctrl Pts',(97.8135631925819,0.560413147551788,-1.55805544796568));
#33085=CARTESIAN_POINT('Ctrl Pts',(97.8337807424909,0.508851549286685,-1.56105899561523));
#33086=CARTESIAN_POINT('Ctrl Pts',(97.8510026265431,0.456378917005767,-1.56406254326478));
#33087=CARTESIAN_POINT('Ctrl Pts',(97.8682570140046,0.403807251457771,-1.5670717596053));
#33088=CARTESIAN_POINT('Ctrl Pts',(97.8825043049642,0.350321628651735,-1.57008097594582));
#33089=CARTESIAN_POINT('Ctrl Pts',(97.8936733262038,0.29629691456199,-1.57309019228634));
#33090=CARTESIAN_POINT('Ctrl Pts',(97.9022180891303,0.254965775138703,-1.57539236717464));
#33091=CARTESIAN_POINT('Ctrl Pts',(97.9089622223474,0.213319403591485,-1.57769454206294));
#33092=CARTESIAN_POINT('Ctrl Pts',(97.9138944051945,0.171527190352026,-1.57999671695124));
#33093=CARTESIAN_POINT('Ctrl Pts',(97.9205702975477,0.114959880210447,-1.58311279601985));
#33094=CARTESIAN_POINT('Ctrl Pts',(97.923944606945,0.0579954345134518,-1.58622887508846));
#33095=CARTESIAN_POINT('Ctrl Pts',(97.9239806575935,0.000924464996447671,
-1.58934495415707));
#33096=CARTESIAN_POINT('Origin',(96.460480949577,-8.32667268468867E-16,
1.18130019239114E-14));
#33097=CARTESIAN_POINT('',(97.9239808736879,0.000471303870065604,-2.16065504579701));
#33098=CARTESIAN_POINT('',(97.9239808936025,0.000404768228816884,-2.08934495411702));
#33099=CARTESIAN_POINT('',(97.923980949577,-1.01189432752408E-15,1.19922289829666E-14));
#33100=CARTESIAN_POINT('Ctrl Pts',(97.9239808736879,0.000471303870068238,
-2.16065504579701));
#33101=CARTESIAN_POINT('Ctrl Pts',(97.9239615958962,0.0603329949048461,
-2.15741638815146));
#33102=CARTESIAN_POINT('Ctrl Pts',(97.92026528758,0.120088518536624,-2.1541777305059));
#33103=CARTESIAN_POINT('Ctrl Pts',(97.912956108285,0.179299089055256,-2.15093907286035));
#33104=CARTESIAN_POINT('Ctrl Pts',(97.905627399874,0.238667862028564,-2.14769176196953));
#33105=CARTESIAN_POINT('Ctrl Pts',(97.8946666302688,0.297488396255375,-2.1444444510787));
#33106=CARTESIAN_POINT('Ctrl Pts',(97.8801887931385,0.355333489738872,-2.14119714018788));
#33107=CARTESIAN_POINT('Ctrl Pts',(97.8656522053234,0.413413317100202,-2.13793665179431));
#33108=CARTESIAN_POINT('Ctrl Pts',(97.8475701160377,0.470509414487508,-2.13467616340075));
#33109=CARTESIAN_POINT('Ctrl Pts',(97.8261072647801,0.526210050478789,-2.13141567500718));
#33110=CARTESIAN_POINT('Ctrl Pts',(97.8142621712294,0.556950572147068,-2.12961625005758));
#33111=CARTESIAN_POINT('Ctrl Pts',(97.801388201685,0.587266460099237,-2.12781682510797));
#33112=CARTESIAN_POINT('Ctrl Pts',(97.7875190028352,0.617091772109138,-2.12601740015837));
#33113=CARTESIAN_POINT('Ctrl Pts',(97.7643182169546,0.666984392818874,-2.1230072714973));
#33114=CARTESIAN_POINT('Ctrl Pts',(97.7382510539732,0.715671604914073,-2.11999714283623));
#33115=CARTESIAN_POINT('Ctrl Pts',(97.7094656361879,0.76280371171842,-2.11698701417517));
#33116=CARTESIAN_POINT('Ctrl Pts',(97.6807313782009,0.809852051488635,-2.11398223536089));
#33117=CARTESIAN_POINT('Ctrl Pts',(97.6492887258075,0.855350323806215,-2.11097745654661));
#33118=CARTESIAN_POINT('Ctrl Pts',(97.61533247712,0.898971745569159,-2.10797267773233));
#33119=CARTESIAN_POINT('Ctrl Pts',(97.5814098225148,0.942550011162192,-2.10497087164888));
#33120=CARTESIAN_POINT('Ctrl Pts',(97.5449788206278,0.984254689807881,-2.10196906556542));
#33121=CARTESIAN_POINT('Ctrl Pts',(97.5062774773565,1.02378800172905,-2.09896725948197));
#33122=CARTESIAN_POINT('Ctrl Pts',(97.4675991365583,1.0632978166895,-2.09596723754753));
#33123=CARTESIAN_POINT('Ctrl Pts',(97.4266534976736,1.10063844628959,-2.0929672156131));
#33124=CARTESIAN_POINT('Ctrl Pts',(97.3837172231288,1.13554701936915,-2.08996719367866));
#33125=CARTESIAN_POINT('Ctrl Pts',(97.3407895103367,1.17044863146824,-2.08696776996673));
#33126=CARTESIAN_POINT('Ctrl Pts',(97.2958723597416,1.20291881719933,-2.0839683462548));
#33127=CARTESIAN_POINT('Ctrl Pts',(97.2492757204877,1.2327347887457,-2.08096892254287));
#33128=CARTESIAN_POINT('Ctrl Pts',(97.202636242373,1.26257817175942,-2.07796674129527));
#33129=CARTESIAN_POINT('Ctrl Pts',(97.1543146365936,1.28976218020006,-2.07496456004767));
#33130=CARTESIAN_POINT('Ctrl Pts',(97.1046488094327,1.31410806950148,-2.07196237880007));
#33131=CARTESIAN_POINT('Ctrl Pts',(97.0549603754898,1.3384650405113,-2.0689588310262));
#33132=CARTESIAN_POINT('Ctrl Pts',(97.0039269879474,1.359981111644,-2.06595528325234));
#33133=CARTESIAN_POINT('Ctrl Pts',(96.9519070394269,1.37852553411781,-2.06295173547847));
#33134=CARTESIAN_POINT('Ctrl Pts',(96.8997889120081,1.39710495606818,-2.05994251901365));
#33135=CARTESIAN_POINT('Ctrl Pts',(96.8466810120016,1.41270137636166,-2.05693330254884));
#33136=CARTESIAN_POINT('Ctrl Pts',(96.7929562839649,1.42523415691025,-2.05392408608402));
#33137=CARTESIAN_POINT('Ctrl Pts',(96.7518546651787,1.43482224766962,-2.05162191215962));
#33138=CARTESIAN_POINT('Ctrl Pts',(96.710392342561,1.44261826540517,-2.04931973823521));
#33139=CARTESIAN_POINT('Ctrl Pts',(96.6687383655387,1.44860660591374,-2.04701756431081));
#33140=CARTESIAN_POINT('Ctrl Pts',(96.6142751346129,1.45643645543345,-2.04400743564988));
#33141=CARTESIAN_POINT('Ctrl Pts',(96.559255288647,1.46120700645385,-2.04099730698895));
#33142=CARTESIAN_POINT('Ctrl Pts',(96.5040526414606,1.46285124249406,-2.03798717832802));
#33143=CARTESIAN_POINT('Ctrl Pts',(96.4489481049327,1.46449255626352,-2.03498239951388));
#33144=CARTESIAN_POINT('Ctrl Pts',(96.3936619355416,1.463018566056,-2.03197762069975));
#33145=CARTESIAN_POINT('Ctrl Pts',(96.3385742598537,1.45841386752894,-2.02897284188562));
#33146=CARTESIAN_POINT('Ctrl Pts',(96.2835410842944,1.45381372458819,-2.02597103580231));
#33147=CARTESIAN_POINT('Ctrl Pts',(96.228706537119,1.4460890527391,-2.02296922971901));
#33148=CARTESIAN_POINT('Ctrl Pts',(96.1744500623932,1.43527648262515,-2.0199674236357));
#33149=CARTESIAN_POINT('Ctrl Pts',(96.1202258354654,1.42447033905438,-2.01696740170142));
#33150=CARTESIAN_POINT('Ctrl Pts',(96.066579516882,1.41058003795132,-2.01396737976714));
#33151=CARTESIAN_POINT('Ctrl Pts',(96.0138824355779,1.39369365977383,-2.01096735783286));
#33152=CARTESIAN_POINT('Ctrl Pts',(95.9611958623903,1.37681064884223,-2.00796793412108));
#33153=CARTESIAN_POINT('Ctrl Pts',(95.9094586532168,1.35693290838663,-2.00496851040931));
#33154=CARTESIAN_POINT('Ctrl Pts',(95.8590267538452,1.33419829876846,-2.00196908669753));
#33155=CARTESIAN_POINT('Ctrl Pts',(95.8085484896468,1.31144278796962,-1.99896690545009));
#33156=CARTESIAN_POINT('Ctrl Pts',(95.759378415272,1.28582537815373,-1.99596472420265));
#33157=CARTESIAN_POINT('Ctrl Pts',(95.7118508647721,1.25753140959782,-1.9929625429552));
#33158=CARTESIAN_POINT('Ctrl Pts',(95.6643016807864,1.22922456225549,-1.9899589951815));
#33159=CARTESIAN_POINT('Ctrl Pts',(95.6183969495375,1.19823902353665,-1.9869554474078));
#33160=CARTESIAN_POINT('Ctrl Pts',(95.5744420009703,1.16480351628584,-1.98395189963409));
#33161=CARTESIAN_POINT('Ctrl Pts',(95.5304040948349,1.13130490514201,-1.98094268316944));
#33162=CARTESIAN_POINT('Ctrl Pts',(95.4883237250118,1.09534743242324,-1.97793346670479));
#33163=CARTESIAN_POINT('Ctrl Pts',(95.4484722035119,1.05719938889871,-1.97492425024013));
#33164=CARTESIAN_POINT('Ctrl Pts',(95.417984156284,1.02801457213745,-1.9726220763145));
#33165=CARTESIAN_POINT('Ctrl Pts',(95.3887999312872,0.997548474542972,-1.97031990238887));
#33166=CARTESIAN_POINT('Ctrl Pts',(95.3610249654051,0.96593415348494,-1.96801772846325));
#33167=CARTESIAN_POINT('Ctrl Pts',(95.3247087601124,0.924597930837241,-1.96500759980071));
#33168=CARTESIAN_POINT('Ctrl Pts',(95.2906506673778,0.881123939421362,-1.96199747113817));
#33169=CARTESIAN_POINT('Ctrl Pts',(95.2591110657112,0.83578864082984,-1.95898734247562));
#33170=CARTESIAN_POINT('Ctrl Pts',(95.2276275188036,0.790533915837978,-1.95598256365988));
#33171=CARTESIAN_POINT('Ctrl Pts',(95.1986538793383,0.743424878570124,-1.95297778484413));
#33172=CARTESIAN_POINT('Ctrl Pts',(95.1724107485305,0.694771478384037,-1.94997300602838));
#33173=CARTESIAN_POINT('Ctrl Pts',(95.1461935809528,0.646166212676844,-1.94697119994346));
#33174=CARTESIAN_POINT('Ctrl Pts',(95.1227018201985,0.596020073256171,-1.94396939385854));
#33175=CARTESIAN_POINT('Ctrl Pts',(95.1021121138656,0.544670869579148,-1.94096758777362));
#33176=CARTESIAN_POINT('Ctrl Pts',(95.0815346452002,0.49335218573886,-1.93796756583772));
#33177=CARTESIAN_POINT('Ctrl Pts',(95.0638560083256,0.440832344121254,-1.93496754390182));
#33178=CARTESIAN_POINT('Ctrl Pts',(95.0492053261603,0.387470469519647,-1.93196752196592));
#33179=CARTESIAN_POINT('Ctrl Pts',(95.0345575654296,0.334119235598484,-1.92896809825254));
#33180=CARTESIAN_POINT('Ctrl Pts',(95.0229367000457,0.279926811133344,-1.92596867453915));
#33181=CARTESIAN_POINT('Ctrl Pts',(95.0144217556271,0.225266636661854,-1.92296925082577));
#33182=CARTESIAN_POINT('Ctrl Pts',(95.0058989829504,0.170556210077254,-1.91996706957673));
#33183=CARTESIAN_POINT('Ctrl Pts',(95.0004879175099,0.115377697289208,-1.9169648883277));
#33184=CARTESIAN_POINT('Ctrl Pts',(94.9982160106488,0.0601123812637398,
-1.91396270707866));
#33185=CARTESIAN_POINT('Ctrl Pts',(94.995943069666,0.00482190969338436,
-1.91095915930338));
#33186=CARTESIAN_POINT('Ctrl Pts',(94.9968121273256,-0.0505549149049093,
-1.90795561152809));
#33187=CARTESIAN_POINT('Ctrl Pts',(95.0007984531729,-0.105637397220232,
-1.9049520637528));
#33188=CARTESIAN_POINT('Ctrl Pts',(95.0047923025393,-0.160823838450338,
-1.9019428472866));
#33189=CARTESIAN_POINT('Ctrl Pts',(95.0119151048094,-0.215714302647041,
-1.8989336308204));
#33190=CARTESIAN_POINT('Ctrl Pts',(95.0220904030614,-0.269934965675806,
-1.89592441435419));
#33191=CARTESIAN_POINT('Ctrl Pts',(95.0298749232028,-0.311415994828604,
-1.89362224044135));
#33192=CARTESIAN_POINT('Ctrl Pts',(95.0394449538539,-0.352505124594627,
-1.89132006652851));
#33193=CARTESIAN_POINT('Ctrl Pts',(95.0507466661871,-0.393041346724551,
-1.88901789261568));
#33194=CARTESIAN_POINT('Ctrl Pts',(95.0655238331106,-0.446043095769737,
-1.88600776395604));
#33195=CARTESIAN_POINT('Ctrl Pts',(95.0833252627432,-0.49832168324049,-1.8829976352964));
#33196=CARTESIAN_POINT('Ctrl Pts',(95.1040616808569,-0.549507977598812,
-1.87998750663677));
#33197=CARTESIAN_POINT('Ctrl Pts',(95.1247612445128,-0.600603299489543,
-1.87698272782391));
#33198=CARTESIAN_POINT('Ctrl Pts',(95.1483852481736,-0.65060969529963,-1.87397794901105));
#33199=CARTESIAN_POINT('Ctrl Pts',(95.1747946365492,-0.699173050462454,
-1.87097317019819));
#33200=CARTESIAN_POINT('Ctrl Pts',(95.2011778972104,-0.747688360231163,
-1.86797136411614));
#33201=CARTESIAN_POINT('Ctrl Pts',(95.2303408326612,-0.794762995788238,
-1.8649695580341));
#33202=CARTESIAN_POINT('Ctrl Pts',(95.2620970379445,-0.840064432255227,
-1.86196775195205));
#33203=CARTESIAN_POINT('Ctrl Pts',(95.2938343686567,-0.885338943427676,
-1.85896773001902));
#33204=CARTESIAN_POINT('Ctrl Pts',(95.3281616116412,-0.928841912857284,
-1.85596770808598));
#33205=CARTESIAN_POINT('Ctrl Pts',(95.3648485424746,-0.970268972247914,
-1.85296768615294));
#33206=CARTESIAN_POINT('Ctrl Pts',(95.4015281577124,-1.0116877708327,-1.84996826244239));
#33207=CARTESIAN_POINT('Ctrl Pts',(95.4405661764015,-1.0510310863171,-1.84696883873185));
#33208=CARTESIAN_POINT('Ctrl Pts',(95.4816930113293,-1.08802868617554,-1.8439694150213));
#33209=CARTESIAN_POINT('Ctrl Pts',(95.5228576564256,-1.12506029996881,-1.84096723377505));
#33210=CARTESIAN_POINT('Ctrl Pts',(95.5661145609304,-1.15974153567516,-1.8379650525288));
#33211=CARTESIAN_POINT('Ctrl Pts',(95.611159389405,-1.19184107054045,-1.83496287128255));
#33212=CARTESIAN_POINT('Ctrl Pts',(95.6562247212858,-1.22395521640164,-1.83195932351002));
#33213=CARTESIAN_POINT('Ctrl Pts',(95.7030791518731,-1.25348503679986,-1.82895577573749));
#33214=CARTESIAN_POINT('Ctrl Pts',(95.7513903259753,-1.28024323373342,-1.82595222796496));
#33215=CARTESIAN_POINT('Ctrl Pts',(95.7997926792891,-1.30705193226092,-1.82294301150144));
#33216=CARTESIAN_POINT('Ctrl Pts',(95.8496567914534,-1.33107832783827,-1.81993379503791));
#33217=CARTESIAN_POINT('Ctrl Pts',(95.9006277989334,-1.35218219915604,-1.81692457857439));
#33218=CARTESIAN_POINT('Ctrl Pts',(95.9396227088394,-1.36832752571304,-1.81462240463897));
#33219=CARTESIAN_POINT('Ctrl Pts',(95.9792649884082,-1.38276330684499,-1.81232023070354));
#33220=CARTESIAN_POINT('Ctrl Pts',(96.0193903770325,-1.39544665136734,-1.81001805676812));
#33221=CARTESIAN_POINT('Ctrl Pts',(96.071854954282,-1.41203032398187,-1.80700792810848));
#33222=CARTESIAN_POINT('Ctrl Pts',(96.1253663095231,-1.42568596254127,-1.80399779944884));
#33223=CARTESIAN_POINT('Ctrl Pts',(96.1795665060706,-1.43628664459066,-1.8009876707892));
#33224=CARTESIAN_POINT('Ctrl Pts',(96.2336703735963,-1.44686848624097,-1.79798289197639));
#33225=CARTESIAN_POINT('Ctrl Pts',(96.2884601387621,-1.45440604574688,-1.79497811316358));
#33226=CARTESIAN_POINT('Ctrl Pts',(96.3435632418238,-1.45882229884717,-1.79197333435077));
#33227=CARTESIAN_POINT('Ctrl Pts',(96.3986118294937,-1.46323418279665,-1.78897152826881));
#33228=CARTESIAN_POINT('Ctrl Pts',(96.4539726171324,-1.46453083556758,-1.78596972218684));
#33229=CARTESIAN_POINT('Ctrl Pts',(96.509265255268,-1.46268668603985,-1.78296791610488));
#33230=CARTESIAN_POINT('Ctrl Pts',(96.5645250297528,-1.46084363259812,-1.77996789417195));
#33231=CARTESIAN_POINT('Ctrl Pts',(96.6197162082497,-1.45586349447287,-1.77696787223902));
#33232=CARTESIAN_POINT('Ctrl Pts',(96.6744580803983,-1.44777278517228,-1.77396785030609));
#33233=CARTESIAN_POINT('Ctrl Pts',(96.7291890366864,-1.43968368920807,-1.77096842659568));
#33234=CARTESIAN_POINT('Ctrl Pts',(96.7834703424089,-1.42848533106372,-1.76796900288527));
#33235=CARTESIAN_POINT('Ctrl Pts',(96.8369283691581,-1.41425584329382,-1.76496957917486));
#33236=CARTESIAN_POINT('Ctrl Pts',(96.8904355428201,-1.40001327357093,-1.7619673979288));
#33237=CARTESIAN_POINT('Ctrl Pts',(96.9431174139069,-1.38273414292471,-1.75896521668273));
#33238=CARTESIAN_POINT('Ctrl Pts',(96.9946139556971,-1.36254694663086,-1.75596303543666));
#33239=CARTESIAN_POINT('Ctrl Pts',(97.04613393757,-1.34235056157342,-1.75295948766434));
#33240=CARTESIAN_POINT('Ctrl Pts',(97.0964670338264,-1.31924369291165,-1.74995593989202));
#33241=CARTESIAN_POINT('Ctrl Pts',(97.1452747797773,-1.29340235816995,-1.74695239211969));
#33242=CARTESIAN_POINT('Ctrl Pts',(97.1941746421349,-1.26751225225774,-1.74394317565641));
#33243=CARTESIAN_POINT('Ctrl Pts',(97.2415429501902,-1.23887764455822,-1.74093395919313));
#33244=CARTESIAN_POINT('Ctrl Pts',(97.2870683687802,-1.20771912645907,-1.73792474272985));
#33245=CARTESIAN_POINT('Ctrl Pts',(97.3218971800013,-1.1838815829852,-1.73562256879342));
#33246=CARTESIAN_POINT('Ctrl Pts',(97.3556479211617,-1.15856776108528,-1.73332039485699));
#33247=CARTESIAN_POINT('Ctrl Pts',(97.3881949183888,-1.13189179786385,-1.73101822092056));
#33248=CARTESIAN_POINT('Ctrl Pts',(97.4301821350619,-1.09747850191746,-1.72804830405806));
#33249=CARTESIAN_POINT('Ctrl Pts',(97.4703512820927,-1.06064408240767,-1.72507838719557));
#33250=CARTESIAN_POINT('Ctrl Pts',(97.5084048713763,-1.02161034847966,-1.72210847033308));
#33251=CARTESIAN_POINT('Ctrl Pts',(97.5464054283538,-0.982631012808632,
-1.71914269241105));
#33252=CARTESIAN_POINT('Ctrl Pts',(97.582295884973,-0.941458811592886,-1.71617691448902));
#33253=CARTESIAN_POINT('Ctrl Pts',(97.6158117674441,-0.898355693078501,
-1.71321113656699));
#33254=CARTESIAN_POINT('Ctrl Pts',(97.6492950240057,-0.855294533132349,
-1.7102482456703));
#33255=CARTESIAN_POINT('Ctrl Pts',(97.680407949961,-0.810306603147918,-1.7072853547736));
#33256=CARTESIAN_POINT('Ctrl Pts',(97.7089246749727,-0.763688755004287,
-1.70432246387691));
#33257=CARTESIAN_POINT('Ctrl Pts',(97.7374256171912,-0.71709670785511,-1.7013612128142));
#33258=CARTESIAN_POINT('Ctrl Pts',(97.763332922242,-0.668876992338361,-1.69839996175149));
#33259=CARTESIAN_POINT('Ctrl Pts',(97.7864640610347,-0.619355340760716,
-1.69543871068878));
#33260=CARTESIAN_POINT('Ctrl Pts',(97.8096066161747,-0.569809247828204,
-1.69247599810397));
#33261=CARTESIAN_POINT('Ctrl Pts',(97.8299700258084,-0.518960422619599,
-1.68951328551917));
#33262=CARTESIAN_POINT('Ctrl Pts',(97.8474186374867,-0.467157467943752,
-1.68655057293436));
#33263=CARTESIAN_POINT('Ctrl Pts',(97.8648705622482,-0.41534467709887,-1.68358729779975));
#33264=CARTESIAN_POINT('Ctrl Pts',(97.8794064323308,-0.362577917863619,
-1.68062402266515));
#33265=CARTESIAN_POINT('Ctrl Pts',(97.8909405843745,-0.30922076776162,-1.67766074753054));
#33266=CARTESIAN_POINT('Ctrl Pts',(97.9024939141118,-0.255774901378304,
-1.67469254539458));
#33267=CARTESIAN_POINT('Ctrl Pts',(97.9110354636563,-0.20173722036308,-1.67172434325863));
#33268=CARTESIAN_POINT('Ctrl Pts',(97.9165310580184,-0.147479936628166,
-1.66875614112267));
#33269=CARTESIAN_POINT('Ctrl Pts',(97.9215307549522,-0.0981185832863154,
-1.66605577604102));
#33270=CARTESIAN_POINT('Ctrl Pts',(97.9240100444567,-0.0485758494338648,
-1.66335541095937));
#33271=CARTESIAN_POINT('Ctrl Pts',(97.9239806916945,0.000868804938497931,
-1.66065504587772));
#33272=CARTESIAN_POINT('Ctrl Pts',(97.9239806575939,0.000924464373924056,
-1.58934495419106));
#33273=CARTESIAN_POINT('Ctrl Pts',(97.9240149768248,-0.0534055734513773,
-1.59231137819076));
#33274=CARTESIAN_POINT('Ctrl Pts',(97.921019683887,-0.107852860549419,-1.59527780219046));
#33275=CARTESIAN_POINT('Ctrl Pts',(97.9149819784938,-0.162046310911714,
-1.59824422619017));
#33276=CARTESIAN_POINT('Ctrl Pts',(97.9089514956399,-0.216174932948707,
-1.60120710163744));
#33277=CARTESIAN_POINT('Ctrl Pts',(97.8998858605244,-0.270049782617476,
-1.60416997708471));
#33278=CARTESIAN_POINT('Ctrl Pts',(97.8878242733974,-0.323300612349155,
-1.60713285253198));
#33279=CARTESIAN_POINT('Ctrl Pts',(97.8757720383231,-0.376510153603537,
-1.61009343068893));
#33280=CARTESIAN_POINT('Ctrl Pts',(97.8607285693229,-0.42909610405418,-1.61305400884588));
#33281=CARTESIAN_POINT('Ctrl Pts',(97.8427844382153,-0.480696697823331,
-1.61601458700284));
#33282=CARTESIAN_POINT('Ctrl Pts',(97.8248466701853,-0.532278993767196,
-1.61897411532416));
#33283=CARTESIAN_POINT('Ctrl Pts',(97.804010457373,-0.582876112447669,-1.62193364364548));
#33284=CARTESIAN_POINT('Ctrl Pts',(97.7804159654134,-0.632142233970416,
-1.6248931719668));
#33285=CARTESIAN_POINT('Ctrl Pts',(97.7568030420099,-0.681446840990178,
-1.62785501219974));
#33286=CARTESIAN_POINT('Ctrl Pts',(97.7304277661814,-0.729417880164871,
-1.63081685243267));
#33287=CARTESIAN_POINT('Ctrl Pts',(97.7014774289467,-0.775731904843368,
-1.6337786926656));
#33288=CARTESIAN_POINT('Ctrl Pts',(97.6725165864269,-0.822062735614098,
-1.63674160766931));
#33289=CARTESIAN_POINT('Ctrl Pts',(97.640979133725,-0.866734907890897,-1.63970452267302));
#33290=CARTESIAN_POINT('Ctrl Pts',(97.6070951758126,-0.909454818115819,
-1.64266743767673));
#33291=CARTESIAN_POINT('Ctrl Pts',(97.5731476039496,-0.952254930962463,
-1.64563591527525));
#33292=CARTESIAN_POINT('Ctrl Pts',(97.5368450900147,-0.993095053534944,
-1.64860439287378));
#33293=CARTESIAN_POINT('Ctrl Pts',(97.4984565286632,-1.03171650525743,-1.6515728704723));
#33294=CARTESIAN_POINT('Ctrl Pts',(97.4664553344499,-1.06391183985348,-1.6540474312478));
#33295=CARTESIAN_POINT('Ctrl Pts',(97.4330053213571,-1.09456596514532,-1.6565219920233));
#33296=CARTESIAN_POINT('Ctrl Pts',(97.3982789955736,-1.12355110027316,-1.65899655279881));
#33297=CARTESIAN_POINT('Ctrl Pts',(97.3560368694842,-1.1588094728525,-1.66200668145296));
#33298=CARTESIAN_POINT('Ctrl Pts',(97.3117148111456,-1.19175635038155,-1.66501681010711));
#33299=CARTESIAN_POINT('Ctrl Pts',(97.2655957836383,-1.2221384348651,-1.66802693876127));
#33300=CARTESIAN_POINT('Ctrl Pts',(97.2195587226361,-1.25246652182484,-1.67103171756874));
#33301=CARTESIAN_POINT('Ctrl Pts',(97.1717314678766,-1.2802385736523,-1.67403649637622));
#33302=CARTESIAN_POINT('Ctrl Pts',(97.1224294527346,-1.30524190446346,-1.6770412751837));
#33303=CARTESIAN_POINT('Ctrl Pts',(97.0731762137674,-1.33022049862179,-1.68004308126043));
#33304=CARTESIAN_POINT('Ctrl Pts',(97.0224515733797,-1.35243556027356,-1.68304488733716));
#33305=CARTESIAN_POINT('Ctrl Pts',(96.970597703677,-1.37171904819699,-1.6860466934139));
#33306=CARTESIAN_POINT('Ctrl Pts',(96.9187746537621,-1.39099107481565,-1.6890467153417));
#33307=CARTESIAN_POINT('Ctrl Pts',(96.8658241988373,-1.40733479755615,-1.6920467372695));
#33308=CARTESIAN_POINT('Ctrl Pts',(96.8121086166901,-1.42063022413315,-1.69504675919731));
#33309=CARTESIAN_POINT('Ctrl Pts',(96.7584037457529,-1.43392299952217,-1.6980461829027));
#33310=CARTESIAN_POINT('Ctrl Pts',(96.7039345629515,-1.44416855909227,-1.7010456066081));
#33311=CARTESIAN_POINT('Ctrl Pts',(96.6490763892943,-1.45129735413451,-1.7040450303135));
#33312=CARTESIAN_POINT('Ctrl Pts',(96.5941677814879,-1.4584327030718,-1.70704721155478));
#33313=CARTESIAN_POINT('Ctrl Pts',(96.5388699931839,-1.46244549455437,-1.71004939279606));
#33314=CARTESIAN_POINT('Ctrl Pts',(96.4835648799873,-1.46331793611533,-1.71305157403735));
#33315=CARTESIAN_POINT('Ctrl Pts',(96.4282345931287,-1.46419077479235,-1.716055121805));
#33316=CARTESIAN_POINT('Ctrl Pts',(96.3728975033235,-1.46192043578891,-1.71905866957266));
#33317=CARTESIAN_POINT('Ctrl Pts',(96.3179335580145,-1.45654127684688,-1.72206221734031));
#33318=CARTESIAN_POINT('Ctrl Pts',(96.2628658775037,-1.45115196564713,-1.72507143379917));
#33319=CARTESIAN_POINT('Ctrl Pts',(96.2081732714503,-1.44264219490996,-1.72808065025804));
#33320=CARTESIAN_POINT('Ctrl Pts',(96.1542275091506,-1.43109785836854,-1.7310898667169));
#33321=CARTESIAN_POINT('Ctrl Pts',(96.1129567890792,-1.42226596756747,-1.73339204069339));
#33322=CARTESIAN_POINT('Ctrl Pts',(96.0721230332597,-1.41165905690264,-1.73569421466988));
#33323=CARTESIAN_POINT('Ctrl Pts',(96.031885835997,-1.39933501300273,-1.73799638864636));
#33324=CARTESIAN_POINT('Ctrl Pts',(95.9792750683316,-1.38322113195669,-1.74100651729453));
#33325=CARTESIAN_POINT('Ctrl Pts',(95.9274637731497,-1.36410225986706,-1.7440166459427));
#33326=CARTESIAN_POINT('Ctrl Pts',(95.8768187042549,-1.34207698489527,-1.74702677459087));
#33327=CARTESIAN_POINT('Ctrl Pts',(95.826263645925,-1.3200908550463,-1.75003155339184));
#33328=CARTESIAN_POINT('Ctrl Pts',(95.7768711809521,-1.29520878219504,-1.75303633219281));
#33329=CARTESIAN_POINT('Ctrl Pts',(95.7289917910453,-1.26757873954662,-1.75604111099377));
#33330=CARTESIAN_POINT('Ctrl Pts',(95.6811597698665,-1.23997603225015,-1.75904291706368));
#33331=CARTESIAN_POINT('Ctrl Pts',(95.6348383135608,-1.2096310033596,-1.76204472313358));
#33332=CARTESIAN_POINT('Ctrl Pts',(95.5903551226692,-1.176738414155,-1.76504652920349));
#33333=CARTESIAN_POINT('Ctrl Pts',(95.5458983707444,-1.1438653749435,-1.76804655112416));
#33334=CARTESIAN_POINT('Ctrl Pts',(95.5032781424389,-1.10844808995638,-1.77104657304482));
#33335=CARTESIAN_POINT('Ctrl Pts',(95.4627928816826,-1.07072441327407,-1.77404659496549));
#33336=CARTESIAN_POINT('Ctrl Pts',(95.4223156939345,-1.03300825892333,-1.77704601866346));
#33337=CARTESIAN_POINT('Ctrl Pts',(95.3839730144261,-0.992986986058309,
-1.78004544236143));
#33338=CARTESIAN_POINT('Ctrl Pts',(95.348028165999,-0.950936934980199,-1.7830448660594));
#33339=CARTESIAN_POINT('Ctrl Pts',(95.312050271492,-0.908848224972956,-1.78604704729286));
#33340=CARTESIAN_POINT('Ctrl Pts',(95.2784749561784,-0.864727412690527,
-1.78904922852632));
#33341=CARTESIAN_POINT('Ctrl Pts',(95.2475257661328,-0.818884590742626,
-1.79205140975978));
#33342=CARTESIAN_POINT('Ctrl Pts',(95.216562488704,-0.773020902161633,-1.79505495751938));
#33343=CARTESIAN_POINT('Ctrl Pts',(95.1882279900561,-0.72543409598279,-1.79805850527897));
#33344=CARTESIAN_POINT('Ctrl Pts',(95.162701096448,-0.676461161348169,-1.80106205303857));
#33345=CARTESIAN_POINT('Ctrl Pts',(95.1371260251242,-0.627395798541108,
-1.80407126948909));
#33346=CARTESIAN_POINT('Ctrl Pts',(95.1143693618401,-0.576939563841812,
-1.80708048593961));
#33347=CARTESIAN_POINT('Ctrl Pts',(95.0945623015679,-0.525450756038149,
-1.81008970239013));
#33348=CARTESIAN_POINT('Ctrl Pts',(95.0794090878959,-0.486059705794032,
-1.81239187642473));
#33349=CARTESIAN_POINT('Ctrl Pts',(95.0659812567716,-0.446064760948663,
-1.81469405045933));
#33350=CARTESIAN_POINT('Ctrl Pts',(95.054317528291,-0.405631215067501,-1.81699622449392));
#33351=CARTESIAN_POINT('Ctrl Pts',(95.0390670203038,-0.352763719443278,
-1.82000635316426));
#33352=CARTESIAN_POINT('Ctrl Pts',(95.0267701018704,-0.298923888233537,
-1.8230164818346));
#33353=CARTESIAN_POINT('Ctrl Pts',(95.0175445955868,-0.24447275581039,-1.82602661050493));
#33354=CARTESIAN_POINT('Ctrl Pts',(95.0083354856268,-0.1901183983884,-1.82903138932867));
#33355=CARTESIAN_POINT('Ctrl Pts',(95.002187042368,-0.135155412313231,-1.83203616815241));
#33356=CARTESIAN_POINT('Ctrl Pts',(94.9991668360948,-0.0799581874332898,
-1.83504094697615));
#33357=CARTESIAN_POINT('Ctrl Pts',(94.9961496178151,-0.0248155710604053,
-1.83804275306917));
#33358=CARTESIAN_POINT('Ctrl Pts',(94.9962545344399,0.0305603003156849,
-1.8410445591622));
#33359=CARTESIAN_POINT('Ctrl Pts',(94.9994975224402,0.0857885518684098,
-1.84404636525523));
#33360=CARTESIAN_POINT('Ctrl Pts',(95.0027385829432,0.140983978041141,-1.84704638719933));
#33361=CARTESIAN_POINT('Ctrl Pts',(95.0091139870974,0.19603143213972,-1.85004640914343));
#33362=CARTESIAN_POINT('Ctrl Pts',(95.0185875942964,0.250550996800594,-1.85304643108753));
#33363=CARTESIAN_POINT('Ctrl Pts',(95.0280593124013,0.305059689932115,-1.8560458548092));
#33364=CARTESIAN_POINT('Ctrl Pts',(95.0406279162633,0.359040182648933,-1.85904527853087));
#33365=CARTESIAN_POINT('Ctrl Pts',(95.056205842006,0.41212094372446,-1.86204470225253));
#33366=CARTESIAN_POINT('Ctrl Pts',(95.0717980893953,0.4652505048723,-1.86504688350992));
#33367=CARTESIAN_POINT('Ctrl Pts',(95.090405037007,0.517478173961618,-1.8680490647673));
#33368=CARTESIAN_POINT('Ctrl Pts',(95.1118891186283,0.568447291750489,-1.87105124602469));
#33369=CARTESIAN_POINT('Ctrl Pts',(95.133382979327,0.619439609550978,-1.87405479380837));
#33370=CARTESIAN_POINT('Ctrl Pts',(95.1577563518279,0.669171759032316,-1.87705834159206));
#33371=CARTESIAN_POINT('Ctrl Pts',(95.184824708617,0.71730983884226,-1.88006188937574));
#33372=CARTESIAN_POINT('Ctrl Pts',(95.2119441523736,0.765538771175316,-1.88307110585032));
#33373=CARTESIAN_POINT('Ctrl Pts',(95.2417684558908,0.812167177828806,-1.88608032232489));
#33374=CARTESIAN_POINT('Ctrl Pts',(95.274069218705,0.85688940642843,-1.88908953879947));
#33375=CARTESIAN_POINT('Ctrl Pts',(95.2987806251552,0.891103742933179,-1.89139171264681));
#33376=CARTESIAN_POINT('Ctrl Pts',(95.3249405515936,0.924202990934809,-1.89369388649415));
#33377=CARTESIAN_POINT('Ctrl Pts',(95.3524317167492,0.956064405586572,-1.89599606034149));
#33378=CARTESIAN_POINT('Ctrl Pts',(95.3883768493095,0.997723708374811,-1.89900618900105));
#33379=CARTESIAN_POINT('Ctrl Pts',(95.4267501688151,1.03744058079069,-1.90201631766061));
#33380=CARTESIAN_POINT('Ctrl Pts',(95.4673136770704,1.07491907547582,-1.90502644632017));
#33381=CARTESIAN_POINT('Ctrl Pts',(95.5078050925418,1.11233096031552,-1.90803122513294));
#33382=CARTESIAN_POINT('Ctrl Pts',(95.5504785871506,1.14751200675065,-1.9110360039457));
#33383=CARTESIAN_POINT('Ctrl Pts',(95.5950575194639,1.18020105770639,-1.91404078275847));
#33384=CARTESIAN_POINT('Ctrl Pts',(95.6395923483092,1.21285776826188,-1.91704258884041));
#33385=CARTESIAN_POINT('Ctrl Pts',(95.6860284567455,1.24302705644994,-1.92004439492235));
#33386=CARTESIAN_POINT('Ctrl Pts',(95.7340555594834,1.2704874665369,-1.92304620100429));
#33387=CARTESIAN_POINT('Ctrl Pts',(95.7820541169036,1.29793155529517,-1.92604622293721));
#33388=CARTESIAN_POINT('Ctrl Pts',(95.8316413367919,1.32266969555349,-1.92904624487013));
#33389=CARTESIAN_POINT('Ctrl Pts',(95.8824792810488,1.34452457068608,-1.93204626680305));
#33390=CARTESIAN_POINT('Ctrl Pts',(95.9333070879124,1.36637508782451,-1.93504569051347));
#33391=CARTESIAN_POINT('Ctrl Pts',(95.9853846389323,1.38534327318461,-1.93804511422389));
#33392=CARTESIAN_POINT('Ctrl Pts',(96.0383529221512,1.40129946066557,-1.94104453793431));
#33393=CARTESIAN_POINT('Ctrl Pts',(96.0913699020352,1.41727031754997,-1.94404671918042));
#33394=CARTESIAN_POINT('Ctrl Pts',(96.1452787434154,1.43022349160589,-1.94704890042653));
#33395=CARTESIAN_POINT('Ctrl Pts',(96.1997055689419,1.44007932102875,-1.95005108167264));
#33396=CARTESIAN_POINT('Ctrl Pts',(96.2541571683514,1.44993963660641,-1.95305462944502));
#33397=CARTESIAN_POINT('Ctrl Pts',(96.3091266968271,1.45669973255316,-1.9560581772174));
#33398=CARTESIAN_POINT('Ctrl Pts',(96.3642336778932,1.46033171323964,-1.95906172498978));
#33399=CARTESIAN_POINT('Ctrl Pts',(96.4194446641128,1.46397054867848,-1.96207094145314));
#33400=CARTESIAN_POINT('Ctrl Pts',(96.4747930917616,1.46446947034545,-1.96508015791651));
#33401=CARTESIAN_POINT('Ctrl Pts',(96.5298981716358,1.46185276251805,-1.96808937437987));
#33402=CARTESIAN_POINT('Ctrl Pts',(96.5720558163894,1.45985087377633,-1.97039154831627));
#33403=CARTESIAN_POINT('Ctrl Pts',(96.6140710101391,1.45602653043774,-1.97269372225266));
#33404=CARTESIAN_POINT('Ctrl Pts',(96.6557768687262,1.4504108914248,-1.97499589618905));
#33405=CARTESIAN_POINT('Ctrl Pts',(96.710307935311,1.44306835502092,-1.97800602484887));
#33406=CARTESIAN_POINT('Ctrl Pts',(96.7645389159977,1.43263081037028,-1.98101615350868));
#33407=CARTESIAN_POINT('Ctrl Pts',(96.8180919056289,1.41913588289201,-1.9840262821685));
#33408=CARTESIAN_POINT('Ctrl Pts',(96.8715497165069,1.40566493970255,-1.98703106098147));
#33409=CARTESIAN_POINT('Ctrl Pts',(96.9243314196578,1.38914752516233,-1.99003583979444));
#33410=CARTESIAN_POINT('Ctrl Pts',(96.9760671332099,1.36967263871585,-1.99304061860741));
#33411=CARTESIAN_POINT('Ctrl Pts',(97.0277516628442,1.35021701944321,-1.99604242468953));
#33412=CARTESIAN_POINT('Ctrl Pts',(97.0783917610071,1.32780990952682,-1.99904423077165));
#33413=CARTESIAN_POINT('Ctrl Pts',(97.1276324138976,1.30259017870354,-2.00204603685377));
#33414=CARTESIAN_POINT('Ctrl Pts',(97.1768438001859,1.27738543744239,-2.00504605878684));
#33415=CARTESIAN_POINT('Ctrl Pts',(97.224656920717,1.24937162897035,-2.00804608071991));
#33416=CARTESIAN_POINT('Ctrl Pts',(97.2707386199934,1.21873490043214,-2.01104610265298));
#33417=CARTESIAN_POINT('Ctrl Pts',(97.3168111303002,1.18810428104301,-2.01404552636353));
#33418=CARTESIAN_POINT('Ctrl Pts',(97.3611524654717,1.15485207251944,-2.01704495007407));
#33419=CARTESIAN_POINT('Ctrl Pts',(97.4034578639348,1.11920810798898,-2.02004437378461));
#33420=CARTESIAN_POINT('Ctrl Pts',(97.4458021560839,1.08353137399608,-2.0230465550308));
#33421=CARTESIAN_POINT('Ctrl Pts',(97.48610636727,1.04545883194557,-2.02604873627698));
#33422=CARTESIAN_POINT('Ctrl Pts',(97.5240994934715,1.00526008728279,-2.02905091752317));
#33423=CARTESIAN_POINT('Ctrl Pts',(97.5621099133003,0.965043045044023,-2.0320544652956));
#33424=CARTESIAN_POINT('Ctrl Pts',(97.5978068101609,0.922698275436627,-2.03505801306803));
#33425=CARTESIAN_POINT('Ctrl Pts',(97.6309589298598,0.878529195686235,-2.03806156084045));
#33426=CARTESIAN_POINT('Ctrl Pts',(97.6641736186053,0.834276754231234,-2.04107077730382));
#33427=CARTESIAN_POINT('Ctrl Pts',(97.69483364252,0.78819356532067,-2.04407999376719));
#33428=CARTESIAN_POINT('Ctrl Pts',(97.7227512786132,0.740611818994866,-2.04708921023056));
#33429=CARTESIAN_POINT('Ctrl Pts',(97.7441094145043,0.704209832789047,-2.04939138416591));
#33430=CARTESIAN_POINT('Ctrl Pts',(97.7638633609549,0.66693137109563,-2.05169355810126));
#33431=CARTESIAN_POINT('Ctrl Pts',(97.781948029552,0.628933229001592,-2.05399573203661));
#33432=CARTESIAN_POINT('Ctrl Pts',(97.8074222819931,0.575408650500181,-2.0572385982068));
#33433=CARTESIAN_POINT('Ctrl Pts',(97.8296770995285,0.520258080670813,-2.06048146437699));
#33434=CARTESIAN_POINT('Ctrl Pts',(97.8485205066686,0.463873299456797,-2.06372433054717));
#33435=CARTESIAN_POINT('Ctrl Pts',(97.8673150132779,0.407634842403311,-2.06695878115451));
#33436=CARTESIAN_POINT('Ctrl Pts',(97.8827155902678,0.350168916233823,-2.07019323176185));
#33437=CARTESIAN_POINT('Ctrl Pts',(97.8945777827573,0.291887860422791,-2.07342768236918));
#33438=CARTESIAN_POINT('Ctrl Pts',(97.9063938671677,0.233833341783416,-2.07664956073873));
#33439=CARTESIAN_POINT('Ctrl Pts',(97.9146988686464,0.174970387112386,-2.07987143910827));
#33440=CARTESIAN_POINT('Ctrl Pts',(97.9193983752572,0.11572465185336,-2.08309331747781));
#33441=CARTESIAN_POINT('Ctrl Pts',(97.9224379693847,0.0774050996357042,
-2.08517719635755));
#33442=CARTESIAN_POINT('Ctrl Pts',(97.9239702396369,0.0389257709143198,
-2.08726107523728));
#33443=CARTESIAN_POINT('Ctrl Pts',(97.9239808936025,0.000404768228821613,
-2.08934495411702));
#33444=CARTESIAN_POINT('Origin',(96.460480949577,-8.32667268468867E-16,
1.18130019239114E-14));
#33445=CARTESIAN_POINT('',(97.9239803697841,-0.00130271001786886,-2.6606550458059));
#33446=CARTESIAN_POINT('',(97.9239803753015,-0.00129649685740057,-2.58934495412449));
#33447=CARTESIAN_POINT('',(97.923980949577,-1.01189432752408E-15,1.19922289829666E-14));
#33448=CARTESIAN_POINT('Ctrl Pts',(97.9239803697841,-0.00130271001787374,
-2.6606550458059));
#33449=CARTESIAN_POINT('Ctrl Pts',(97.924028892116,0.0532085807223716,-2.65769006743583));
#33450=CARTESIAN_POINT('Ctrl Pts',(97.9210275607864,0.107804431595655,-2.65472508906576));
#33451=CARTESIAN_POINT('Ctrl Pts',(97.9149746591878,0.162111994320599,-2.6517601106957));
#33452=CARTESIAN_POINT('Ctrl Pts',(97.9089263301197,0.216378531600288,-2.64879737215286));
#33453=CARTESIAN_POINT('Ctrl Pts',(97.8998310544556,0.270356673964938,-2.64583463361002));
#33454=CARTESIAN_POINT('Ctrl Pts',(97.887739109395,0.323676374227503,-2.64287189506718));
#33455=CARTESIAN_POINT('Ctrl Pts',(97.8756512268637,0.376978160676594,-2.63991015191527));
#33456=CARTESIAN_POINT('Ctrl Pts',(97.8605687908678,0.429621414540402,-2.63694840876335));
#33457=CARTESIAN_POINT('Ctrl Pts',(97.8425931245834,0.481246491622603,-2.63398666561144));
#33458=CARTESIAN_POINT('Ctrl Pts',(97.8246030797137,0.53291286317251,-2.63102255338592));
#33459=CARTESIAN_POINT('Ctrl Pts',(97.803715356552,0.583558915781514,-2.62805844116042));
#33460=CARTESIAN_POINT('Ctrl Pts',(97.7800805804418,0.632842053139188,-2.62509432893491));
#33461=CARTESIAN_POINT('Ctrl Pts',(97.7564368907842,0.682143776989095,-2.62212909883314));
#33462=CARTESIAN_POINT('Ctrl Pts',(97.7300443453952,0.7300810844637,-2.61916386873138));
#33463=CARTESIAN_POINT('Ctrl Pts',(97.701099412135,0.776336319104215,-2.61619863862962));
#33464=CARTESIAN_POINT('Ctrl Pts',(97.6721000727146,0.822678497103016,-2.61322783495191));
#33465=CARTESIAN_POINT('Ctrl Pts',(97.6405390775404,0.867331843094967,-2.61025703127421));
#33466=CARTESIAN_POINT('Ctrl Pts',(97.6066552965318,0.910009129834844,-2.6072862275965));
#33467=CARTESIAN_POINT('Ctrl Pts',(97.5790164534826,0.944820794733497,-2.60486295681224));
#33468=CARTESIAN_POINT('Ctrl Pts',(97.549832995274,0.978318193879708,-2.60243968602799));
#33469=CARTESIAN_POINT('Ctrl Pts',(97.5192522745611,1.01036405883789,-2.60001641524373));
#33470=CARTESIAN_POINT('Ctrl Pts',(97.4812656391025,1.05017066122483,-2.5970062865825));
#33471=CARTESIAN_POINT('Ctrl Pts',(97.4409511564579,1.08791564893057,-2.59399615792126));
#33472=CARTESIAN_POINT('Ctrl Pts',(97.3985613494285,1.12331536685584,-2.59098602926002));
#33473=CARTESIAN_POINT('Ctrl Pts',(97.3562468810303,1.15865216950778,-2.58798125044558));
#33474=CARTESIAN_POINT('Ctrl Pts',(97.3118648100527,1.1916516384344,-2.58497647163114));
#33475=CARTESIAN_POINT('Ctrl Pts',(97.2657045114627,1.22206680070452,-2.5819716928167));
#33476=CARTESIAN_POINT('Ctrl Pts',(97.2195898808406,1.25245187221056,-2.57896988673308));
#33477=CARTESIAN_POINT('Ctrl Pts',(97.1717009464437,1.28025741270252,-2.57596808064946));
#33478=CARTESIAN_POINT('Ctrl Pts',(97.122358696316,1.30527778590293,-2.57296627456584));
#33479=CARTESIAN_POINT('Ctrl Pts',(97.0730457731752,1.33028328803137,-2.56996625263124));
#33480=CARTESIAN_POINT('Ctrl Pts',(97.0222817164732,1.35250666558854,-2.56696623069665));
#33481=CARTESIAN_POINT('Ctrl Pts',(96.9704129215266,1.37178775106925,-2.56396620876205));
#33482=CARTESIAN_POINT('Ctrl Pts',(96.9185544695313,1.39106499178496,-2.56096678504996));
#33483=CARTESIAN_POINT('Ctrl Pts',(96.8655922115242,1.40740092169674,-2.55796736133787));
#33484=CARTESIAN_POINT('Ctrl Pts',(96.8118912035211,1.42068401955641,-2.55496793762578));
#33485=CARTESIAN_POINT('Ctrl Pts',(96.7581408252191,1.43397932930064,-2.55196575637802));
#33486=CARTESIAN_POINT('Ctrl Pts',(96.7036508537876,1.44421607261516,-2.54896357513026));
#33487=CARTESIAN_POINT('Ctrl Pts',(96.6487986873739,1.45133341435765,-2.54596139388251));
#33488=CARTESIAN_POINT('Ctrl Pts',(96.5939215534718,1.45845399575611,-2.54295784610849));
#33489=CARTESIAN_POINT('Ctrl Pts',(96.5386824236007,1.46245230695219,-2.53995429833447));
#33490=CARTESIAN_POINT('Ctrl Pts',(96.4834626938998,1.46331954453833,-2.53695075056046));
#33491=CARTESIAN_POINT('Ctrl Pts',(96.4281387462522,1.46418841888947,-2.53394153409549));
#33492=CARTESIAN_POINT('Ctrl Pts',(96.3728348008828,1.46191443648741,-2.53093231763053));
#33493=CARTESIAN_POINT('Ctrl Pts',(96.3179299526928,1.45654092400019,-2.52792310116557));
#33494=CARTESIAN_POINT('Ctrl Pts',(96.2759254936491,1.45242996672353,-2.52562092724244));
#33495=CARTESIAN_POINT('Ctrl Pts',(96.2341545894424,1.44650597742633,-2.52331875331931));
#33496=CARTESIAN_POINT('Ctrl Pts',(96.1927823540791,1.43880843477109,-2.52101657939618));
#33497=CARTESIAN_POINT('Ctrl Pts',(96.1386875047738,1.42874377652143,-2.51800645073495));
#33498=CARTESIAN_POINT('Ctrl Pts',(96.085047386684,1.41560302543568,-2.51499632207372));
#33499=CARTESIAN_POINT('Ctrl Pts',(96.0322375460565,1.39944268812308,-2.5119861934125));
#33500=CARTESIAN_POINT('Ctrl Pts',(95.9795215633959,1.38331107228337,-2.50898141459806));
#33501=CARTESIAN_POINT('Ctrl Pts',(95.927633430702,1.36417067366608,-2.50597663578363));
#33502=CARTESIAN_POINT('Ctrl Pts',(95.8769381077974,1.342128906554,-2.50297185696919));
#33503=CARTESIAN_POINT('Ctrl Pts',(95.826292939516,1.32010894611872,-2.49997005088558));
#33504=CARTESIAN_POINT('Ctrl Pts',(95.7768387252643,1.29519351290047,-2.49696824480197));
#33505=CARTESIAN_POINT('Ctrl Pts',(95.7289230775661,1.26753908417015,-2.49396643871835));
#33506=CARTESIAN_POINT('Ctrl Pts',(95.6810359089415,1.23990109208518,-2.49096641678377));
#33507=CARTESIAN_POINT('Ctrl Pts',(95.6346859508392,1.20952759464432,-2.48796639484918));
#33508=CARTESIAN_POINT('Ctrl Pts',(95.5901966168965,1.17662119235161,-2.48496637291459));
#33509=CARTESIAN_POINT('Ctrl Pts',(95.545716154396,1.14372135179439,-2.4819669492025));
#33510=CARTESIAN_POINT('Ctrl Pts',(95.5030960035813,1.10828992331889,-2.47896752549042));
#33511=CARTESIAN_POINT('Ctrl Pts',(95.4626290316732,1.07057171639067,-2.47596810177833));
#33512=CARTESIAN_POINT('Ctrl Pts',(95.4221248562456,1.03281883303431,-2.47296592053058));
#33513=CARTESIAN_POINT('Ctrl Pts',(95.3837782017353,0.992775331836872,-2.46996373928283));
#33514=CARTESIAN_POINT('Ctrl Pts',(95.3478462280774,0.950724053820785,-2.46696155803508));
#33515=CARTESIAN_POINT('Ctrl Pts',(95.3118978989827,0.908653634996414,-2.46395801026106));
#33516=CARTESIAN_POINT('Ctrl Pts',(95.2783667620356,0.864574038623944,-2.46095446248705));
#33517=CARTESIAN_POINT('Ctrl Pts',(95.24746858368,0.818799884087048,-2.45795091471304));
#33518=CARTESIAN_POINT('Ctrl Pts',(95.2165120902127,0.772939338536952,-2.45494169824808));
#33519=CARTESIAN_POINT('Ctrl Pts',(95.1881987530261,0.725378300840873,-2.45193248178312));
#33520=CARTESIAN_POINT('Ctrl Pts',(95.1626994208353,0.67645794670244,-2.44892326531817));
#33521=CARTESIAN_POINT('Ctrl Pts',(95.1431913866637,0.639031870871124,-2.44662109139498));
#33522=CARTESIAN_POINT('Ctrl Pts',(95.1253294290495,0.600810769922743,-2.4443189174718));
#33523=CARTESIAN_POINT('Ctrl Pts',(95.1091707011953,0.56195450226743,-2.44201674354862));
#33524=CARTESIAN_POINT('Ctrl Pts',(95.0880429100438,0.511149320364774,-2.43900661488736));
#33525=CARTESIAN_POINT('Ctrl Pts',(95.0697398927803,0.459044223043108,-2.4359964862261));
#33526=CARTESIAN_POINT('Ctrl Pts',(95.0544195205938,0.405984615380659,-2.43298635756484));
#33527=CARTESIAN_POINT('Ctrl Pts',(95.0391263770255,0.353019309591584,-2.42998157875037));
#33528=CARTESIAN_POINT('Ctrl Pts',(95.0268055039807,0.299103363331115,-2.4269767999359));
#33529=CARTESIAN_POINT('Ctrl Pts',(95.017566351721,0.244601131015325,-2.42397202112144));
#33530=CARTESIAN_POINT('Ctrl Pts',(95.0083363400718,0.190152819628835,-2.42097021503779));
#33531=CARTESIAN_POINT('Ctrl Pts',(95.0021820974107,0.135119889332189,-2.41796840895415));
#33532=CARTESIAN_POINT('Ctrl Pts',(94.9991625039305,0.0798789735359879,
-2.41496660287051));
#33533=CARTESIAN_POINT('Ctrl Pts',(94.9961447051714,0.0246708906487744,
-2.41196658093589));
#33534=CARTESIAN_POINT('Ctrl Pts',(94.9962578915633,-0.0307444064430082,
-2.40896655900127));
#33535=CARTESIAN_POINT('Ctrl Pts',(94.9995090916734,-0.0859853499940245,
-2.40596653706665));
#33536=CARTESIAN_POINT('Ctrl Pts',(95.0027596434745,-0.141215278166994,
-2.40296711335454));
#33537=CARTESIAN_POINT('Ctrl Pts',(95.009146935292,-0.196270394937041,-2.39996768964242));
#33538=CARTESIAN_POINT('Ctrl Pts',(95.0186259541096,-0.25077165319408,-2.39696826593031));
#33539=CARTESIAN_POINT('Ctrl Pts',(95.0281136875121,-0.305323017464164,
-2.39396608468253));
#33540=CARTESIAN_POINT('Ctrl Pts',(95.0406987359633,-0.359318984497081,
-2.39096390343475));
#33541=CARTESIAN_POINT('Ctrl Pts',(95.0562847236741,-0.412389632701869,
-2.38796172218697));
#33542=CARTESIAN_POINT('Ctrl Pts',(95.0718778057804,-0.465484437487563,
-2.38495817441293));
#33543=CARTESIAN_POINT('Ctrl Pts',(95.0904743724567,-0.517652585520922,
-2.38195462663889));
#33544=CARTESIAN_POINT('Ctrl Pts',(95.1119288154397,-0.568541459802043,
-2.37895107886486));
#33545=CARTESIAN_POINT('Ctrl Pts',(95.1334237500733,-0.619526378269138,
-2.37594186239987));
#33546=CARTESIAN_POINT('Ctrl Pts',(95.15778710286,-0.669226724449195,-2.37293264593488));
#33547=CARTESIAN_POINT('Ctrl Pts',(95.1848264810336,-0.717312990879972,
-2.3699234294699));
#33548=CARTESIAN_POINT('Ctrl Pts',(95.2055127134958,-0.754100955427203,
-2.36762125554695));
#33549=CARTESIAN_POINT('Ctrl Pts',(95.2277642106588,-0.789944685160006,
-2.365319081624));
#33550=CARTESIAN_POINT('Ctrl Pts',(95.2514783150874,-0.824708966725413,
-2.36301690770106));
#33551=CARTESIAN_POINT('Ctrl Pts',(95.2824848801017,-0.870163812375398,
-2.36000677903983));
#33552=CARTESIAN_POINT('Ctrl Pts',(95.3161236046273,-0.913963102553221,
-2.3569966503786));
#33553=CARTESIAN_POINT('Ctrl Pts',(95.3521914628132,-0.955785887910526,
-2.35398652171737));
#33554=CARTESIAN_POINT('Ctrl Pts',(95.3881952182524,-0.997534342393801,
-2.35098174290295));
#33555=CARTESIAN_POINT('Ctrl Pts',(95.4266191976168,-1.03731286654294,-2.34797696408852));
#33556=CARTESIAN_POINT('Ctrl Pts',(95.4672180474705,-1.07483071099548,-2.34497218527409));
#33557=CARTESIAN_POINT('Ctrl Pts',(95.5077767314886,-1.11231143775669,-2.34197037919048));
#33558=CARTESIAN_POINT('Ctrl Pts',(95.5505056376785,-1.14753555868996,-2.33896857310687));
#33559=CARTESIAN_POINT('Ctrl Pts',(95.5951214973287,-1.18024796903217,-2.33596676702326));
#33560=CARTESIAN_POINT('Ctrl Pts',(95.6397108391626,-1.21294093647456,-2.33296674508868));
#33561=CARTESIAN_POINT('Ctrl Pts',(95.6861844864651,-1.24312484061695,-2.32996672315409));
#33562=CARTESIAN_POINT('Ctrl Pts',(95.7342267063618,-1.27058530772705,-2.32696670121951));
#33563=CARTESIAN_POINT('Ctrl Pts',(95.7822593463493,-1.29804029905401,-2.32396727750743));
#33564=CARTESIAN_POINT('Ctrl Pts',(95.8318594795136,-1.3227726699341,-2.32096785379535));
#33565=CARTESIAN_POINT('Ctrl Pts',(95.8826850487632,-1.34461301012697,-2.31796843008327));
#33566=CARTESIAN_POINT('Ctrl Pts',(95.9335573447621,-1.36647342934929,-2.31496624883553));
#33567=CARTESIAN_POINT('Ctrl Pts',(95.9856568414113,-1.38543629699036,-2.31196406758778));
#33568=CARTESIAN_POINT('Ctrl Pts',(96.0386210600697,-1.40138020666232,-2.30896188634003));
#33569=CARTESIAN_POINT('Ctrl Pts',(96.0916093868648,-1.41733137364803,-2.30595833856603));
#33570=CARTESIAN_POINT('Ctrl Pts',(96.1454627058692,-1.43026071986212,-2.30295479079202));
#33571=CARTESIAN_POINT('Ctrl Pts',(96.1998061310722,-1.44009752759925,-2.29995124301801));
#33572=CARTESIAN_POINT('Ctrl Pts',(96.2542521203446,-1.44995290065552,-2.29694202655306));
#33573=CARTESIAN_POINT('Ctrl Pts',(96.3091895381736,-1.45670401105605,-2.29393281008811));
#33574=CARTESIAN_POINT('Ctrl Pts',(96.3642372905393,-1.46033195133676,-2.29092359362315));
#33575=CARTESIAN_POINT('Ctrl Pts',(96.4063510771359,-1.46310747433637,-2.28862141969993));
#33576=CARTESIAN_POINT('Ctrl Pts',(96.4485292961512,-1.46405611982684,-2.28631924577671));
#33577=CARTESIAN_POINT('Ctrl Pts',(96.4906026111435,-1.46318998612773,-2.28401707185349));
#33578=CARTESIAN_POINT('Ctrl Pts',(96.5456141331019,-1.46205750267555,-2.28100694319231));
#33579=CARTESIAN_POINT('Ctrl Pts',(96.6006772844208,-1.45781592578263,-2.27799681453112));
#33580=CARTESIAN_POINT('Ctrl Pts',(96.6554123288551,-1.45045992959914,-2.27498668586993));
#33581=CARTESIAN_POINT('Ctrl Pts',(96.7100500936928,-1.44311700709357,-2.27198190705554));
#33582=CARTESIAN_POINT('Ctrl Pts',(96.7643603897109,-1.43267071971393,-2.26897712824115));
#33583=CARTESIAN_POINT('Ctrl Pts',(96.8179656463394,-1.4191676932557,-2.26597234942676));
#33584=CARTESIAN_POINT('Ctrl Pts',(96.8715178694473,-1.40567802580508,-2.2629705433432));
#33585=CARTESIAN_POINT('Ctrl Pts',(96.9243659253177,-1.38913773831275,-2.25996873725964));
#33586=CARTESIAN_POINT('Ctrl Pts',(96.976141379934,-1.36964468770702,-2.25696693117608));
#33587=CARTESIAN_POINT('Ctrl Pts',(97.0278860613677,-1.35016322296197,-2.25396690924153));
#33588=CARTESIAN_POINT('Ctrl Pts',(97.0785589118724,-1.32773265933739,-2.25096688730699));
#33589=CARTESIAN_POINT('Ctrl Pts',(97.1278078724749,-1.30250029864706,-2.24796686537244));
#33590=CARTESIAN_POINT('Ctrl Pts',(97.1770470125367,-1.27727296944203,-2.24496744166041));
#33591=CARTESIAN_POINT('Ctrl Pts',(97.224862356819,-1.24924519339155,-2.24196801794838));
#33592=CARTESIAN_POINT('Ctrl Pts',(97.2709251210342,-1.21861088742511,-2.23896859423635));
#33593=CARTESIAN_POINT('Ctrl Pts',(97.3170302332895,-1.18794841765132,-2.23596641298864));
#33594=CARTESIAN_POINT('Ctrl Pts',(97.3613791057318,-1.15467492349606,-2.23296423174094));
#33595=CARTESIAN_POINT('Ctrl Pts',(97.4036720003372,-1.11902765460283,-2.22996205049323));
#33596=CARTESIAN_POINT('Ctrl Pts',(97.4459841457293,-1.08336415986417,-2.22695850271927));
#33597=CARTESIAN_POINT('Ctrl Pts',(97.4862380632468,-1.04532509986363,-2.22395495494531));
#33598=CARTESIAN_POINT('Ctrl Pts',(97.5241696886636,-1.00518581184794,-2.22095140717135));
#33599=CARTESIAN_POINT('Ctrl Pts',(97.5621729036397,-0.964970767681221,
-2.21794219070643));
#33600=CARTESIAN_POINT('Ctrl Pts',(97.5978447297311,-0.922647981943616,
-2.21493297424152));
#33601=CARTESIAN_POINT('Ctrl Pts',(97.6309611031513,-0.878526300169063,
-2.2119237577766));
#33602=CARTESIAN_POINT('Ctrl Pts',(97.656296486039,-0.844771405355317,-2.20962158385304));
#33603=CARTESIAN_POINT('Ctrl Pts',(97.6801370154664,-0.809964347957141,
-2.20731940992948));
#33604=CARTESIAN_POINT('Ctrl Pts',(97.7024002993347,-0.774253562276253,
-2.20501723600592));
#33605=CARTESIAN_POINT('Ctrl Pts',(97.7322757960106,-0.726332623693341,
-2.20192790786333));
#33606=CARTESIAN_POINT('Ctrl Pts',(97.7594296788854,-0.676590924984949,
-2.19883857972074));
#33607=CARTESIAN_POINT('Ctrl Pts',(97.7836425547771,-0.625360389314989,
-2.19574925157814));
#33608=CARTESIAN_POINT('Ctrl Pts',(97.8077982313761,-0.574250878112431,
-2.19266722151058));
#33609=CARTESIAN_POINT('Ctrl Pts',(97.8290265048961,-0.521659961848709,
-2.18958519144301));
#33610=CARTESIAN_POINT('Ctrl Pts',(97.847152932833,-0.467945574669573,-2.18650316137545));
#33611=CARTESIAN_POINT('Ctrl Pts',(97.8652540308782,-0.414306248038114,
-2.18342543814032));
#33612=CARTESIAN_POINT('Ctrl Pts',(97.8802617284973,-0.359547027438996,
-2.18034771490519));
#33613=CARTESIAN_POINT('Ctrl Pts',(97.8920493474776,-0.304046332213235,
-2.17726999167006));
#33614=CARTESIAN_POINT('Ctrl Pts',(97.9038220450869,-0.248615892606251,
-2.17419616437442));
#33615=CARTESIAN_POINT('Ctrl Pts',(97.9123826613459,-0.192446321192262,
-2.17112233707877));
#33616=CARTESIAN_POINT('Ctrl Pts',(97.9176547047841,-0.13592975073733,-2.16804850978313));
#33617=CARTESIAN_POINT('Ctrl Pts',(97.9218816461293,-0.0906167272115239,
-2.16558402180305));
#33618=CARTESIAN_POINT('Ctrl Pts',(97.9239955432845,-0.0450810319793854,
-2.16311953382297));
#33619=CARTESIAN_POINT('Ctrl Pts',(97.9239808736882,0.000471303021997256,
-2.16065504584289));
#33620=CARTESIAN_POINT('Ctrl Pts',(97.9239808936027,0.000404767488459722,
-2.08934495415707));
#33621=CARTESIAN_POINT('Ctrl Pts',(97.9239966450049,-0.0565468821818031,
-2.09242587966883));
#33622=CARTESIAN_POINT('Ctrl Pts',(97.9206836795153,-0.113466791214522,
-2.09550680518059));
#33623=CARTESIAN_POINT('Ctrl Pts',(97.9140791524384,-0.169954448715279,
-2.09858773069235));
#33624=CARTESIAN_POINT('Ctrl Pts',(97.9074619006337,-0.226550939151006,
-2.10167459212322));
#33625=CARTESIAN_POINT('Ctrl Pts',(97.8975404829998,-0.282713030988987,
-2.10476145355409));
#33626=CARTESIAN_POINT('Ctrl Pts',(97.8844036811519,-0.338047784350542,
-2.10784831498497));
#33627=CARTESIAN_POINT('Ctrl Pts',(97.8712537796522,-0.393437715982223,
-2.11093825454782));
#33628=CARTESIAN_POINT('Ctrl Pts',(97.8548822482323,-0.447998199943239,
-2.11402819411067));
#33629=CARTESIAN_POINT('Ctrl Pts',(97.8354276192171,-0.501352077532047,
-2.11711813367352));
#33630=CARTESIAN_POINT('Ctrl Pts',(97.8159252667035,-0.554836835729674,
-2.12021565306355));
#33631=CARTESIAN_POINT('Ctrl Pts',(97.7933248982422,-0.607108625827405,
-2.12331317245358));
#33632=CARTESIAN_POINT('Ctrl Pts',(97.7678128057932,-0.657811270595443,
-2.12641069184361));
#33633=CARTESIAN_POINT('Ctrl Pts',(97.7497344722237,-0.693740088539389,
-2.12860565052379));
#33634=CARTESIAN_POINT('Ctrl Pts',(97.7301950372407,-0.728881467022591,
-2.13080060920398));
#33635=CARTESIAN_POINT('Ctrl Pts',(97.7092738802521,-0.763117596636286,
-2.13299556788417));
#33636=CARTESIAN_POINT('Ctrl Pts',(97.6805829646373,-0.810068437178112,
-2.1360056965451));
#33637=CARTESIAN_POINT('Ctrl Pts',(97.6491802703056,-0.855497639194756,
-2.13901582520603));
#33638=CARTESIAN_POINT('Ctrl Pts',(97.6152524926459,-0.899074487080088,
-2.14202595386695));
#33639=CARTESIAN_POINT('Ctrl Pts',(97.5813850142069,-0.94257388662803,-2.14503073268108));
#33640=CARTESIAN_POINT('Ctrl Pts',(97.5450016802927,-0.984227052010367,
-2.14803551149521));
#33641=CARTESIAN_POINT('Ctrl Pts',(97.5063329733976,-1.02373130960729,-2.15104029030934));
#33642=CARTESIAN_POINT('Ctrl Pts',(97.4677025227817,-1.0631964842861,-2.15404209639265));
#33643=CARTESIAN_POINT('Ctrl Pts',(97.4267915457187,-1.100516587111,-2.15704390247595));
#33644=CARTESIAN_POINT('Ctrl Pts',(97.3838701777455,-1.1354226452306,-2.16004570855925));
#33645=CARTESIAN_POINT('Ctrl Pts',(97.340974320453,-1.17030795663712,-2.16304573049353));
#33646=CARTESIAN_POINT('Ctrl Pts',(97.2960708495153,-1.20278173467465,-2.16604575242781));
#33647=CARTESIAN_POINT('Ctrl Pts',(97.2494643640091,-1.23261406034128,-2.16904577436209));
#33648=CARTESIAN_POINT('Ctrl Pts',(97.2028671721178,-1.26244043726185,-2.17204519807386));
#33649=CARTESIAN_POINT('Ctrl Pts',(97.1545680846216,-1.28962612330639,-2.17504462178563));
#33650=CARTESIAN_POINT('Ctrl Pts',(97.1049002438924,-1.31398478800708,-2.1780440454974));
#33651=CARTESIAN_POINT('Ctrl Pts',(97.0551867407775,-1.33836584697191,-2.18104622674485));
#33652=CARTESIAN_POINT('Ctrl Pts',(97.0041024455503,-1.35991445901165,-2.18404840799229));
#33653=CARTESIAN_POINT('Ctrl Pts',(96.9520033009044,-1.37849121438824,-2.18705058923974));
#33654=CARTESIAN_POINT('Ctrl Pts',(96.8998804418844,-1.39707642549151,-2.19005413701344));
#33655=CARTESIAN_POINT('Ctrl Pts',(96.8467423201935,-1.41268693425617,-2.19305768478715));
#33656=CARTESIAN_POINT('Ctrl Pts',(96.7929598092032,-1.42523333454619,-2.19606123256085));
#33657=CARTESIAN_POINT('Ctrl Pts',(96.7390757927746,-1.4378034140553,-2.19907044902551));
#33658=CARTESIAN_POINT('Ctrl Pts',(96.6845454791106,-1.44729774186084,-2.20207966549016));
#33659=CARTESIAN_POINT('Ctrl Pts',(96.6297485368579,-1.45367834609177,-2.20508888195482));
#33660=CARTESIAN_POINT('Ctrl Pts',(96.5878266302286,-1.45855976983206,-2.20739105588046));
#33661=CARTESIAN_POINT('Ctrl Pts',(96.5457488678837,-1.46161983639159,-2.2096932298061));
#33662=CARTESIAN_POINT('Ctrl Pts',(96.5036849796955,-1.46286214722424,-2.21199540373174));
#33663=CARTESIAN_POINT('Ctrl Pts',(96.4486857834913,-1.46448648820115,-2.21500553239283));
#33664=CARTESIAN_POINT('Ctrl Pts',(96.3934792952583,-1.46300822420362,-2.21801566105392));
#33665=CARTESIAN_POINT('Ctrl Pts',(96.3384445078446,-1.45840301593534,-2.22102578971501));
#33666=CARTESIAN_POINT('Ctrl Pts',(96.2835075327554,-1.45380599241977,-2.22403056852931));
#33667=CARTESIAN_POINT('Ctrl Pts',(96.2287421749122,-1.44609309713392,-2.2270353473436));
#33668=CARTESIAN_POINT('Ctrl Pts',(96.1745278663474,-1.43529198569194,-2.23004012615789));
#33669=CARTESIAN_POINT('Ctrl Pts',(96.1203671938593,-1.42450156016029,-2.23304193224136));
#33670=CARTESIAN_POINT('Ctrl Pts',(96.0667570060808,-1.41062907351305,-2.23604373832482));
#33671=CARTESIAN_POINT('Ctrl Pts',(96.0140701760109,-1.3937538058223,-2.23904554440829));
#33672=CARTESIAN_POINT('Ctrl Pts',(95.9614146608074,-1.37688856809069,-2.24204556634273));
#33673=CARTESIAN_POINT('Ctrl Pts',(95.9096819174873,-1.35702424753404,-2.24504558827717));
#33674=CARTESIAN_POINT('Ctrl Pts',(95.8592309411424,-1.33429032723671,-2.24804561021161));
#33675=CARTESIAN_POINT('Ctrl Pts',(95.8087900250273,-1.31156094022055,-2.25104503392354));
#33676=CARTESIAN_POINT('Ctrl Pts',(95.7596308495122,-1.28596330670364,-2.25404445763547));
#33677=CARTESIAN_POINT('Ctrl Pts',(95.7120914990629,-1.25767463215221,-2.2570438813474));
#33678=CARTESIAN_POINT('Ctrl Pts',(95.6645084430664,-1.22935995026184,-2.26004606259499));
#33679=CARTESIAN_POINT('Ctrl Pts',(95.6185486421705,-1.1983495552044,-2.26304824384259));
#33680=CARTESIAN_POINT('Ctrl Pts',(95.5745233414731,-1.16486538563163,-2.26605042509019));
#33681=CARTESIAN_POINT('Ctrl Pts',(95.5304780014361,-1.13136597480818,-2.26905397286404));
#33682=CARTESIAN_POINT('Ctrl Pts',(95.488369319128,-1.09539088849361,-2.2720575206379));
#33683=CARTESIAN_POINT('Ctrl Pts',(95.4484748183483,-1.05720189195612,-2.27506106841175));
#33684=CARTESIAN_POINT('Ctrl Pts',(95.4085050234125,-1.01894082011465,-2.27807028487655));
#33685=CARTESIAN_POINT('Ctrl Pts',(95.3707581190338,-0.978457878288022,
-2.28107950134135));
#33686=CARTESIAN_POINT('Ctrl Pts',(95.3354733571345,-0.936050301504515,
-2.28408871780615));
#33687=CARTESIAN_POINT('Ctrl Pts',(95.3084790681816,-0.903606767245913,
-2.28639089173054));
#33688=CARTESIAN_POINT('Ctrl Pts',(95.2829250559329,-0.870037517218534,
-2.28869306565492));
#33689=CARTESIAN_POINT('Ctrl Pts',(95.2589010438097,-0.835486672578428,
-2.2909952395793));
#33690=CARTESIAN_POINT('Ctrl Pts',(95.2274892696218,-0.790310899095273,
-2.29400536824071));
#33691=CARTESIAN_POINT('Ctrl Pts',(95.1985627470502,-0.743266261780503,
-2.29701549690211));
#33692=CARTESIAN_POINT('Ctrl Pts',(95.172348941115,-0.694656878448467,-2.30002562556351));
#33693=CARTESIAN_POINT('Ctrl Pts',(95.1461817244992,-0.646133887687202,
-2.30303040437812));
#33694=CARTESIAN_POINT('Ctrl Pts',(95.1227179053385,-0.596052130884527,
-2.30603518319273));
#33695=CARTESIAN_POINT('Ctrl Pts',(95.1021416414848,-0.544744503498396,
-2.30903996200734));
#33696=CARTESIAN_POINT('Ctrl Pts',(95.0815857344353,-0.493487636509195,
-2.31204176809113));
#33697=CARTESIAN_POINT('Ctrl Pts',(95.0639119192025,-0.441007789184984,
-2.31504357417491));
#33698=CARTESIAN_POINT('Ctrl Pts',(95.0492575329352,-0.387660571017612,
-2.3180453802587));
#33699=CARTESIAN_POINT('Ctrl Pts',(95.0346118566272,-0.334345060223814,
-2.32104540219347));
#33700=CARTESIAN_POINT('Ctrl Pts',(95.0229821918346,-0.280163708634643,
-2.32404542412824));
#33701=CARTESIAN_POINT('Ctrl Pts',(95.0144562464984,-0.225487933350093,
-2.32704544606301));
#33702=CARTESIAN_POINT('Ctrl Pts',(95.0059320012873,-0.170823060745626,
-2.33004486977527));
#33703=CARTESIAN_POINT('Ctrl Pts',(95.0005103277463,-0.115664481760865,
-2.33304429348754));
#33704=CARTESIAN_POINT('Ctrl Pts',(94.9982275395534,-0.0603921756059455,
-2.3360437171998));
#33705=CARTESIAN_POINT('Ctrl Pts',(94.9959426526674,-0.00506905457112808,
-2.33904589844773));
#33706=CARTESIAN_POINT('Ctrl Pts',(94.9968024383236,0.050367473722371,-2.34204807969566));
#33707=CARTESIAN_POINT('Ctrl Pts',(95.000791080028,0.105535466720293,-2.34505026094359));
#33708=CARTESIAN_POINT('Ctrl Pts',(95.0047815372734,0.160728570963964,-2.34805380871778));
#33709=CARTESIAN_POINT('Ctrl Pts',(95.0119036215515,0.215652371608006,-2.35105735649198));
#33710=CARTESIAN_POINT('Ctrl Pts',(95.0220897353198,0.269931407486378,-2.35406090426617));
#33711=CARTESIAN_POINT('Ctrl Pts',(95.0322950736635,0.324312885910187,-2.3570701207313));
#33712=CARTESIAN_POINT('Ctrl Pts',(95.0455758665916,0.378046654705103,-2.36007933719644));
#33713=CARTESIAN_POINT('Ctrl Pts',(95.0618138980795,0.430769925894763,-2.36308855366158));
#33714=CARTESIAN_POINT('Ctrl Pts',(95.0742366576468,0.471105389098869,-2.36539072758334));
#33715=CARTESIAN_POINT('Ctrl Pts',(95.0883891959999,0.510849668479265,-2.3676929015051));
#33716=CARTESIAN_POINT('Ctrl Pts',(95.1041998323173,0.549848871022576,-2.36999507542686));
#33717=CARTESIAN_POINT('Ctrl Pts',(95.1248724883147,0.60084094257259,-2.37300520408805));
#33718=CARTESIAN_POINT('Ctrl Pts',(95.1484682997943,0.650772688870073,-2.37601533274923));
#33719=CARTESIAN_POINT('Ctrl Pts',(95.1748568458959,0.699287433059006,-2.37902546141042));
#33720=CARTESIAN_POINT('Ctrl Pts',(95.2011984921157,0.747715952877547,-2.38203024022481));
#33721=CARTESIAN_POINT('Ctrl Pts',(95.2303227726028,0.79473200821732,-2.3850350190392));
#33722=CARTESIAN_POINT('Ctrl Pts',(95.2620515015793,0.839999469149773,-2.3880397978536));
#33723=CARTESIAN_POINT('Ctrl Pts',(95.2937488402351,0.885222145429272,-2.39104160393717));
#33724=CARTESIAN_POINT('Ctrl Pts',(95.32804522149,0.928699223901158,-2.39404341002074));
#33725=CARTESIAN_POINT('Ctrl Pts',(95.3647178533028,0.970121377376899,-2.39704521610431));
#33726=CARTESIAN_POINT('Ctrl Pts',(95.4013686884245,1.0115189112428,-2.40004523803885));
#33727=CARTESIAN_POINT('Ctrl Pts',(95.4403926253668,1.05086354630681,-2.4030452599734));
#33728=CARTESIAN_POINT('Ctrl Pts',(95.4815265155872,1.08787888396257,-2.40604528190795));
#33729=CARTESIAN_POINT('Ctrl Pts',(95.5226522034612,1.12488684053629,-2.40904470561999));
#33730=CARTESIAN_POINT('Ctrl Pts',(95.5658866166968,1.15956606906539,-2.41204412933204));
#33731=CARTESIAN_POINT('Ctrl Pts',(95.61093135413,1.19167853671865,-2.41504355304408));
#33732=CARTESIAN_POINT('Ctrl Pts',(95.6560175036751,1.22382052713472,-2.41804573429179));
#33733=CARTESIAN_POINT('Ctrl Pts',(95.7029168715836,1.25339073494567,-2.42104791553949));
#33734=CARTESIAN_POINT('Ctrl Pts',(95.7513009286169,1.28019371497873,-2.4240500967872));
#33735=CARTESIAN_POINT('Ctrl Pts',(95.7997070089989,1.3070088951333,-2.42705364456116));
#33736=CARTESIAN_POINT('Ctrl Pts',(95.8495986490855,1.33105410693755,-2.43005719233513));
#33737=CARTESIAN_POINT('Ctrl Pts',(95.9006244550134,1.35218081464536,-2.4330607401091));
#33738=CARTESIAN_POINT('Ctrl Pts',(95.9517465635629,1.37334739545852,-2.43606995657401));
#33739=CARTESIAN_POINT('Ctrl Pts',(96.0040066141782,1.39158429428956,-2.43907917303893));
#33740=CARTESIAN_POINT('Ctrl Pts',(96.0570361693938,1.4067922943146,-2.44208838950384));
#33741=CARTESIAN_POINT('Ctrl Pts',(96.0976059524642,1.41842703760901,-2.44439056342737));
#33742=CARTESIAN_POINT('Ctrl Pts',(96.1386257475107,1.42829002409361,-2.4466927373509));
#33743=CARTESIAN_POINT('Ctrl Pts',(96.1799274988729,1.4363572018471,-2.44899491127443));
#33744=CARTESIAN_POINT('Ctrl Pts',(96.2339301892273,1.44690516380721,-2.45200503993565));
#33745=CARTESIAN_POINT('Ctrl Pts',(96.2886420293264,1.45442554682468,-2.45501516859687));
#33746=CARTESIAN_POINT('Ctrl Pts',(96.3436930312583,1.45883269504587,-2.45802529725809));
#33747=CARTESIAN_POINT('Ctrl Pts',(96.3986461920481,1.46323201052287,-2.46103007607252));
#33748=CARTESIAN_POINT('Ctrl Pts',(96.4539367962634,1.46452902986565,-2.46403485488695));
#33749=CARTESIAN_POINT('Ctrl Pts',(96.5091859660334,1.46268932838521,-2.46703963370137));
#33750=CARTESIAN_POINT('Ctrl Pts',(96.5643804759032,1.4608514469846,-2.47004143978498));
#33751=CARTESIAN_POINT('Ctrl Pts',(96.6195331073032,1.45588300966985,-2.47304324586858));
#33752=CARTESIAN_POINT('Ctrl Pts',(96.6742630576916,1.44780159560973,-2.47604505195219));
#33753=CARTESIAN_POINT('Ctrl Pts',(96.7289604788675,1.43972498480692,-2.47904507388677));
#33754=CARTESIAN_POINT('Ctrl Pts',(96.7832351955663,1.42853914151569,-2.48204509582136));
#33755=CARTESIAN_POINT('Ctrl Pts',(96.8367119331856,1.41431343660905,-2.48504511775594));
#33756=CARTESIAN_POINT('Ctrl Pts',(96.8901780072203,1.40009056839394,-2.48804454146802));
#33757=CARTESIAN_POINT('Ctrl Pts',(96.9428459081041,1.38282917807458,-2.4910439651801));
#33758=CARTESIAN_POINT('Ctrl Pts',(96.9943532317103,1.36264912445198,-2.49404338889218));
#33759=CARTESIAN_POINT('Ctrl Pts',(97.0459079088402,1.34245051819298,-2.49704557013992));
#33760=CARTESIAN_POINT('Ctrl Pts',(97.0962993842198,1.31932808083586,-2.50004775138766));
#33761=CARTESIAN_POINT('Ctrl Pts',(97.1451844601707,1.29345017398454,-2.50304993263541));
#33762=CARTESIAN_POINT('Ctrl Pts',(97.194091787523,1.26756048808447,-2.50605348040941));
#33763=CARTESIAN_POINT('Ctrl Pts',(97.2414908958246,1.23891310611822,-2.50905702818341));
#33764=CARTESIAN_POINT('Ctrl Pts',(97.2870653821634,1.2077211705546,-2.51206057595742));
#33765=CARTESIAN_POINT('Ctrl Pts',(97.3327258826753,1.17647036546201,-2.51506979242237));
#33766=CARTESIAN_POINT('Ctrl Pts',(97.3765544627584,1.14266573652958,-2.51807900888731));
#33767=CARTESIAN_POINT('Ctrl Pts',(97.4182667128676,1.10656164836748,-2.52108822535226));
#33768=CARTESIAN_POINT('Ctrl Pts',(97.450178293706,1.07894054125959,-2.5233903992755));
#33769=CARTESIAN_POINT('Ctrl Pts',(97.4808518653103,1.04997445604528,-2.52569257319875));
#33770=CARTESIAN_POINT('Ctrl Pts',(97.5101754585963,1.0197910019875,-2.52799474712199));
#33771=CARTESIAN_POINT('Ctrl Pts',(97.5479955087937,0.980861947950277,-2.53096397168089));
#33772=CARTESIAN_POINT('Ctrl Pts',(97.583736810613,0.939733435353951,-2.53393319623979));
#33773=CARTESIAN_POINT('Ctrl Pts',(97.6171288425952,0.896659300724986,-2.5369024207987));
#33774=CARTESIAN_POINT('Ctrl Pts',(97.650473055172,0.853646850856692,-2.53986739324882));
#33775=CARTESIAN_POINT('Ctrl Pts',(97.6814743257114,0.808694718016118,-2.54283236569893));
#33776=CARTESIAN_POINT('Ctrl Pts',(97.7098994920492,0.762092878674607,-2.54579733814905));
#33777=CARTESIAN_POINT('Ctrl Pts',(97.7382959113231,0.7155381689097,-2.54875931205023));
#33778=CARTESIAN_POINT('Ctrl Pts',(97.7641211034871,0.667337517991422,-2.5517212859514));
#33779=CARTESIAN_POINT('Ctrl Pts',(97.7871842221689,0.617811198096895,-2.55468325985257));
#33780=CARTESIAN_POINT('Ctrl Pts',(97.8102422235838,0.568295867149768,-2.55764457654813));
#33781=CARTESIAN_POINT('Ctrl Pts',(97.8305391172134,0.517455933024783,-2.56060589324369));
#33782=CARTESIAN_POINT('Ctrl Pts',(97.8479302400693,0.465635819404298,-2.56356720993925));
#33783=CARTESIAN_POINT('Ctrl Pts',(97.8653178582868,0.413826148511774,-2.56652792987378));
#33784=CARTESIAN_POINT('Ctrl Pts',(97.8798007010528,0.361037207951688,-2.5694886498083));
#33785=CARTESIAN_POINT('Ctrl Pts',(97.8912835084281,0.307630114886793,-2.57244936974282));
#33786=CARTESIAN_POINT('Ctrl Pts',(97.9027779699189,0.254168817966135,-2.57541309456728));
#33787=CARTESIAN_POINT('Ctrl Pts',(97.9112662065411,0.20008864975942,-2.57837681939174));
#33788=CARTESIAN_POINT('Ctrl Pts',(97.916704153813,0.145760863898986,-2.5813405442162));
#33789=CARTESIAN_POINT('Ctrl Pts',(97.9215997454083,0.0968514797968769,
-2.58400868085229));
#33790=CARTESIAN_POINT('Ctrl Pts',(97.9240238177501,0.0477418006625273,
-2.58667681748839));
#33791=CARTESIAN_POINT('Ctrl Pts',(97.9239803753015,-0.00129649685740054,
-2.58934495412449));
#33792=CARTESIAN_POINT('Origin',(96.460480949577,-8.32667268468867E-16,
1.18130019239114E-14));
#33793=CARTESIAN_POINT('',(97.9239807388018,0.000785454741002297,-3.16065504587761));
#33794=CARTESIAN_POINT('',(97.9239807053004,0.000845575209100124,-3.08934495419159));
#33795=CARTESIAN_POINT('',(97.923980949577,-1.01189432752408E-15,1.19922289829666E-14));
#33796=CARTESIAN_POINT('Ctrl Pts',(97.9239807388014,0.000785455376517466,
-3.16065504584289));
#33797=CARTESIAN_POINT('Ctrl Pts',(97.9239557214913,0.0473989602722419,
-3.15810845262082));
#33798=CARTESIAN_POINT('Ctrl Pts',(97.9217038592401,0.0939508689700229,
-3.15556185939875));
#33799=CARTESIAN_POINT('Ctrl Pts',(97.9172417156336,0.140286565566206,-3.15301526617668));
#33800=CARTESIAN_POINT('Ctrl Pts',(97.9119673646911,0.195056368279042,-3.15000513751544));
#33801=CARTESIAN_POINT('Ctrl Pts',(97.9035888686244,0.249643385155502,-3.1469950088542));
#33802=CARTESIAN_POINT('Ctrl Pts',(97.8921295296342,0.303668558168621,-3.14398488019296));
#33803=CARTESIAN_POINT('Ctrl Pts',(97.8806905571183,0.357597713226631,-3.14098010137851));
#33804=CARTESIAN_POINT('Ctrl Pts',(97.866181716592,0.4109664936164,-3.13797532256407));
#33805=CARTESIAN_POINT('Ctrl Pts',(97.8486779510305,0.463401915356002,-3.13497054374962));
#33806=CARTESIAN_POINT('Ctrl Pts',(97.8311915025451,0.515785460932966,-3.131968737666));
#33807=CARTESIAN_POINT('Ctrl Pts',(97.8107161649499,0.567236978598564,-3.12896693158238));
#33808=CARTESIAN_POINT('Ctrl Pts',(97.7873772782786,0.617396455187672,-3.12596512549876));
#33809=CARTESIAN_POINT('Ctrl Pts',(97.7640522632734,0.667526119064526,-3.12296510356416));
#33810=CARTESIAN_POINT('Ctrl Pts',(97.7378672949656,0.716364786098106,-3.11996508162956));
#33811=CARTESIAN_POINT('Ctrl Pts',(97.7089957838616,0.76357249725958,-3.11696505969495));
#33812=CARTESIAN_POINT('Ctrl Pts',(97.6801300299115,0.810770794918064,-3.11396563598286));
#33813=CARTESIAN_POINT('Ctrl Pts',(97.6485790724551,0.856338332297967,-3.11096621227077));
#33814=CARTESIAN_POINT('Ctrl Pts',(97.6145610508622,0.899961871313187,-3.10796678855868));
#33815=CARTESIAN_POINT('Ctrl Pts',(97.5805117546256,0.943625515854127,-3.10496460731091));
#33816=CARTESIAN_POINT('Ctrl Pts',(97.5439911883238,0.985341174032972,-3.10196242606315));
#33817=CARTESIAN_POINT('Ctrl Pts',(97.5052585122345,1.02482783654984,-3.09896024481539));
#33818=CARTESIAN_POINT('Ctrl Pts',(97.4665082058909,1.06433247251896,-3.09595669704137));
#33819=CARTESIAN_POINT('Ctrl Pts',(97.4255441738651,1.10160573426969,-3.09295314926735));
#33820=CARTESIAN_POINT('Ctrl Pts',(97.3826608677621,1.13640505476529,-3.08994960149332));
#33821=CARTESIAN_POINT('Ctrl Pts',(97.3396966266358,1.17127005312182,-3.08694038502836));
#33822=CARTESIAN_POINT('Ctrl Pts',(97.2948063046736,1.20365147315747,-3.08393116856339));
#33823=CARTESIAN_POINT('Ctrl Pts',(97.2483147524996,1.23334915939184,-3.08092195209842));
#33824=CARTESIAN_POINT('Ctrl Pts',(97.2127468097126,1.25606910646815,-3.07861977817532));
#33825=CARTESIAN_POINT('Ctrl Pts',(97.176242331798,1.27721916981499,-3.07631760425222));
#33826=CARTESIAN_POINT('Ctrl Pts',(97.1389555392849,1.2967283759989,-3.07401543032911));
#33827=CARTESIAN_POINT('Ctrl Pts',(97.0902024708467,1.32223697033355,-3.07100530166787));
#33828=CARTESIAN_POINT('Ctrl Pts',(97.0399063977555,1.34504588612147,-3.06799517300663));
#33829=CARTESIAN_POINT('Ctrl Pts',(96.9883975235416,1.36496752376511,-3.06498504434539));
#33830=CARTESIAN_POINT('Ctrl Pts',(96.9369801951108,1.38485375504535,-3.06198026553094));
#33831=CARTESIAN_POINT('Ctrl Pts',(96.8843548317162,1.40186270272879,-3.0589754867165));
#33832=CARTESIAN_POINT('Ctrl Pts',(96.8308747660283,1.41585333659058,-3.05597070790205));
#33833=CARTESIAN_POINT('Ctrl Pts',(96.7774476100051,1.42983012903804,-3.05296890181843));
#33834=CARTESIAN_POINT('Ctrl Pts',(96.7231679351649,1.4407943900243,-3.04996709573481));
#33835=CARTESIAN_POINT('Ctrl Pts',(96.6684057475248,1.4486543854206,-3.04696528965118));
#33836=CARTESIAN_POINT('Ctrl Pts',(96.6136761082576,1.45650970916167,-3.04396526771658));
#33837=CARTESIAN_POINT('Ctrl Pts',(96.5584650463337,1.46126434943487,-3.04096524578198));
#33838=CARTESIAN_POINT('Ctrl Pts',(96.503152037409,1.46287778992752,-3.03796522384738));
#33839=CARTESIAN_POINT('Ctrl Pts',(96.4478500582326,1.46449090869039,-3.03496580013529));
#33840=CARTESIAN_POINT('Ctrl Pts',(96.3924467000232,1.46296405623548,-3.03196637642319));
#33841=CARTESIAN_POINT('Ctrl Pts',(96.3373234986036,1.45830877809527,-3.0289669527111));
#33842=CARTESIAN_POINT('Ctrl Pts',(96.2821496193843,1.45364922010109,-3.02596477146334));
#33843=CARTESIAN_POINT('Ctrl Pts',(96.2272569389069,1.44585553481691,-3.02296259021558));
#33844=CARTESIAN_POINT('Ctrl Pts',(96.1730224141812,1.43499123357187,-3.01996040896782));
#33845=CARTESIAN_POINT('Ctrl Pts',(96.1187632031039,1.42412198713808,-3.01695686119379));
#33846=CARTESIAN_POINT('Ctrl Pts',(96.0651632569648,1.41017947175422,-3.01395331341977));
#33847=CARTESIAN_POINT('Ctrl Pts',(96.0125866193864,1.39327776088728,-3.01094976564575));
#33848=CARTESIAN_POINT('Ctrl Pts',(95.9599107522528,1.37634415088552,-3.00794054918078));
#33849=CARTESIAN_POINT('Ctrl Pts',(95.9082625457957,1.35644037890225,-3.00493133271581));
#33850=CARTESIAN_POINT('Ctrl Pts',(95.8579871327224,1.33372915190904,-3.00192211625084));
#33851=CARTESIAN_POINT('Ctrl Pts',(95.8195243812728,1.31635413247992,-2.99961994232775));
#33852=CARTESIAN_POINT('Ctrl Pts',(95.7818647305796,1.2973369613695,-2.99731776840465));
#33853=CARTESIAN_POINT('Ctrl Pts',(95.7451518882949,1.27676802281594,-2.99501559448156));
#33854=CARTESIAN_POINT('Ctrl Pts',(95.6971492688196,1.24987381171829,-2.99200546582032));
#33855=CARTESIAN_POINT('Ctrl Pts',(95.6505646110984,1.22021219893694,-2.98899533715909));
#33856=CARTESIAN_POINT('Ctrl Pts',(95.6057354567556,1.18795723513156,-2.98598520849785));
#33857=CARTESIAN_POINT('Ctrl Pts',(95.5609859764515,1.15575959748532,-2.98298042968341));
#33858=CARTESIAN_POINT('Ctrl Pts',(95.517986233034,1.12097806158295,-2.97997565086897));
#33859=CARTESIAN_POINT('Ctrl Pts',(95.4770474026959,1.08383149468393,-2.97697087205453));
#33860=CARTESIAN_POINT('Ctrl Pts',(95.4361490745479,1.04672167815864,-2.97396906597091));
#33861=CARTESIAN_POINT('Ctrl Pts',(95.3973080096399,1.007251818816,-2.97096725988729));
#33862=CARTESIAN_POINT('Ctrl Pts',(95.3608032076086,0.965681683485441,-2.96796545380367));
#33863=CARTESIAN_POINT('Ctrl Pts',(95.3243201025174,0.924136255718989,-2.96496543186907));
#33864=CARTESIAN_POINT('Ctrl Pts',(95.2901708558294,0.880493422246292,-2.96196540993448));
#33865=CARTESIAN_POINT('Ctrl Pts',(95.2585967450554,0.835048866187807,-2.95896538799988));
#33866=CARTESIAN_POINT('Ctrl Pts',(95.22702893035,0.78961337204849,-2.95596596428779));
#33867=CARTESIAN_POINT('Ctrl Pts',(95.1980355329397,0.742377302293595,-2.9529665405757));
#33868=CARTESIAN_POINT('Ctrl Pts',(95.171815352806,0.693666511876485,-2.94996711686361));
#33869=CARTESIAN_POINT('Ctrl Pts',(95.1455710670144,0.644910938942837,-2.94696493561586));
#33870=CARTESIAN_POINT('Ctrl Pts',(95.1221053430655,0.594678402675534,-2.9439627543681));
#33871=CARTESIAN_POINT('Ctrl Pts',(95.1015709563422,0.543319317056278,-2.94096057312034));
#33872=CARTESIAN_POINT('Ctrl Pts',(95.0810272228218,0.491936853921341,-2.93795702534632));
#33873=CARTESIAN_POINT('Ctrl Pts',(95.0634176545321,0.4394273208251,-2.93495347757231));
#33874=CARTESIAN_POINT('Ctrl Pts',(95.0488456238805,0.386157943393404,-2.93194992979829));
#33875=CARTESIAN_POINT('Ctrl Pts',(95.0342460909735,0.332788028976673,-2.92894071333332));
#33876=CARTESIAN_POINT('Ctrl Pts',(95.0226956584212,0.278655923186859,-2.92593149686836));
#33877=CARTESIAN_POINT('Ctrl Pts',(95.0142466339124,0.224139586405414,-2.9229222804034));
#33878=CARTESIAN_POINT('Ctrl Pts',(95.0077827838947,0.182432354511517,-2.92062010648026));
#33879=CARTESIAN_POINT('Ctrl Pts',(95.003133091206,0.140500475882642,-2.91831793255712));
#33880=CARTESIAN_POINT('Ctrl Pts',(95.0003003779112,0.0985136951381245,
-2.91601575863398));
#33881=CARTESIAN_POINT('Ctrl Pts',(94.9965965606662,0.0436153180685221,
-2.91300562997275));
#33882=CARTESIAN_POINT('Ctrl Pts',(94.9959852855462,-0.0116075752867995,
-2.90999550131151));
#33883=CARTESIAN_POINT('Ctrl Pts',(94.998505211858,-0.0667771841359344,
-2.90698537265027));
#33884=CARTESIAN_POINT('Ctrl Pts',(95.0010206595508,-0.121848741045036,
-2.90398059383583));
#33885=CARTESIAN_POINT('Ctrl Pts',(95.0066562409394,-0.176866678084867,
-2.90097581502138));
#33886=CARTESIAN_POINT('Ctrl Pts',(95.015398674254,-0.231450788607809,-2.89797103620694));
#33887=CARTESIAN_POINT('Ctrl Pts',(95.0241324583791,-0.285980897196529,
-2.89496923012332));
#33888=CARTESIAN_POINT('Ctrl Pts',(95.0359669224377,-0.340077510585632,
-2.8919674240397));
#33889=CARTESIAN_POINT('Ctrl Pts',(95.0508369490254,-0.393365023494636,
-2.88896561795608));
#33890=CARTESIAN_POINT('Ctrl Pts',(95.0656981374862,-0.446620864516341,
-2.88596559602148));
#33891=CARTESIAN_POINT('Ctrl Pts',(95.0835911707428,-0.499068050558755,
-2.88296557408688));
#33892=CARTESIAN_POINT('Ctrl Pts',(95.1044002393092,-0.550342945116653,
-2.87996555215228));
#33893=CARTESIAN_POINT('Ctrl Pts',(95.1252051584216,-0.601607615150639,
-2.87696612844019));
#33894=CARTESIAN_POINT('Ctrl Pts',(95.1489247595747,-0.651699968862824,
-2.8739667047281));
#33895=CARTESIAN_POINT('Ctrl Pts',(95.1753947540048,-0.700275460051026,
-2.87096728101601));
#33896=CARTESIAN_POINT('Ctrl Pts',(95.2018890837609,-0.74889560936772,-2.86796509976825));
#33897=CARTESIAN_POINT('Ctrl Pts',(95.2311386053416,-0.795995645329472,
-2.86496291852049));
#33898=CARTESIAN_POINT('Ctrl Pts',(95.2629333134761,-0.841256149617383,
-2.86196073727273));
#33899=CARTESIAN_POINT('Ctrl Pts',(95.2947424938559,-0.886537255482135,
-2.85895718949871));
#33900=CARTESIAN_POINT('Ctrl Pts',(95.3290988420247,-0.929976745601661,
-2.85595364172469));
#33901=CARTESIAN_POINT('Ctrl Pts',(95.3657512789154,-0.971287392162184,
-2.85295009395067));
#33902=CARTESIAN_POINT('Ctrl Pts',(95.4024728911124,-1.01267600561579,-2.84994087748571));
#33903=CARTESIAN_POINT('Ctrl Pts',(95.4414988755614,-1.05192737383626,-2.84693166102074));
#33904=CARTESIAN_POINT('Ctrl Pts',(95.4825412609867,-1.08879117165776,-2.84392244455577));
#33905=CARTESIAN_POINT('Ctrl Pts',(95.5139403678866,-1.11699348778878,-2.84162027063266));
#33906=CARTESIAN_POINT('Ctrl Pts',(95.5465188709158,-1.1437991444267,-2.83931809670954));
#33907=CARTESIAN_POINT('Ctrl Pts',(95.5801361463526,-1.16911303022238,-2.83701592278643));
#33908=CARTESIAN_POINT('Ctrl Pts',(95.6240912634221,-1.20221133456672,-2.83400579412519));
#33909=CARTESIAN_POINT('Ctrl Pts',(95.6700079244915,-1.23289686607654,-2.83099566546395));
#33910=CARTESIAN_POINT('Ctrl Pts',(95.7175908345235,-1.26093081767231,-2.82798553680271));
#33911=CARTESIAN_POINT('Ctrl Pts',(95.7650891763169,-1.28891494503698,-2.82498075798827));
#33912=CARTESIAN_POINT('Ctrl Pts',(95.8142474388297,-1.31425657877337,-2.82197597917382));
#33913=CARTESIAN_POINT('Ctrl Pts',(95.8647399316551,-1.33675909930151,-2.81897120035938));
#33914=CARTESIAN_POINT('Ctrl Pts',(95.9151824705241,-1.35923935731366,-2.81596939427576));
#33915=CARTESIAN_POINT('Ctrl Pts',(95.9669561448404,-1.37888585235778,-2.81296758819214));
#33916=CARTESIAN_POINT('Ctrl Pts',(96.0197107951788,-1.39554789276175,-2.80996578210852));
#33917=CARTESIAN_POINT('Ctrl Pts',(96.0724340903412,-1.41220002994005,-2.80696576017392));
#33918=CARTESIAN_POINT('Ctrl Pts',(96.12613670329,-1.42587106959966,-2.80396573823932));
#33919=CARTESIAN_POINT('Ctrl Pts',(96.1804508008166,-1.43645931574313,-2.80096571630472));
#33920=CARTESIAN_POINT('Ctrl Pts',(96.2347540677838,-1.44704545052631,-2.79796629259263));
#33921=CARTESIAN_POINT('Ctrl Pts',(96.2896680591062,-1.45454991162158,-2.79496686888053));
#33922=CARTESIAN_POINT('Ctrl Pts',(96.3448144413312,-1.45892203659765,-2.79196744516844));
#33923=CARTESIAN_POINT('Ctrl Pts',(96.4000115226672,-1.46329818110938,-2.78896526392068));
#33924=CARTESIAN_POINT('Ctrl Pts',(96.4554408941549,-1.46453619434792,-2.78596308267292));
#33925=CARTESIAN_POINT('Ctrl Pts',(96.5107202883001,-1.46263743246393,-2.78296090142516));
#33926=CARTESIAN_POINT('Ctrl Pts',(96.5660248443985,-1.46073780630567,-2.77995735365114));
#33927=CARTESIAN_POINT('Ctrl Pts',(96.6211787602276,-1.45569860695866,-2.77695380587712));
#33928=CARTESIAN_POINT('Ctrl Pts',(96.6758042861467,-1.44757317974896,-2.7739502581031));
#33929=CARTESIAN_POINT('Ctrl Pts',(96.7305329085528,-1.43943241716285,-2.77094104163813));
#33930=CARTESIAN_POINT('Ctrl Pts',(96.7847306305091,-1.42819389839289,-2.76793182517316));
#33931=CARTESIAN_POINT('Ctrl Pts',(96.8380304515775,-1.41396203044465,-2.7649226087082));
#33932=CARTESIAN_POINT('Ctrl Pts',(96.8788069990937,-1.40307406819633,-2.76262043478509));
#33933=CARTESIAN_POINT('Ctrl Pts',(96.9190582241114,-1.39043520068447,-2.76031826086198));
#33934=CARTESIAN_POINT('Ctrl Pts',(96.9586276320664,-1.37611123559282,-2.75801608693887));
#33935=CARTESIAN_POINT('Ctrl Pts',(97.0103652561433,-1.3573824256484,-2.75500595827763));
#33936=CARTESIAN_POINT('Ctrl Pts',(97.0611538979779,-1.33569244020793,-2.75199582961639));
#33937=CARTESIAN_POINT('Ctrl Pts',(97.1106322021646,-1.31115811356172,-2.74898570095516));
#33938=CARTESIAN_POINT('Ctrl Pts',(97.1600225694634,-1.286667391327,-2.74598092214071));
#33939=CARTESIAN_POINT('Ctrl Pts',(97.208106751396,-1.25934259267139,-2.74297614332627));
#33940=CARTESIAN_POINT('Ctrl Pts',(97.254542117813,-1.22934905990921,-2.73997136451183));
#33941=CARTESIAN_POINT('Ctrl Pts',(97.300931544128,-1.19938520077857,-2.73696955842821));
#33942=CARTESIAN_POINT('Ctrl Pts',(97.3456749448753,-1.16675812292461,-2.7339677523446));
#33943=CARTESIAN_POINT('Ctrl Pts',(97.3884547859886,-1.13167875695163,-2.73096594626098));
#33944=CARTESIAN_POINT('Ctrl Pts',(97.4312092005388,-1.09662024069868,-2.72796592432638));
#33945=CARTESIAN_POINT('Ctrl Pts',(97.472001961081,-1.05911265946188,-2.72496590239178));
#33946=CARTESIAN_POINT('Ctrl Pts',(97.5105469118594,-1.01940851715887,-2.72196588045719));
#33947=CARTESIAN_POINT('Ctrl Pts',(97.5490841765415,-0.979712292101846,
-2.7189664567451));
#33948=CARTESIAN_POINT('Ctrl Pts',(97.5853741539633,-0.937820754555385,
-2.71596703303301));
#33949=CARTESIAN_POINT('Ctrl Pts',(97.6191676930618,-0.894023087214543,
-2.71296760932092));
#33950=CARTESIAN_POINT('Ctrl Pts',(97.6529923004249,-0.85018515426221,-2.70996542807316));
#33951=CARTESIAN_POINT('Ctrl Pts',(97.6843155608173,-0.804438009447671,
-2.70696324682541));
#33952=CARTESIAN_POINT('Ctrl Pts',(97.7129297405936,-0.757102553080593,
-2.70396106557765));
#33953=CARTESIAN_POINT('Ctrl Pts',(97.7415569449093,-0.709745550664548,
-2.70095751780363));
#33954=CARTESIAN_POINT('Ctrl Pts',(97.7674723629326,-0.660799263062575,
-2.69795397002962));
#33955=CARTESIAN_POINT('Ctrl Pts',(97.7905142718888,-0.610609213441926,
-2.6949504222556));
#33956=CARTESIAN_POINT('Ctrl Pts',(97.8135996685704,-0.560324438549256,
-2.69194120579064));
#33957=CARTESIAN_POINT('Ctrl Pts',(97.8338005291566,-0.508791705253196,
-2.68893198932567));
#33958=CARTESIAN_POINT('Ctrl Pts',(97.8510037697259,-0.45637543387556,-2.68592277286071));
#33959=CARTESIAN_POINT('Ctrl Pts',(97.8641649538059,-0.416274838083115,
-2.68362059893757));
#33960=CARTESIAN_POINT('Ctrl Pts',(97.8755726734547,-0.375657526258517,
-2.68131842501444));
#33961=CARTESIAN_POINT('Ctrl Pts',(97.885196536363,-0.334690523871024,-2.67901625109131));
#33962=CARTESIAN_POINT('Ctrl Pts',(97.901927104205,-0.263471594501355,-2.6750140455973));
#33963=CARTESIAN_POINT('Ctrl Pts',(97.9133233497531,-0.190955566274591,
-2.67101184010329));
#33964=CARTESIAN_POINT('Ctrl Pts',(97.9192301652513,-0.117826040286424,
-2.66700963460928));
#33965=CARTESIAN_POINT('Ctrl Pts',(97.9223563901513,-0.079121708801346,
-2.66489143835382));
#33966=CARTESIAN_POINT('Ctrl Pts',(97.9239457051545,-0.0402458655927077,
-2.66277324209836));
#33967=CARTESIAN_POINT('Ctrl Pts',(97.9239803697835,-0.00130271069809296,
-2.6606550458429));
#33968=CARTESIAN_POINT('Ctrl Pts',(97.923980375301,-0.00129649745620706,
-2.58934495415707));
#33969=CARTESIAN_POINT('Ctrl Pts',(97.9239140881349,-0.0761221201656831,
-2.59341615963053));
#33970=CARTESIAN_POINT('Ctrl Pts',(97.918105600398,-0.1506992465285,-2.59748736510399));
#33971=CARTESIAN_POINT('Ctrl Pts',(97.9066901297894,-0.22430170991184,-2.60155857057746));
#33972=CARTESIAN_POINT('Ctrl Pts',(97.9016093545666,-0.257060549658327,
-2.60337057470815));
#33973=CARTESIAN_POINT('Ctrl Pts',(97.8954184794346,-0.289626688431987,
-2.60518257883885));
#33974=CARTESIAN_POINT('Ctrl Pts',(97.8881323183465,-0.321937601485883,
-2.60699458296955));
#33975=CARTESIAN_POINT('Ctrl Pts',(97.8760284373731,-0.375612978824297,
-2.61000471163078));
#33976=CARTESIAN_POINT('Ctrl Pts',(97.860867868147,-0.42871758077675,-2.61301484029201));
#33977=CARTESIAN_POINT('Ctrl Pts',(97.842721283876,-0.480878267586448,-2.61602496895323));
#33978=CARTESIAN_POINT('Ctrl Pts',(97.8246069511984,-0.532946250158388,
-2.61902974776767));
#33979=CARTESIAN_POINT('Ctrl Pts',(97.8035173073587,-0.584073152043793,
-2.6220345265821));
#33980=CARTESIAN_POINT('Ctrl Pts',(97.7795734963088,-0.633898338187242,
-2.62503930539654));
#33981=CARTESIAN_POINT('Ctrl Pts',(97.7556533736932,-0.683674230563705,
-2.62804111148015));
#33982=CARTESIAN_POINT('Ctrl Pts',(97.7288849051549,-0.732150484666301,
-2.63104291756376));
#33983=CARTESIAN_POINT('Ctrl Pts',(97.6994376062592,-0.778985656390934,
-2.63404472364737));
#33984=CARTESIAN_POINT('Ctrl Pts',(97.6700078096165,-0.825792991232241,
-2.63704474558196));
#33985=CARTESIAN_POINT('Ctrl Pts',(97.6379026189751,-0.870960730789967,
-2.64004476751655));
#33986=CARTESIAN_POINT('Ctrl Pts',(97.6033367246649,-0.914173357382652,
-2.64304478945114));
#33987=CARTESIAN_POINT('Ctrl Pts',(97.5687777230029,-0.957377367116386,
-2.64604421316322));
#33988=CARTESIAN_POINT('Ctrl Pts',(97.5317593218419,-0.998626625955224,
-2.6490436368753));
#33989=CARTESIAN_POINT('Ctrl Pts',(97.4925372346774,-1.03763773754852,-2.65204306058738));
#33990=CARTESIAN_POINT('Ctrl Pts',(97.4532790884846,-1.07668471420857,-2.65504524183513));
#33991=CARTESIAN_POINT('Ctrl Pts',(97.411813583908,-1.11348905947499,-2.65804742308288));
#33992=CARTESIAN_POINT('Ctrl Pts',(97.3684330879568,-1.14780449746962,-2.66104960433063));
#33993=CARTESIAN_POINT('Ctrl Pts',(97.3250328461669,-1.18213555508986,-2.66405315210464));
#33994=CARTESIAN_POINT('Ctrl Pts',(97.2797163082787,-1.21397514295071,-2.66705669987865));
#33995=CARTESIAN_POINT('Ctrl Pts',(97.2328060309846,-1.24311955122135,-2.67006024765266));
#33996=CARTESIAN_POINT('Ctrl Pts',(97.1858072184368,-1.27231896465781,-2.67306946411761));
#33997=CARTESIAN_POINT('Ctrl Pts',(97.1372091225313,-1.29881278363015,-2.67607868058257));
#33998=CARTESIAN_POINT('Ctrl Pts',(97.0873591380174,-1.32244318851801,-2.67908789704753));
#33999=CARTESIAN_POINT('Ctrl Pts',(97.0492218568493,-1.34052141670828,-2.68139007097072));
#34000=CARTESIAN_POINT('Ctrl Pts',(97.0103523913196,-1.35692467056133,-2.68369224489392));
#34001=CARTESIAN_POINT('Ctrl Pts',(96.9709126475336,-1.37160188528639,-2.68599441881711));
#34002=CARTESIAN_POINT('Ctrl Pts',(96.9193445614017,-1.39079257468909,-2.68900454747835));
#34003=CARTESIAN_POINT('Ctrl Pts',(96.8665843525549,-1.40711133598553,-2.69201467613959));
#34004=CARTESIAN_POINT('Ctrl Pts',(96.812983151145,-1.42041347779078,-2.69502480480083));
#34005=CARTESIAN_POINT('Ctrl Pts',(96.7594772141733,-1.4336919779419,-2.69802958361527));
#34006=CARTESIAN_POINT('Ctrl Pts',(96.7051337592647,-1.44396437212756,-2.70103436242972));
#34007=CARTESIAN_POINT('Ctrl Pts',(96.6503210205638,-1.45113507208934,-2.70403914124416));
#34008=CARTESIAN_POINT('Ctrl Pts',(96.5955625099868,-1.4582986778315,-2.70704094732778));
#34009=CARTESIAN_POINT('Ctrl Pts',(96.5403361564106,-1.46236659995512,-2.7100427534114));
#34010=CARTESIAN_POINT('Ctrl Pts',(96.4850205511011,-1.46329424859016,-2.71304455949502));
#34011=CARTESIAN_POINT('Ctrl Pts',(96.4297378230929,-1.46422134586933,-2.71604458142962));
#34012=CARTESIAN_POINT('Ctrl Pts',(96.3743664754827,-1.46201186024532,-2.71904460336422));
#34013=CARTESIAN_POINT('Ctrl Pts',(96.3192880687736,-1.45667320302477,-2.72204462529882));
#34014=CARTESIAN_POINT('Ctrl Pts',(96.2642206450318,-1.45133561036474,-2.72504404901091));
#34015=CARTESIAN_POINT('Ctrl Pts',(96.209446571541,-1.44287013621926,-2.728043472723));
#34016=CARTESIAN_POINT('Ctrl Pts',(96.155342921222,-1.43133610086925,-2.73104289643509));
#34017=CARTESIAN_POINT('Ctrl Pts',(96.1011895304327,-1.41979146164432,-2.73404507768285));
#34018=CARTESIAN_POINT('Ctrl Pts',(96.0477083118358,-1.40517273537667,-2.73704725893061));
#34019=CARTESIAN_POINT('Ctrl Pts',(95.9952652762933,-1.38759022313189,-2.74004944017837));
#34020=CARTESIAN_POINT('Ctrl Pts',(95.9427983698451,-1.36999970771783,-2.74305298795239));
#34021=CARTESIAN_POINT('Ctrl Pts',(95.8913710797078,-1.34944291345235,-2.74605653572641));
#34022=CARTESIAN_POINT('Ctrl Pts',(95.8413302620576,-1.32607868399435,-2.74906008350042));
#34023=CARTESIAN_POINT('Ctrl Pts',(95.7911950007855,-1.30267035848528,-2.75206929996539));
#34024=CARTESIAN_POINT('Ctrl Pts',(95.7424519055442,-1.27644426392872,-2.75507851643036));
#34025=CARTESIAN_POINT('Ctrl Pts',(95.6954229696403,-1.24760512075542,-2.75808773289532));
#34026=CARTESIAN_POINT('Ctrl Pts',(95.659443906276,-1.22554199430654,-2.76038990681844));
#34027=CARTESIAN_POINT('Ctrl Pts',(95.6244676163366,-1.20195044434708,-2.76269208074156));
#34028=CARTESIAN_POINT('Ctrl Pts',(95.5906253328191,-1.1769381699965,-2.76499425466467));
#34029=CARTESIAN_POINT('Ctrl Pts',(95.5463760141404,-1.1442342273667,-2.76800438332591));
#34030=CARTESIAN_POINT('Ctrl Pts',(95.5038806413711,-1.10896263963651,-2.77101451198715));
#34031=CARTESIAN_POINT('Ctrl Pts',(95.4634522535768,-1.07133842895327,-2.77402464064839));
#34032=CARTESIAN_POINT('Ctrl Pts',(95.423095718419,-1.03378108709376,-2.77702941946283));
#34033=CARTESIAN_POINT('Ctrl Pts',(95.3847992613976,-0.99387977692337,-2.78003419827728));
#34034=CARTESIAN_POINT('Ctrl Pts',(95.3488441419424,-0.951890675399192,
-2.78303897709173));
#34035=CARTESIAN_POINT('Ctrl Pts',(95.3129245941211,-0.909943115134485,
-2.78604078317535));
#34036=CARTESIAN_POINT('Ctrl Pts',(95.2793421370661,-0.865912254390238,
-2.78904258925897));
#34037=CARTESIAN_POINT('Ctrl Pts',(95.2483409767751,-0.82009080981064,-2.79204439534259));
#34038=CARTESIAN_POINT('Ctrl Pts',(95.2173582422879,-0.774296599597015,
-2.79504441727719));
#34039=CARTESIAN_POINT('Ctrl Pts',(95.188954058994,-0.726714351496427,-2.79804443921179));
#34040=CARTESIAN_POINT('Ctrl Pts',(95.1633307028859,-0.677667682208029,
-2.80104446114639));
#34041=CARTESIAN_POINT('Ctrl Pts',(95.1377124562299,-0.628630793121955,
-2.80404388485849));
#34042=CARTESIAN_POINT('Ctrl Pts',(95.114874179924,-0.578130530601198,-2.80704330857058));
#34043=CARTESIAN_POINT('Ctrl Pts',(95.0949722228001,-0.526515115733661,
-2.81004273228267));
#34044=CARTESIAN_POINT('Ctrl Pts',(95.0750519687092,-0.474852247968114,
-2.81304491353043));
#34045=CARTESIAN_POINT('Ctrl Pts',(95.0580736174965,-0.422072673411288,
-2.8160470947782));
#34046=CARTESIAN_POINT('Ctrl Pts',(95.0441447759492,-0.368543204079821,
-2.81904927602596));
#34047=CARTESIAN_POINT('Ctrl Pts',(95.0302095943025,-0.314989369322186,
-2.82205282379998));
#34048=CARTESIAN_POINT('Ctrl Pts',(95.0193267932962,-0.260685478084066,
-2.825056371574));
#34049=CARTESIAN_POINT('Ctrl Pts',(95.0115528579442,-0.206008823299595,
-2.82805991934802));
#34050=CARTESIAN_POINT('Ctrl Pts',(95.0037642505975,-0.151228975530921,
-2.83106913581299));
#34051=CARTESIAN_POINT('Ctrl Pts',(94.9990962747166,-0.0960754863342362,
-2.83407835227796));
#34052=CARTESIAN_POINT('Ctrl Pts',(94.9975534073099,-0.0409298922093092,
-2.83708756874293));
#34053=CARTESIAN_POINT('Ctrl Pts',(94.9963730505121,0.00125874734068382,
-2.83938974266603));
#34054=CARTESIAN_POINT('Ctrl Pts',(94.9970207010016,0.0434426617659435,
-2.84169191658913));
#34055=CARTESIAN_POINT('Ctrl Pts',(94.9994778630617,0.0854530935235066,
-2.84399409051224));
#34056=CARTESIAN_POINT('Ctrl Pts',(95.002690641153,0.140382394665889,-2.84700421917347));
#34057=CARTESIAN_POINT('Ctrl Pts',(95.0090122402784,0.195245670108552,-2.85001434783471));
#34058=CARTESIAN_POINT('Ctrl Pts',(95.018433616919,0.249663253952133,-2.85302447649594));
#34059=CARTESIAN_POINT('Ctrl Pts',(95.0278382491187,0.303984122416013,-2.85602925531038));
#34060=CARTESIAN_POINT('Ctrl Pts',(95.0403316364684,0.357860355081541,-2.85903403412482));
#34061=CARTESIAN_POINT('Ctrl Pts',(95.0558529029206,0.410916415522879,-2.86203881293927));
#34062=CARTESIAN_POINT('Ctrl Pts',(95.071358813651,0.463919985782394,-2.86504061902288));
#34063=CARTESIAN_POINT('Ctrl Pts',(95.089886521821,0.516104486830948,-2.8680424251065));
#34064=CARTESIAN_POINT('Ctrl Pts',(95.1113243025617,0.567105450347909,-2.87104423119012));
#34065=CARTESIAN_POINT('Ctrl Pts',(95.1327493415746,0.618076101007678,-2.87404425312471));
#34066=CARTESIAN_POINT('Ctrl Pts',(95.157080820689,0.667864122528863,-2.87704427505931));
#34067=CARTESIAN_POINT('Ctrl Pts',(95.1841582250178,0.716123280430041,-2.88004429699391));
#34068=CARTESIAN_POINT('Ctrl Pts',(95.2112302299486,0.764372815163445,-2.883043720706));
#34069=CARTESIAN_POINT('Ctrl Pts',(95.2410468144008,0.811093631411541,-2.88604314441809));
#34070=CARTESIAN_POINT('Ctrl Pts',(95.2734017622296,0.855964516184354,-2.88904256813017));
#34071=CARTESIAN_POINT('Ctrl Pts',(95.3057864557467,0.90087665323662,-2.89204474937793));
#34072=CARTESIAN_POINT('Ctrl Pts',(95.3407138654392,0.943935031660171,-2.89504693062569));
#34073=CARTESIAN_POINT('Ctrl Pts',(95.3779355722973,0.984849103228719,-2.89804911187344));
#34074=CARTESIAN_POINT('Ctrl Pts',(95.4151742216501,1.02578179797441,-2.90105265964746));
#34075=CARTESIAN_POINT('Ctrl Pts',(95.4547088722911,1.0645678697017,-2.90405620742148));
#34076=CARTESIAN_POINT('Ctrl Pts',(95.4962543944235,1.10095385931328,-2.90705975519549));
#34077=CARTESIAN_POINT('Ctrl Pts',(95.5378783267371,1.13740852135674,-2.91006897166046));
#34078=CARTESIAN_POINT('Ctrl Pts',(95.581520294585,1.1714537267717,-2.91307818812542));
#34079=CARTESIAN_POINT('Ctrl Pts',(95.6268631971002,1.20287725589749,-2.91608740459038));
#34080=CARTESIAN_POINT('Ctrl Pts',(95.6615523758234,1.22691754351679,-2.91838957851352));
#34081=CARTESIAN_POINT('Ctrl Pts',(95.6972364131332,1.24942424404626,-2.92069175243666));
#34082=CARTESIAN_POINT('Ctrl Pts',(95.7337638640587,1.27032063968737,-2.9229939263598));
#34083=CARTESIAN_POINT('Ctrl Pts',(95.7815240814113,1.29764300608362,-2.92600405502104));
#34084=CARTESIAN_POINT('Ctrl Pts',(95.8309276480725,1.32232557501321,-2.92901418368228));
#34085=CARTESIAN_POINT('Ctrl Pts',(95.8816516422904,1.34416847270948,-2.93202431234352));
#34086=CARTESIAN_POINT('Ctrl Pts',(95.9322854856781,1.3659725494219,-2.93502909115797));
#34087=CARTESIAN_POINT('Ctrl Pts',(95.984234618307,1.38494676331392,-2.93803386997242));
#34088=CARTESIAN_POINT('Ctrl Pts',(96.0371512558801,1.40093690808491,-2.94103864878686));
#34089=CARTESIAN_POINT('Ctrl Pts',(96.0900155412073,1.41691123325679,-2.94404045487048));
#34090=CARTESIAN_POINT('Ctrl Pts',(96.1438449322852,1.42990718554609,-2.94704226095411));
#34091=CARTESIAN_POINT('Ctrl Pts',(96.1982731310567,1.43981919347772,-2.95004406703773));
#34092=CARTESIAN_POINT('Ctrl Pts',(96.2526689799646,1.44972531012299,-2.95304408897233));
#34093=CARTESIAN_POINT('Ctrl Pts',(96.3076624126027,1.45655102104374,-2.95604411090693));
#34094=CARTESIAN_POINT('Ctrl Pts',(96.3628757435706,1.46024158061618,-2.95904413284153));
#34095=CARTESIAN_POINT('Ctrl Pts',(96.4180780646666,1.46393140426874,-2.96204355655362));
#34096=CARTESIAN_POINT('Ctrl Pts',(96.4734996703651,1.46448728292817,-2.96504298026572));
#34097=CARTESIAN_POINT('Ctrl Pts',(96.5287588604504,1.46190641864887,-2.96804240397781));
#34098=CARTESIAN_POINT('Ctrl Pts',(96.5840688533572,1.45932318163867,-2.97104458522557));
#34099=CARTESIAN_POINT('Ctrl Pts',(96.6392156036589,1.453597464962,-2.97404676647333));
#34100=CARTESIAN_POINT('Ctrl Pts',(96.6938200342248,1.44477857181498,-2.97704894772109));
#34101=CARTESIAN_POINT('Ctrl Pts',(96.7484493195153,1.43595566450357,-2.98005249549511));
#34102=CARTESIAN_POINT('Ctrl Pts',(96.8025352763465,1.42403688793077,-2.98305604326913));
#34103=CARTESIAN_POINT('Ctrl Pts',(96.8557098321016,1.40912255691915,-2.98605959104315));
#34104=CARTESIAN_POINT('Ctrl Pts',(96.9089847458818,1.39418007761772,-2.98906880750812));
#34105=CARTESIAN_POINT('Ctrl Pts',(96.961344321584,1.37623092160183,-2.99207802397309));
#34106=CARTESIAN_POINT('Ctrl Pts',(97.0124375568619,1.35542471339227,-2.99508724043806));
#34107=CARTESIAN_POINT('Ctrl Pts',(97.0515259758152,1.33950711140641,-2.99738941436116));
#34108=CARTESIAN_POINT('Ctrl Pts',(97.0898735611337,1.32191834261412,-2.99969158828426));
#34109=CARTESIAN_POINT('Ctrl Pts',(97.1273333106589,1.30274332795046,-3.00199376220736));
#34110=CARTESIAN_POINT('Ctrl Pts',(97.1763125231142,1.27767169429172,-3.0050038908686));
#34111=CARTESIAN_POINT('Ctrl Pts',(97.2239787537575,1.24978133638679,-3.00801401952983));
#34112=CARTESIAN_POINT('Ctrl Pts',(97.2699881597525,1.21923349965211,-3.01102414819107));
#34113=CARTESIAN_POINT('Ctrl Pts',(97.315915794069,1.18873995503075,-3.01402892700551));
#34114=CARTESIAN_POINT('Ctrl Pts',(97.3601920109915,1.15559859433552,-3.01703370581995));
#34115=CARTESIAN_POINT('Ctrl Pts',(97.4024976306186,1.12001643855764,-3.0200384846344));
#34116=CARTESIAN_POINT('Ctrl Pts',(97.4447613958441,1.08446948542787,-3.02304029071802));
#34117=CARTESIAN_POINT('Ctrl Pts',(97.4850580236171,1.04648685900687,-3.02604209680163));
#34118=CARTESIAN_POINT('Ctrl Pts',(97.5230989511658,1.00631765993617,-3.02904390288525));
#34119=CARTESIAN_POINT('Ctrl Pts',(97.5611172687651,0.966172335771173,-3.03204392481985));
#34120=CARTESIAN_POINT('Ctrl Pts',(97.5968821810716,0.923843397553973,-3.03504394675445));
#34121=CARTESIAN_POINT('Ctrl Pts',(97.630141471332,0.879617254178147,-3.03804396868905));
#34122=CARTESIAN_POINT('Ctrl Pts',(97.6633941294888,0.835399929762643,-3.04104339240114));
#34123=CARTESIAN_POINT('Ctrl Pts',(97.6941418406163,0.78928657334929,-3.04404281611323));
#34124=CARTESIAN_POINT('Ctrl Pts',(97.7221737018601,0.741595340355052,-3.04704223982532));
#34125=CARTESIAN_POINT('Ctrl Pts',(97.7502313343402,0.693860262179654,-3.05004442107307));
#34126=CARTESIAN_POINT('Ctrl Pts',(97.7755678604076,0.644544865525786,-3.05304660232083));
#34127=CARTESIAN_POINT('Ctrl Pts',(97.79801744656,0.593993576765358,-3.05604878356859));
#34128=CARTESIAN_POINT('Ctrl Pts',(97.8204772512656,0.543419278180456,-3.05905233134261));
#34129=CARTESIAN_POINT('Ctrl Pts',(97.8400473096086,0.491608460991503,-3.06205587911662));
#34130=CARTESIAN_POINT('Ctrl Pts',(97.8566105245198,0.438924207546307,-3.06505942689064));
#34131=CARTESIAN_POINT('Ctrl Pts',(97.8732049997116,0.386140521439122,-3.0680686433556));
#34132=CARTESIAN_POINT('Ctrl Pts',(97.886781165104,0.332480619252992,-3.07107785982057));
#34133=CARTESIAN_POINT('Ctrl Pts',(97.8972725489559,0.278320229150155,-3.07408707628553));
#34134=CARTESIAN_POINT('Ctrl Pts',(97.9052988875735,0.236885311053383,-3.07638925020866));
#34135=CARTESIAN_POINT('Ctrl Pts',(97.9115207904248,0.195157742081021,-3.07869142413179));
#34136=CARTESIAN_POINT('Ctrl Pts',(97.9159290596762,0.153307040962702,-3.08099359805492));
#34137=CARTESIAN_POINT('Ctrl Pts',(97.9212595324585,0.102701233895996,-3.08377738342231));
#34138=CARTESIAN_POINT('Ctrl Pts',(97.9239512576967,0.0518126899422455,
-3.08656116878969));
#34139=CARTESIAN_POINT('Ctrl Pts',(97.9239807053001,0.000845575841043114,
-3.08934495415707));
#34140=CARTESIAN_POINT('Origin',(96.460480949577,-8.32667268468867E-16,
1.18130019239114E-14));
#34141=CARTESIAN_POINT('',(97.9239808415864,0.000562217564739472,-3.66065504578966));
#34142=CARTESIAN_POINT('',(97.9239808649782,0.000497614912990139,-3.58934495410898));
#34143=CARTESIAN_POINT('',(97.923980949577,-1.01189432752408E-15,1.19922289829666E-14));
#34144=CARTESIAN_POINT('Ctrl Pts',(97.9239808415864,0.000562217564739831,
-3.66065504578966));
#34145=CARTESIAN_POINT('Ctrl Pts',(97.9239576848819,0.0608410786727076,
-3.657393306043));
#34146=CARTESIAN_POINT('Ctrl Pts',(97.9202061513422,0.121005515574799,-3.65413156629635));
#34147=CARTESIAN_POINT('Ctrl Pts',(97.9127935705301,0.180610910579241,-3.65086982654969));
#34148=CARTESIAN_POINT('Ctrl Pts',(97.9053586167204,0.240396209371518,-3.64759824206775));
#34149=CARTESIAN_POINT('Ctrl Pts',(97.8942406267972,0.299618735368977,-3.64432665758581));
#34150=CARTESIAN_POINT('Ctrl Pts',(97.8795576996842,0.357845535538924,-3.64105507310387));
#34151=CARTESIAN_POINT('Ctrl Pts',(97.8648121525538,0.416320662436631,-3.63776953590829));
#34152=CARTESIAN_POINT('Ctrl Pts',(97.8464713619942,0.473791213877508,-3.63448399871271));
#34153=CARTESIAN_POINT('Ctrl Pts',(97.824703128336,0.529839689889331,-3.63119846151713));
#34154=CARTESIAN_POINT('Ctrl Pts',(97.8154624057349,0.553632544522167,-3.62980373476544));
#34155=CARTESIAN_POINT('Ctrl Pts',(97.8056046193567,0.57716942246352,-3.62840900801375));
#34156=CARTESIAN_POINT('Ctrl Pts',(97.7951450939575,0.600419746265101,-3.62701428126206));
#34157=CARTESIAN_POINT('Ctrl Pts',(97.7725711258674,0.650599084958767,-3.62400415260082));
#34158=CARTESIAN_POINT('Ctrl Pts',(97.7471159056111,0.699609016294283,-3.62099402393958));
#34159=CARTESIAN_POINT('Ctrl Pts',(97.7189231632658,0.747098015528166,-3.61798389527834));
#34160=CARTESIAN_POINT('Ctrl Pts',(97.6907805273674,0.794502613429475,-3.61497911646389));
#34161=CARTESIAN_POINT('Ctrl Pts',(97.6599102921119,0.840391193152365,-3.61197433764944));
#34162=CARTESIAN_POINT('Ctrl Pts',(97.6265031467642,0.884434557028855,-3.608969558835));
#34163=CARTESIAN_POINT('Ctrl Pts',(97.593129052252,0.928434347293605,-3.60596775275137));
#34164=CARTESIAN_POINT('Ctrl Pts',(97.5572233371307,0.970592119309586,-3.60296594666775));
#34165=CARTESIAN_POINT('Ctrl Pts',(97.5190202583804,1.01060713520049,-3.59996414058413));
#34166=CARTESIAN_POINT('Ctrl Pts',(97.4808398859554,1.05059836782577,-3.59696411864953));
#34167=CARTESIAN_POINT('Ctrl Pts',(97.4403652202861,1.08844898739605,-3.59396409671493));
#34168=CARTESIAN_POINT('Ctrl Pts',(97.3978696091432,1.12389267766842,-3.59096407478032));
#34169=CARTESIAN_POINT('Ctrl Pts',(97.3553824718821,1.15932930025471,-3.58796465106823));
#34170=CARTESIAN_POINT('Ctrl Pts',(97.3108755948043,1.19235960864079,-3.58496522735613));
#34171=CARTESIAN_POINT('Ctrl Pts',(97.2646561119048,1.22275694980441,-3.58196580364404));
#34172=CARTESIAN_POINT('Ctrl Pts',(97.2183941368853,1.25318223692048,-3.57896362239628));
#34173=CARTESIAN_POINT('Ctrl Pts',(97.1704168526017,1.28096942988906,-3.57596144114851));
#34174=CARTESIAN_POINT('Ctrl Pts',(97.1210598997175,1.30593556526777,-3.57295925990075));
#34175=CARTESIAN_POINT('Ctrl Pts',(97.071680480644,1.33091306467712,-3.56995571212673));
#34176=CARTESIAN_POINT('Ctrl Pts',(97.0209206259756,1.35306673514927,-3.5669521643527));
#34177=CARTESIAN_POINT('Ctrl Pts',(96.9691370623423,1.37226134863099,-3.56394861657868));
#34178=CARTESIAN_POINT('Ctrl Pts',(96.9172557659474,1.39149218871532,-3.56093940011371));
#34179=CARTESIAN_POINT('Ctrl Pts',(96.8643474070127,1.4077526599334,-3.55793018364874));
#34180=CARTESIAN_POINT('Ctrl Pts',(96.8107838906918,1.42095745870392,-3.55492096718377));
#34181=CARTESIAN_POINT('Ctrl Pts',(96.7698056055007,1.4310596709386,-3.55261879326068));
#34182=CARTESIAN_POINT('Ctrl Pts',(96.7284441957512,1.43937446924753,-3.55031661933758));
#34183=CARTESIAN_POINT('Ctrl Pts',(96.6868685021343,1.44588413299514,-3.54801444541448));
#34184=CARTESIAN_POINT('Ctrl Pts',(96.6325076279573,1.45439562086541,-3.54500431675325));
#34185=CARTESIAN_POINT('Ctrl Pts',(96.577551859042,1.45985502291365,-3.54199418809201));
#34186=CARTESIAN_POINT('Ctrl Pts',(96.5223741403715,1.46219064520782,-3.53898405943078));
#34187=CARTESIAN_POINT('Ctrl Pts',(96.4672944880545,1.46452211644307,-3.53597928061634));
#34188=CARTESIAN_POINT('Ctrl Pts',(96.4119941921812,1.46374080342767,-3.53297450180189));
#34189=CARTESIAN_POINT('Ctrl Pts',(96.3568531565239,1.45982654123939,-3.52996972298745));
#34190=CARTESIAN_POINT('Ctrl Pts',(96.3017666737861,1.45591615156505,-3.52696791690384));
#34191=CARTESIAN_POINT('Ctrl Pts',(96.2468396633429,1.44887898995706,-3.52396611082022));
#34192=CARTESIAN_POINT('Ctrl Pts',(96.1924519983541,1.43874693094593,-3.5209643047366));
#34193=CARTESIAN_POINT('Ctrl Pts',(96.1380966591373,1.42862089401041,-3.51796428280201));
#34194=CARTESIAN_POINT('Ctrl Pts',(96.0842805481421,1.41540370216654,-3.51496426086741));
#34195=CARTESIAN_POINT('Ctrl Pts',(96.0313760685382,1.3991787773793,-3.51196423893282));
#34196=CARTESIAN_POINT('Ctrl Pts',(95.9784821384072,1.38295708794013,-3.50896481522073));
#34197=CARTESIAN_POINT('Ctrl Pts',(95.9264999832728,1.3637290114147,-3.50596539150864));
#34198=CARTESIAN_POINT('Ctrl Pts',(95.8757872479501,1.34162793846799,-3.50296596779655));
#34199=CARTESIAN_POINT('Ctrl Pts',(95.8250278896126,1.31950654678581,-3.49996378654879));
#34200=CARTESIAN_POINT('Ctrl Pts',(95.7755407678742,1.29450709314496,-3.49696160530104));
#34201=CARTESIAN_POINT('Ctrl Pts',(95.7276625122829,1.26681071512748,-3.49395942405328));
#34202=CARTESIAN_POINT('Ctrl Pts',(95.6797624635725,1.23910173033355,-3.49095587627927));
#34203=CARTESIAN_POINT('Ctrl Pts',(95.6334731830045,1.20869366453128,-3.48795232850525));
#34204=CARTESIAN_POINT('Ctrl Pts',(95.5891028417432,1.17581139779641,-3.48494878073123));
#34205=CARTESIAN_POINT('Ctrl Pts',(95.54464875893,1.14286707131694,-3.48193956426627));
#34206=CARTESIAN_POINT('Ctrl Pts',(95.5021212570437,1.10743955443111,-3.4789303478013));
#34207=CARTESIAN_POINT('Ctrl Pts',(95.4617949876454,1.06979371817218,-3.47592113133634));
#34208=CARTESIAN_POINT('Ctrl Pts',(95.4309437388545,1.04099311058575,-3.4736189574132));
#34209=CARTESIAN_POINT('Ctrl Pts',(95.4013801595763,1.01089498991828,-3.47131678349007));
#34210=CARTESIAN_POINT('Ctrl Pts',(95.3732113452109,0.979631082306743,-3.46901460956693));
#34211=CARTESIAN_POINT('Ctrl Pts',(95.3363801767998,0.938753030732131,-3.46600448090569));
#34212=CARTESIAN_POINT('Ctrl Pts',(95.3017801642556,0.89570909109196,-3.46299435224445));
#34213=CARTESIAN_POINT('Ctrl Pts',(95.2696751288506,0.850772441563674,-3.45998422358322));
#34214=CARTESIAN_POINT('Ctrl Pts',(95.2376271531398,0.805915657123372,-3.45697944476877));
#34215=CARTESIAN_POINT('Ctrl Pts',(95.20806565924,0.759173264671544,-3.45397466595433));
#34216=CARTESIAN_POINT('Ctrl Pts',(95.1812151137463,0.710852425807484,-3.45096988713989));
#34217=CARTESIAN_POINT('Ctrl Pts',(95.1543911324189,0.662579392407994,-3.44796808105627));
#34218=CARTESIAN_POINT('Ctrl Pts',(95.1302730417724,0.612731465437158,-3.44496627497265));
#34219=CARTESIAN_POINT('Ctrl Pts',(95.1090417072327,0.561644215007995,-3.44196446888903));
#34220=CARTESIAN_POINT('Ctrl Pts',(95.0878229917177,0.510587328721379,-3.43896444695443));
#34221=CARTESIAN_POINT('Ctrl Pts',(95.0694878338139,0.458293065675287,-3.43596442501983));
#34222=CARTESIAN_POINT('Ctrl Pts',(95.0541698450105,0.405118904980973,-3.43296440308523));
#34223=CARTESIAN_POINT('Ctrl Pts',(95.0388549107067,0.351955347535718,-3.42996497937314));
#34224=CARTESIAN_POINT('Ctrl Pts',(95.0265560967773,0.297912748086633,-3.42696555566105));
#34225=CARTESIAN_POINT('Ctrl Pts',(95.0173571006733,0.24336352792737,-3.42396613194896));
#34226=CARTESIAN_POINT('Ctrl Pts',(95.0081496474247,0.188764157661057,-3.4209639507012));
#34227=CARTESIAN_POINT('Ctrl Pts',(95.0020477936072,0.133657758030095,-3.41796176945344));
#34228=CARTESIAN_POINT('Ctrl Pts',(94.9990837646842,0.0784252382043858,
-3.41495958820568));
#34229=CARTESIAN_POINT('Ctrl Pts',(94.9961183866011,0.0231675777617289,
-3.41195604043166));
#34230=CARTESIAN_POINT('Ctrl Pts',(94.9962936788924,-0.0322157882785609,
-3.40895249265764));
#34231=CARTESIAN_POINT('Ctrl Pts',(94.9995896819569,-0.0873438846820572,
-3.40594894488362));
#34232=CARTESIAN_POINT('Ctrl Pts',(95.0028919056725,-0.142576026089837,
-3.40293972841866));
#34233=CARTESIAN_POINT('Ctrl Pts',(95.0093265444389,-0.19755140961134,-3.39993051195369));
#34234=CARTESIAN_POINT('Ctrl Pts',(95.018821830172,-0.251895282679696,-3.39692129548872));
#34235=CARTESIAN_POINT('Ctrl Pts',(95.0260861129053,-0.2934705727646,-3.39461912156561));
#34236=CARTESIAN_POINT('Ctrl Pts',(95.0351406753307,-0.334676361031573,
-3.39231694764249));
#34237=CARTESIAN_POINT('Ctrl Pts',(95.0459337097695,-0.375350977556801,
-3.39001477371937));
#34238=CARTESIAN_POINT('Ctrl Pts',(95.0600457722768,-0.428533679244961,
-3.38700464505813));
#34239=CARTESIAN_POINT('Ctrl Pts',(95.0771909191365,-0.481031160584242,
-3.38399451639689));
#34240=CARTESIAN_POINT('Ctrl Pts',(95.0972845071804,-0.532473200675086,
-3.38098438773565));
#34241=CARTESIAN_POINT('Ctrl Pts',(95.1173423832566,-0.583823813765898,
-3.37797960892121));
#34242=CARTESIAN_POINT('Ctrl Pts',(95.1403381106903,-0.634122220236709,
-3.37497483010676));
#34243=CARTESIAN_POINT('Ctrl Pts',(95.1661370810418,-0.683012591381184,
-3.37197005129231));
#34244=CARTESIAN_POINT('Ctrl Pts',(95.1919105275863,-0.731854593603253,
-3.36896824520869));
#34245=CARTESIAN_POINT('Ctrl Pts',(95.2204814779276,-0.779290855221575,
-3.36596643912507));
#34246=CARTESIAN_POINT('Ctrl Pts',(95.2516677072236,-0.824986542381811,
-3.36296463304145));
#34247=CARTESIAN_POINT('Ctrl Pts',(95.2828354007185,-0.870655069921066,
-3.35996461110685));
#34248=CARTESIAN_POINT('Ctrl Pts',(95.31661499511,-0.914584638159802,-3.35696458917225));
#34249=CARTESIAN_POINT('Ctrl Pts',(95.3527800968148,-0.956468018696854,
-3.35396456723765));
#34250=CARTESIAN_POINT('Ctrl Pts',(95.3889379869797,-0.998343047434655,
-3.35096514352556));
#34251=CARTESIAN_POINT('Ctrl Pts',(95.4274800948128,-1.03817229928642,-3.34796571981346));
#34252=CARTESIAN_POINT('Ctrl Pts',(95.4681402394164,-1.07568218585139,-3.34496629610137));
#34253=CARTESIAN_POINT('Ctrl Pts',(95.5088377651339,-1.11322655732413,-3.34196411485361));
#34254=CARTESIAN_POINT('Ctrl Pts',(95.5516568289275,-1.14844694454707,-3.33896193360585));
#34255=CARTESIAN_POINT('Ctrl Pts',(95.5962960169831,-1.18110823055201,-3.33595975235809));
#34256=CARTESIAN_POINT('Ctrl Pts',(95.6409555238062,-1.21378438324931,-3.33295620458407));
#34257=CARTESIAN_POINT('Ctrl Pts',(95.6874363624139,-1.24389882502842,-3.32995265681005));
#34258=CARTESIAN_POINT('Ctrl Pts',(95.7354085499465,-1.27126010922002,-3.32694910903603));
#34259=CARTESIAN_POINT('Ctrl Pts',(95.7834712769097,-1.2986730332308,-3.32393989257106));
#34260=CARTESIAN_POINT('Ctrl Pts',(95.8330305015201,-1.32332218383296,-3.32093067610609));
#34261=CARTESIAN_POINT('Ctrl Pts',(95.8837331446179,-1.34506290539695,-3.31792145964112));
#34262=CARTESIAN_POINT('Ctrl Pts',(95.9225227445457,-1.36169544839836,-3.31561928571802));
#34263=CARTESIAN_POINT('Ctrl Pts',(95.9619810785525,-1.37662668963317,-3.31331711179491));
#34264=CARTESIAN_POINT('Ctrl Pts',(96.0019444362136,-1.38981168361493,-3.3110149378718));
#34265=CARTESIAN_POINT('Ctrl Pts',(96.0541971557357,-1.40705127089561,-3.30800480921057));
#34266=CARTESIAN_POINT('Ctrl Pts',(96.1075332501576,-1.42137616669331,-3.30499468054933));
#34267=CARTESIAN_POINT('Ctrl Pts',(96.1615964008176,-1.43265497469311,-3.30198455188809));
#34268=CARTESIAN_POINT('Ctrl Pts',(96.2155634660256,-1.44391373707307,-3.29897977307365));
#34269=CARTESIAN_POINT('Ctrl Pts',(96.2702545103201,-1.45213704830828,-3.29597499425921));
#34270=CARTESIAN_POINT('Ctrl Pts',(96.3252979680604,-1.45724322318146,-3.29297021544476));
#34271=CARTESIAN_POINT('Ctrl Pts',(96.3802869694184,-1.46234434634055,-3.28996840936115));
#34272=CARTESIAN_POINT('Ctrl Pts',(96.4356271702808,-1.46433439363331,-3.28696660327753));
#34273=CARTESIAN_POINT('Ctrl Pts',(96.4909385713449,-1.46318303136561,-3.28396479719391));
#34274=CARTESIAN_POINT('Ctrl Pts',(96.5462170976066,-1.46203235341987,-3.28096477525931));
#34275=CARTESIAN_POINT('Ctrl Pts',(96.6014663310501,-1.45774397764402,-3.27796475332471));
#34276=CARTESIAN_POINT('Ctrl Pts',(96.6563052590559,-1.45033964636464,-3.27496473139011));
#34277=CARTESIAN_POINT('Ctrl Pts',(96.711133251848,-1.44293679155368,-3.27196530767802));
#34278=CARTESIAN_POINT('Ctrl Pts',(96.7655505786146,-1.43241928581969,-3.26896588396593));
#34279=CARTESIAN_POINT('Ctrl Pts',(96.8191826615094,-1.41886057519997,-3.26596646025384));
#34280=CARTESIAN_POINT('Ctrl Pts',(96.8728640513364,-1.40528939930967,-3.26296427900608));
#34281=CARTESIAN_POINT('Ctrl Pts',(96.9257582418854,-1.38867156231267,-3.25996209775832));
#34282=CARTESIAN_POINT('Ctrl Pts',(96.977503625043,-1.36913103940199,-3.25695991651056));
#34283=CARTESIAN_POINT('Ctrl Pts',(97.0292725615504,-1.34958162207904,-3.25395636873654));
#34284=CARTESIAN_POINT('Ctrl Pts',(97.0798911647579,-1.32710708157964,-3.25095282096253));
#34285=CARTESIAN_POINT('Ctrl Pts',(97.1290187915884,-1.30187918172107,-3.24794927318851));
#34286=CARTESIAN_POINT('Ctrl Pts',(97.1782391385467,-1.2766036684472,-3.24494005672354));
#34287=CARTESIAN_POINT('Ctrl Pts',(97.2259624313338,-1.24856468317768,-3.24193084025858));
#34288=CARTESIAN_POINT('Ctrl Pts',(97.2718745959,-1.21797889994313,-3.23892162379361));
#34289=CARTESIAN_POINT('Ctrl Pts',(97.3069992834222,-1.19457952226435,-3.23661944987049));
#34290=CARTESIAN_POINT('Ctrl Pts',(97.3410644786033,-1.16969047719024,-3.23431727594736));
#34291=CARTESIAN_POINT('Ctrl Pts',(97.3739430876555,-1.1434243185699,-3.23201510202424));
#34292=CARTESIAN_POINT('Ctrl Pts',(97.4164069259365,-1.10950068420493,-3.22904176635146));
#34293=CARTESIAN_POINT('Ctrl Pts',(97.4570782501623,-1.07312835567167,-3.22606843067869));
#34294=CARTESIAN_POINT('Ctrl Pts',(97.4956562800578,-1.03452611623096,-3.22309509500591));
#34295=CARTESIAN_POINT('Ctrl Pts',(97.5341692430004,-0.995988984575801,
-3.22012677425725));
#34296=CARTESIAN_POINT('Ctrl Pts',(97.5705955300688,-0.955229777234613,
-3.21715845350858));
#34297=CARTESIAN_POINT('Ctrl Pts',(97.604667165064,-0.912507618757003,-3.21419013275992));
#34298=CARTESIAN_POINT('Ctrl Pts',(97.6387056440851,-0.869827034297733,
-3.21122470055962));
#34299=CARTESIAN_POINT('Ctrl Pts',(97.6703936701961,-0.825187701695912,
-3.20825926835933));
#34300=CARTESIAN_POINT('Ctrl Pts',(97.699501443502,-0.778884115664169,-3.20529383615903));
#34301=CARTESIAN_POINT('Ctrl Pts',(97.7285930751017,-0.732606207270699,
-3.20233004843818));
#34302=CARTESIAN_POINT('Ctrl Pts',(97.755107000612,-0.684666332170437,-3.19936626071733));
#34303=CARTESIAN_POINT('Ctrl Pts',(97.7788564003111,-0.635388401610821,
-3.19640247299648));
#34304=CARTESIAN_POINT('Ctrl Pts',(97.8027273163715,-0.58585833521259,-3.19342352073657));
#34305=CARTESIAN_POINT('Ctrl Pts',(97.8238050598094,-0.534976961069053,
-3.19044456847667));
#34306=CARTESIAN_POINT('Ctrl Pts',(97.8419475559497,-0.483096538465318,
-3.18746561621676));
#34307=CARTESIAN_POINT('Ctrl Pts',(97.8600104555927,-0.431443730622092,
-3.18449973350162));
#34308=CARTESIAN_POINT('Ctrl Pts',(97.8751636881653,-0.378801157440791,
-3.18153385078646));
#34309=CARTESIAN_POINT('Ctrl Pts',(97.8873170410266,-0.325531900336655,
-3.17856796807132));
#34310=CARTESIAN_POINT('Ctrl Pts',(97.8995507268635,-0.271910536453492,
-3.17558248103903));
#34311=CARTESIAN_POINT('Ctrl Pts',(97.9087446207047,-0.217654719128803,
-3.17259699400675));
#34312=CARTESIAN_POINT('Ctrl Pts',(97.9148594487037,-0.163142365061595,
-3.16961150697446));
#34313=CARTESIAN_POINT('Ctrl Pts',(97.9209742767027,-0.108630010994388,
-3.16662601994218));
#34314=CARTESIAN_POINT('Ctrl Pts',(97.9240100677082,-0.0538616766468094,
-3.16364053290989));
#34315=CARTESIAN_POINT('Ctrl Pts',(97.9239807388017,0.000785454740996269,
-3.16065504587761));
#34316=CARTESIAN_POINT('Ctrl Pts',(97.9239807053004,0.000845575209102073,
-3.08934495419159));
#34317=CARTESIAN_POINT('Ctrl Pts',(97.9240121116984,-0.0535118081674962,
-3.0923139135121));
#34318=CARTESIAN_POINT('Ctrl Pts',(97.9210108565796,-0.107988214502587,
-3.09528287283261));
#34319=CARTESIAN_POINT('Ctrl Pts',(97.9149634846939,-0.162212222227354,
-3.09825183215312));
#34320=CARTESIAN_POINT('Ctrl Pts',(97.9089235593934,-0.216369459840959,
-3.10121713557006));
#34321=CARTESIAN_POINT('Ctrl Pts',(97.8998449981556,-0.270274378405412,
-3.10418243898699));
#34322=CARTESIAN_POINT('Ctrl Pts',(97.887766341459,-0.323556270407781,-3.10714774240393));
#34323=CARTESIAN_POINT('Ctrl Pts',(97.8756974888544,-0.376794914176668,
-3.11011063892183));
#34324=CARTESIAN_POINT('Ctrl Pts',(97.8606334808327,-0.429411004759582,
-3.11307353543973));
#34325=CARTESIAN_POINT('Ctrl Pts',(97.8426642475837,-0.481042181841941,
-3.11603643195763));
#34326=CARTESIAN_POINT('Ctrl Pts',(97.8247020604722,-0.532653113187079,
-3.11899816665765));
#34327=CARTESIAN_POINT('Ctrl Pts',(97.8038370841483,-0.583279384134176,
-3.12195990135768));
#34328=CARTESIAN_POINT('Ctrl Pts',(97.780208886654,-0.63257443996624,-3.1249216360577));
#34329=CARTESIAN_POINT('Ctrl Pts',(97.7565628657859,-0.681906680361391,
-3.12788560487247));
#34330=CARTESIAN_POINT('Ctrl Pts',(97.7301496885838,-0.729905205756458,
-3.13084957368724));
#34331=CARTESIAN_POINT('Ctrl Pts',(97.7011561263692,-0.776245679982617,
-3.133813542502));
#34332=CARTESIAN_POINT('Ctrl Pts',(97.6721530801836,-0.822601312460516,
-3.13677848084904));
#34333=CARTESIAN_POINT('Ctrl Pts',(97.6405682784201,-0.867297366750257,
-3.13974341919608));
#34334=CARTESIAN_POINT('Ctrl Pts',(97.6066314129966,-0.910039210805195,
-3.14270835754312));
#34335=CARTESIAN_POINT('Ctrl Pts',(97.5726295608355,-0.952862902519668,
-3.14567897354095));
#34336=CARTESIAN_POINT('Ctrl Pts',(97.5362670075506,-0.99372449954857,-3.14864958953877));
#34337=CARTESIAN_POINT('Ctrl Pts',(97.497812431789,-1.03236410534844,-3.1516202055366));
#34338=CARTESIAN_POINT('Ctrl Pts',(97.4616819967994,-1.06866838741961,-3.15441128165856));
#34339=CARTESIAN_POINT('Ctrl Pts',(97.4237054074271,-1.10301125847572,-3.15720235778053));
#34340=CARTESIAN_POINT('Ctrl Pts',(97.3841308561572,-1.13521059723489,-3.15999343390249));
#34341=CARTESIAN_POINT('Ctrl Pts',(97.3414503681205,-1.16993704260454,-3.16300356256373));
#34342=CARTESIAN_POINT('Ctrl Pts',(97.2967190667783,-1.20232611928244,-3.16601369122497));
#34343=CARTESIAN_POINT('Ctrl Pts',(97.2502230660361,-1.23212809378356,-3.16902381988621));
#34344=CARTESIAN_POINT('Ctrl Pts',(97.2038097017883,-1.2618771017787,-3.17202859870065));
#34345=CARTESIAN_POINT('Ctrl Pts',(97.1556383033114,-1.28904784969789,-3.1750333775151));
#34346=CARTESIAN_POINT('Ctrl Pts',(97.1060269435155,-1.31343161973127,-3.17803815632954));
#34347=CARTESIAN_POINT('Ctrl Pts',(97.0564646659408,-1.33779126606395,-3.18103996241316));
#34348=CARTESIAN_POINT('Ctrl Pts',(97.00546572075,-1.35936916469082,-3.18404176849678));
#34349=CARTESIAN_POINT('Ctrl Pts',(96.9533743582289,-1.37800157391331,-3.1870435745804));
#34350=CARTESIAN_POINT('Ctrl Pts',(96.9013139566528,-1.39662290880462,-3.190043596515));
#34351=CARTESIAN_POINT('Ctrl Pts',(96.8481629209475,-1.41230204673818,-3.1930436184496));
#34352=CARTESIAN_POINT('Ctrl Pts',(96.7942850036013,-1.42492354304256,-3.1960436403842));
#34353=CARTESIAN_POINT('Ctrl Pts',(96.7404178298375,-1.43754252254429,-3.19904306409629));
#34354=CARTESIAN_POINT('Ctrl Pts',(96.6858245761938,-1.44710495089075,-3.20204248780838));
#34355=CARTESIAN_POINT('Ctrl Pts',(96.6308814054568,-1.4535459864194,-3.20504191152047));
#34356=CARTESIAN_POINT('Ctrl Pts',(96.5758877224324,-1.4599929435473,-3.20804409276823));
#34357=CARTESIAN_POINT('Ctrl Pts',(96.520544005255,-1.4633127130099,-3.21104627401599));
#34358=CARTESIAN_POINT('Ctrl Pts',(96.4652323024529,-1.46349228718359,-3.21404845526375));
#34359=CARTESIAN_POINT('Ctrl Pts',(96.4098954229915,-1.46367194309546,-3.21705200303776));
#34360=CARTESIAN_POINT('Ctrl Pts',(96.3545911152333,-1.46070858272002,-3.22005555081178));
#34361=CARTESIAN_POINT('Ctrl Pts',(96.2996988664161,-1.45464132064727,-3.2230590985858));
#34362=CARTESIAN_POINT('Ctrl Pts',(96.2447030177171,-1.44856260763843,-3.22606831505077));
#34363=CARTESIAN_POINT('Ctrl Pts',(96.1901213035764,-1.43936837842356,-3.22907753151573));
#34364=CARTESIAN_POINT('Ctrl Pts',(96.1363243881436,-1.42714917709386,-3.2320867479807));
#34365=CARTESIAN_POINT('Ctrl Pts',(96.095167543066,-1.41780098729428,-3.23438892190381));
#34366=CARTESIAN_POINT('Ctrl Pts',(96.0544698633411,-1.40668339077257,-3.23669109582693));
#34367=CARTESIAN_POINT('Ctrl Pts',(96.0143902056032,-1.39385626882433,-3.23899326975004));
#34368=CARTESIAN_POINT('Ctrl Pts',(95.9619854218993,-1.37708460486363,-3.24200339841128));
#34369=CARTESIAN_POINT('Ctrl Pts',(95.9104176910409,-1.35731820048868,-3.24501352707252));
#34370=CARTESIAN_POINT('Ctrl Pts',(95.8600525030574,-1.33466023039948,-3.24802365573375));
#34371=CARTESIAN_POINT('Ctrl Pts',(95.8097768282042,-1.31204252990746,-3.25102843454819));
#34372=CARTESIAN_POINT('Ctrl Pts',(95.7606999325518,-1.28654367725042,-3.25403321336264));
#34373=CARTESIAN_POINT('Ctrl Pts',(95.7131704166725,-1.2583160244589,-3.25703799217708));
#34374=CARTESIAN_POINT('Ctrl Pts',(95.6656879233748,-1.23011629825322,-3.2600397982607));
#34375=CARTESIAN_POINT('Ctrl Pts',(95.6197502291,-1.19919338822771,-3.26304160434432));
#34376=CARTESIAN_POINT('Ctrl Pts',(95.5756825689323,-1.16574614544013,-3.26604341042795));
#34377=CARTESIAN_POINT('Ctrl Pts',(95.5316411007539,-1.13231878230631,-3.26904343236254));
#34378=CARTESIAN_POINT('Ctrl Pts',(95.4894678835039,-1.09637037886921,-3.27204345429714));
#34379=CARTESIAN_POINT('Ctrl Pts',(95.4494583581334,-1.05814250911235,-3.27504347623174));
#34380=CARTESIAN_POINT('Ctrl Pts',(95.409456810904,-1.0199222622238,-3.27804289994383));
#34381=CARTESIAN_POINT('Ctrl Pts',(95.3716184803319,-0.979423816342476,
-3.28104232365592));
#34382=CARTESIAN_POINT('Ctrl Pts',(95.3362032069245,-0.936926788696039,
-3.28404174736801));
#34383=CARTESIAN_POINT('Ctrl Pts',(95.3007553743028,-0.894390691187924,
-3.28704392861577));
#34384=CARTESIAN_POINT('Ctrl Pts',(95.2677353882254,-0.849852747592058,
-3.29004610986353));
#34385=CARTESIAN_POINT('Ctrl Pts',(95.2373628927433,-0.803625826518439,
-3.29304829111129));
#34386=CARTESIAN_POINT('Ctrl Pts',(95.2069765723756,-0.757377863976506,
-3.29605183888531));
#34387=CARTESIAN_POINT('Ctrl Pts',(95.1792404097869,-0.70943984935139,-3.29905538665933));
#34388=CARTESIAN_POINT('Ctrl Pts',(95.1543289957927,-0.660150985476428,
-3.30205893443335));
#34389=CARTESIAN_POINT('Ctrl Pts',(95.129370565697,-0.610769097165899,-3.30506815089832));
#34390=CARTESIAN_POINT('Ctrl Pts',(95.1072477457684,-0.560031751868807,
-3.30807736736329));
#34391=CARTESIAN_POINT('Ctrl Pts',(95.0880872323301,-0.508298863722103,
-3.31108658382825));
#34392=CARTESIAN_POINT('Ctrl Pts',(95.0734286542899,-0.468721084108807,
-3.31338875775137));
#34393=CARTESIAN_POINT('Ctrl Pts',(95.0605028881457,-0.428561070948869,
-3.3156909316745));
#34394=CARTESIAN_POINT('Ctrl Pts',(95.0493465803421,-0.387984589853703,
-3.31799310559762));
#34395=CARTESIAN_POINT('Ctrl Pts',(95.0347595321891,-0.334930201785944,
-3.32100323425886));
#34396=CARTESIAN_POINT('Ctrl Pts',(95.023138022119,-0.280940553597613,-3.32401336292009));
#34397=CARTESIAN_POINT('Ctrl Pts',(95.0145953408613,-0.226378127275874,
-3.32702349158133));
#34398=CARTESIAN_POINT('Ctrl Pts',(95.0060678423553,-0.171912673759762,
-3.33002827039578));
#34399=CARTESIAN_POINT('Ctrl Pts',(95.0006083945771,-0.116876979854245,
-3.33303304921022));
#34400=CARTESIAN_POINT('Ctrl Pts',(94.9982798725851,-0.0616462524720104,
-3.33603782802466));
#34401=CARTESIAN_POINT('Ctrl Pts',(94.9959536542799,-0.00647016674420076,
-3.33903963410828));
#34402=CARTESIAN_POINT('Ctrl Pts',(94.9967522478346,0.0489000451757762,
-3.34204144019191));
#34403=CARTESIAN_POINT('Ctrl Pts',(95.0006868173097,0.104083338714638,-3.34504324627553));
#34404=CARTESIAN_POINT('Ctrl Pts',(95.0046190482399,0.15923383359278,-3.34804326821013));
#34405=CARTESIAN_POINT('Ctrl Pts',(95.011683523246,0.214197104563301,-3.35104329014472));
#34406=CARTESIAN_POINT('Ctrl Pts',(95.0218393453912,0.268593716802291,-3.35404331207932));
#34407=CARTESIAN_POINT('Ctrl Pts',(95.031993142404,0.3229794820279,-3.35704273579141));
#34408=CARTESIAN_POINT('Ctrl Pts',(95.0452369654758,0.376798294070868,-3.36004215950349));
#34409=CARTESIAN_POINT('Ctrl Pts',(95.0614786034864,0.429679747757636,-3.36304158321558));
#34410=CARTESIAN_POINT('Ctrl Pts',(95.0777351733308,0.482609818281835,-3.36604376446333));
#34411=CARTESIAN_POINT('Ctrl Pts',(95.0969949089703,0.534600302828475,-3.36904594571109));
#34412=CARTESIAN_POINT('Ctrl Pts',(95.119115787171,0.585296293413356,-3.37204812695885));
#34413=CARTESIAN_POINT('Ctrl Pts',(95.1412467343044,0.636015359687777,-3.37505167473287));
#34414=CARTESIAN_POINT('Ctrl Pts',(95.1662411813487,0.6854382853224,-3.37805522250689));
#34415=CARTESIAN_POINT('Ctrl Pts',(95.1939104325383,0.733233506714116,-3.38105877028091));
#34416=CARTESIAN_POINT('Ctrl Pts',(95.2216319047829,0.781118933542593,-3.38406798674587));
#34417=CARTESIAN_POINT('Ctrl Pts',(95.2520379749969,0.827370076917965,-3.38707720321084));
#34418=CARTESIAN_POINT('Ctrl Pts',(95.2848964317778,0.871684169588323,-3.3900864196758));
#34419=CARTESIAN_POINT('Ctrl Pts',(95.3100344978611,0.905586266616025,-3.39238859359893));
#34420=CARTESIAN_POINT('Ctrl Pts',(95.3366070018268,0.938355217170115,-3.39469076752205));
#34421=CARTESIAN_POINT('Ctrl Pts',(95.3644951339879,0.969869755187488,-3.39699294144517));
#34422=CARTESIAN_POINT('Ctrl Pts',(95.4009593059964,1.01107550996512,-3.40000307010641));
#34423=CARTESIAN_POINT('Ctrl Pts',(95.4398271418934,1.05030856924532,-3.40301319876765));
#34424=CARTESIAN_POINT('Ctrl Pts',(95.4808569548691,1.08727599025845,-3.40602332742889));
#34425=CARTESIAN_POINT('Ctrl Pts',(95.5218138463062,1.12417770974817,-3.40902810624333));
#34426=CARTESIAN_POINT('Ctrl Pts',(95.5649247002899,1.15882143129332,-3.41203288505777));
#34427=CARTESIAN_POINT('Ctrl Pts',(95.6099096256182,1.1909494837561,-3.41503766387222));
#34428=CARTESIAN_POINT('Ctrl Pts',(95.6548500458156,1.2230457508337,-3.41803946995583));
#34429=CARTESIAN_POINT('Ctrl Pts',(95.7016604368568,1.25263097367015,-3.42104127603945));
#34430=CARTESIAN_POINT('Ctrl Pts',(95.7500277636557,1.2794876008052,-3.42404308212307));
#34431=CARTESIAN_POINT('Ctrl Pts',(95.7983663429219,1.30632826547513,-3.42704310405767));
#34432=CARTESIAN_POINT('Ctrl Pts',(95.8482595629937,1.33044329302549,-3.43004312599227));
#34433=CARTESIAN_POINT('Ctrl Pts',(95.8993672910688,1.35165961404323,-3.43304314792687));
#34434=CARTESIAN_POINT('Ctrl Pts',(95.9504648279539,1.3728717043983,-3.43604257163895));
#34435=CARTESIAN_POINT('Ctrl Pts',(96.0027759043986,1.39118603377389,-3.43904199535104));
#34436=CARTESIAN_POINT('Ctrl Pts',(96.0559399123072,1.40647744353213,-3.44204141906313));
#34437=CARTESIAN_POINT('Ctrl Pts',(96.1091527968208,1.42178291152683,-3.44504360031089));
#34438=CARTESIAN_POINT('Ctrl Pts',(96.1632196707923,1.43405976125441,-3.44804578155864));
#34439=CARTESIAN_POINT('Ctrl Pts',(96.217765688296,1.4432330206662,-3.4510479628064));
#34440=CARTESIAN_POINT('Ctrl Pts',(96.272336533936,1.45241045554205,-3.45405151058041));
#34441=CARTESIAN_POINT('Ctrl Pts',(96.3273864320175,1.45848142601984,-3.45705505835442));
#34442=CARTESIAN_POINT('Ctrl Pts',(96.382534586474,1.46142280483062,-3.46005860612844));
#34443=CARTESIAN_POINT('Ctrl Pts',(96.437786823791,1.46436973499891,-3.4630678225934));
#34444=CARTESIAN_POINT('Ctrl Pts',(96.4931371585245,1.4641752760542,-3.46607703905837));
#34445=CARTESIAN_POINT('Ctrl Pts',(96.5482051355539,1.46086848045767,-3.46908625552334));
#34446=CARTESIAN_POINT('Ctrl Pts',(96.5903343948453,1.45833864630313,-3.47138842944647));
#34447=CARTESIAN_POINT('Ctrl Pts',(96.6322983846968,1.45398828503215,-3.47369060336961));
#34448=CARTESIAN_POINT('Ctrl Pts',(96.6739306243701,1.44785064365449,-3.47599277729274));
#34449=CARTESIAN_POINT('Ctrl Pts',(96.7283654334054,1.43982558089201,-3.47900290595397));
#34450=CARTESIAN_POINT('Ctrl Pts',(96.7824614093834,1.42870951185747,-3.48201303461521));
#34451=CARTESIAN_POINT('Ctrl Pts',(96.8358411481265,1.41454479297931,-3.48502316327644));
#34452=CARTESIAN_POINT('Ctrl Pts',(96.8891260160331,1.40040524879775,-3.48802794209089));
#34453=CARTESIAN_POINT('Ctrl Pts',(96.9416966665717,1.38322794180103,-3.49103272090533));
#34454=CARTESIAN_POINT('Ctrl Pts',(96.9931843617755,1.36310649790546,-3.49403749971977));
#34455=CARTESIAN_POINT('Ctrl Pts',(97.044621118435,1.34300496084503,-3.49703930580339));
#34456=CARTESIAN_POINT('Ctrl Pts',(97.0949765526913,1.31996524816049,-3.50004111188701));
#34457=CARTESIAN_POINT('Ctrl Pts',(97.1438974181991,1.29413066589739,-3.50304291797063));
#34458=CARTESIAN_POINT('Ctrl Pts',(97.1927892071738,1.26831143863836,-3.50604293990523));
#34459=CARTESIAN_POINT('Ctrl Pts',(97.2402476513393,1.23970088044227,-3.50904296183983));
#34460=CARTESIAN_POINT('Ctrl Pts',(97.2859419531762,1.20848929723727,-3.51204298377443));
#34461=CARTESIAN_POINT('Ctrl Pts',(97.3316271432932,1.17728393781056,-3.51504240748653));
#34462=CARTESIAN_POINT('Ctrl Pts',(97.3755484538541,1.14347888111908,-3.51804183119863));
#34463=CARTESIAN_POINT('Ctrl Pts',(97.4174040262834,1.10730775995957,-3.52104125491073));
#34464=CARTESIAN_POINT('Ctrl Pts',(97.4592980788492,1.07110338469324,-3.52404343615849));
#34465=CARTESIAN_POINT('Ctrl Pts',(97.4991221985946,1.03252894514053,-3.52704561740625));
#34466=CARTESIAN_POINT('Ctrl Pts',(97.5366087800687,0.991857420419461,-3.53004779865401));
#34467=CARTESIAN_POINT('Ctrl Pts',(97.5741124246027,0.951167382923171,-3.53305134642803));
#34468=CARTESIAN_POINT('Ctrl Pts',(97.6092760739727,0.908378766162039,-3.53605489420205));
#34469=CARTESIAN_POINT('Ctrl Pts',(97.6418722929925,0.863797860441228,-3.53905844197608));
#34470=CARTESIAN_POINT('Ctrl Pts',(97.6745300318901,0.81913281576358,-3.54206765844104));
#34471=CARTESIAN_POINT('Ctrl Pts',(97.7046103729047,0.772669169180129,-3.54507687490601));
#34472=CARTESIAN_POINT('Ctrl Pts',(97.7319297690702,0.72474143624424,-3.54808609137097));
#34473=CARTESIAN_POINT('Ctrl Pts',(97.7528302267739,0.688074756314997,-3.55038826529408));
#34474=CARTESIAN_POINT('Ctrl Pts',(97.7721156414486,0.650551765119928,-3.55269043921719));
#34475=CARTESIAN_POINT('Ctrl Pts',(97.7897228939381,0.612330060793356,-3.5549926131403));
#34476=CARTESIAN_POINT('Ctrl Pts',(97.8147040021358,0.558101240490146,-3.55825892944363));
#34477=CARTESIAN_POINT('Ctrl Pts',(97.8363970660602,0.502267217142413,-3.56152524574696));
#34478=CARTESIAN_POINT('Ctrl Pts',(97.8546129689978,0.445228213869789,-3.56479156205029));
#34479=CARTESIAN_POINT('Ctrl Pts',(97.8727780892455,0.388348225169438,-3.56804877244609));
#34480=CARTESIAN_POINT('Ctrl Pts',(97.8874852156449,0.330270297420546,-3.57130598284188));
#34481=CARTESIAN_POINT('Ctrl Pts',(97.898593061022,0.271414452296158,-3.57456319323767));
#34482=CARTESIAN_POINT('Ctrl Pts',(97.9096536738433,0.212808872808053,-3.57780655338919));
#34483=CARTESIAN_POINT('Ctrl Pts',(97.9171454033261,0.153432332319883,-3.5810499135407));
#34484=CARTESIAN_POINT('Ctrl Pts',(97.9209772034918,0.0937173532535882,
-3.58429327369221));
#34485=CARTESIAN_POINT('Ctrl Pts',(97.9229666042936,0.0627144245782946,
-3.58597716716447));
#34486=CARTESIAN_POINT('Ctrl Pts',(97.9239702826564,0.0316205307435951,
-3.58766106063673));
#34487=CARTESIAN_POINT('Ctrl Pts',(97.9239808649782,0.000497614912986743,
-3.58934495410898));
#34488=CARTESIAN_POINT('Origin',(96.460480949577,-8.32667268468867E-16,
1.18130019239114E-14));
#34489=CARTESIAN_POINT('',(97.9239803682192,-0.00130446693377829,-4.16065504588301));
#34490=CARTESIAN_POINT('',(97.9239803685999,-0.00130403978581263,-4.08934495418713));
#34491=CARTESIAN_POINT('',(97.923980949577,-1.01189432752408E-15,1.19922289829666E-14));
#34492=CARTESIAN_POINT('Ctrl Pts',(97.9239803682198,-0.00130446619604857,
-4.1606550458429));
#34493=CARTESIAN_POINT('Ctrl Pts',(97.9240290145792,0.0532725852280853,
-4.15768779896672));
#34494=CARTESIAN_POINT('Ctrl Pts',(97.921020447974,0.107929002943695,-4.15472055209055));
#34495=CARTESIAN_POINT('Ctrl Pts',(97.914954670438,0.162291236130919,-4.15175330521438));
#34496=CARTESIAN_POINT('Ctrl Pts',(97.9088930972105,0.216615789794604,-4.14878811499485));
#34497=CARTESIAN_POINT('Ctrl Pts',(97.8997785687796,0.270646025560744,-4.14582292477533));
#34498=CARTESIAN_POINT('Ctrl Pts',(97.8876630704609,0.324011487187377,-4.14285773455581));
#34499=CARTESIAN_POINT('Ctrl Pts',(97.8755509065509,0.377362261654151,-4.13989336041135));
#34500=CARTESIAN_POINT('Ctrl Pts',(97.8604395308884,0.430048096798754,-4.1369289862669));
#34501=CARTESIAN_POINT('Ctrl Pts',(97.8424319199135,0.481709212685351,-4.13396461212244));
#34502=CARTESIAN_POINT('Ctrl Pts',(97.824409016481,0.533414200323036,-4.13099772056654));
#34503=CARTESIAN_POINT('Ctrl Pts',(97.8034851423599,0.584092217259106,-4.12803082901064));
#34504=CARTESIAN_POINT('Ctrl Pts',(97.7798124814009,0.633400788707461,-4.12506393745474));
#34505=CARTESIAN_POINT('Ctrl Pts',(97.7561296712694,0.682730500203988,-4.12209577390436));
#34506=CARTESIAN_POINT('Ctrl Pts',(97.729695989229,0.73068912166178,-4.11912761035398));
#34507=CARTESIAN_POINT('Ctrl Pts',(97.7007093301368,0.776959338739193,-4.11615944680361));
#34508=CARTESIAN_POINT('Ctrl Pts',(97.6716690716219,0.823315114380496,-4.11318579480241));
#34509=CARTESIAN_POINT('Ctrl Pts',(97.6400667247767,0.867975809663054,-4.11021214280122));
#34510=CARTESIAN_POINT('Ctrl Pts',(97.6061423735087,0.910654792835792,-4.10723849080002));
#34511=CARTESIAN_POINT('Ctrl Pts',(97.582469385632,0.940436911387082,-4.10516342598249));
#34512=CARTESIAN_POINT('Ctrl Pts',(97.5576665713033,0.969254718261061,-4.10308836116496));
#34513=CARTESIAN_POINT('Ctrl Pts',(97.5318258778327,0.997021712251408,-4.10101329634742));
#34514=CARTESIAN_POINT('Ctrl Pts',(97.4943408742874,1.03730104412602,-4.09800316768619));
#34515=CARTESIAN_POINT('Ctrl Pts',(97.4545023806711,1.07554808367405,-4.09499303902495));
#34516=CARTESIAN_POINT('Ctrl Pts',(97.412559346666,1.11147603473777,-4.09198291036371));
#34517=CARTESIAN_POINT('Ctrl Pts',(97.3706908572507,1.14734013170904,-4.08897813154927));
#34518=CARTESIAN_POINT('Ctrl Pts',(97.32672564806,1.18089297889855,-4.08597335273482));
#34519=CARTESIAN_POINT('Ctrl Pts',(97.2809499775627,1.2118839977969,-4.08296857392038));
#34520=CARTESIAN_POINT('Ctrl Pts',(97.2352195945075,1.24284435621644,-4.07996676783676));
#34521=CARTESIAN_POINT('Ctrl Pts',(97.1876827334991,1.27124761245919,-4.07696496175315));
#34522=CARTESIAN_POINT('Ctrl Pts',(97.1386577814209,1.29688412541374,-4.07396315566953));
#34523=CARTESIAN_POINT('Ctrl Pts',(97.0896619677406,1.32250540108839,-4.07096313373493));
#34524=CARTESIAN_POINT('Ctrl Pts',(97.0391802831046,1.34536294862066,-4.06796311180034));
#34525=CARTESIAN_POINT('Ctrl Pts',(96.9875570892554,1.36529227383068,-4.06496308986574));
#34526=CARTESIAN_POINT('Ctrl Pts',(96.935944189383,1.3852176250128,-4.06196366615365));
#34527=CARTESIAN_POINT('Ctrl Pts',(96.8831907247496,1.40221572339025,-4.05896424244156));
#34528=CARTESIAN_POINT('Ctrl Pts',(96.8296603257169,1.4161704834634,-4.05596481872947));
#34529=CARTESIAN_POINT('Ctrl Pts',(96.7760807132356,1.43013807291725,-4.05296263748172));
#34530=CARTESIAN_POINT('Ctrl Pts',(96.721723251454,1.44105660070094,-4.04996045623396));
#34531=CARTESIAN_POINT('Ctrl Pts',(96.6669645468348,1.44886050883564,-4.0469582749862));
#34532=CARTESIAN_POINT('Ctrl Pts',(96.6121809172688,1.4566679691361,-4.04395472721218));
#34533=CARTESIAN_POINT('Ctrl Pts',(96.5569962079277,1.46135793888929,-4.04095117943817));
#34534=CARTESIAN_POINT('Ctrl Pts',(96.501791674746,1.46291683768627,-4.03794763166415));
#34535=CARTESIAN_POINT('Ctrl Pts',(96.4464829522984,1.46447867864238,-4.03493841519918));
#34536=CARTESIAN_POINT('Ctrl Pts',(96.3911548604652,1.46289765888106,-4.03192919873422));
#34537=CARTESIAN_POINT('Ctrl Pts',(96.3361870071489,1.45821235280589,-4.02891998226925));
#34538=CARTESIAN_POINT('Ctrl Pts',(96.2941343466014,1.45462790163937,-4.02661780834612));
#34539=CARTESIAN_POINT('Ctrl Pts',(96.2522925109856,1.44922763500382,-4.024315634423));
#34540=CARTESIAN_POINT('Ctrl Pts',(96.2108270958956,1.44204896010572,-4.02201346049987));
#34541=CARTESIAN_POINT('Ctrl Pts',(96.1566104126298,1.43266272962009,-4.01900333183863));
#34542=CARTESIAN_POINT('Ctrl Pts',(96.1028098911466,1.42019495131143,-4.01599320317738));
#34543=CARTESIAN_POINT('Ctrl Pts',(96.0498017560758,1.40469742294388,-4.01298307451614));
#34544=CARTESIAN_POINT('Ctrl Pts',(95.9968878313971,1.38922743805099,-4.0099782957017));
#34545=CARTESIAN_POINT('Ctrl Pts',(95.9447640011588,1.37073853610967,-4.00697351688726));
#34546=CARTESIAN_POINT('Ctrl Pts',(95.8937965421099,1.34933355117765,-4.00396873807281));
#34547=CARTESIAN_POINT('Ctrl Pts',(95.8428795069179,1.327949742932,-4.00096693198919));
#34548=CARTESIAN_POINT('Ctrl Pts',(95.7931170611558,1.30365577019171,-3.99796512590557));
#34549=CARTESIAN_POINT('Ctrl Pts',(95.74485875024,1.27660374345999,-3.99496331982195));
#34550=CARTESIAN_POINT('Ctrl Pts',(95.6966291220623,1.24956779533082,-3.99196329788735));
#34551=CARTESIAN_POINT('Ctrl Pts',(95.6499023165267,1.21977730007933,-3.98896327595275));
#34552=CARTESIAN_POINT('Ctrl Pts',(95.6050042598401,1.18743079095867,-3.98596325401815));
#34553=CARTESIAN_POINT('Ctrl Pts',(95.5601151560974,1.1550907319275,-3.98296383030606));
#34554=CARTESIAN_POINT('Ctrl Pts',(95.5170545052516,1.12019597977172,-3.97996440659397));
#34555=CARTESIAN_POINT('Ctrl Pts',(95.4761182182349,1.08298765604447,-3.97696498288188));
#34556=CARTESIAN_POINT('Ctrl Pts',(95.4351442962315,1.04574512465277,-3.97396280163413));
#34557=CARTESIAN_POINT('Ctrl Pts',(95.396299031632,1.00618512821078,-3.97096062038637));
#34558=CARTESIAN_POINT('Ctrl Pts',(95.3598431073006,0.964587264144195,-3.96795843913861));
#34559=CARTESIAN_POINT('Ctrl Pts',(95.3233705890418,0.922970465653291,-3.96495489136459));
#34560=CARTESIAN_POINT('Ctrl Pts',(95.2892899046026,0.879314367459632,-3.96195134359057));
#34561=CARTESIAN_POINT('Ctrl Pts',(95.2578207446867,0.833930861386753,-3.95894779581655));
#34562=CARTESIAN_POINT('Ctrl Pts',(95.2262921920276,0.788461701583897,-3.95593857935158));
#34563=CARTESIAN_POINT('Ctrl Pts',(95.1973852864467,0.741259072640951,-3.95292936288661));
#34564=CARTESIAN_POINT('Ctrl Pts',(95.1712751371105,0.69266198329532,-3.94992014642165));
#34565=CARTESIAN_POINT('Ctrl Pts',(95.1512998027901,0.655483218280164,-3.94761797249853));
#34566=CARTESIAN_POINT('Ctrl Pts',(95.1329604567089,0.617488870375159,-3.94531579857542));
#34567=CARTESIAN_POINT('Ctrl Pts',(95.1163162501074,0.578838069497707,-3.94301362465231));
#34568=CARTESIAN_POINT('Ctrl Pts',(95.0945536878475,0.528301538641816,-3.94000349599107));
#34569=CARTESIAN_POINT('Ctrl Pts',(95.0755993939873,0.47642980884546,-3.93699336732983));
#34570=CARTESIAN_POINT('Ctrl Pts',(95.0596155541659,0.423566280456311,-3.93398323866859));
#34571=CARTESIAN_POINT('Ctrl Pts',(95.0436601221316,0.370796705452491,-3.93097845985415));
#34572=CARTESIAN_POINT('Ctrl Pts',(95.030664818874,0.317039331382095,-3.9279736810397));
#34573=CARTESIAN_POINT('Ctrl Pts',(95.0207436502798,0.262657113005483,-3.92496890222526));
#34574=CARTESIAN_POINT('Ctrl Pts',(95.0108322970383,0.208328696824217,-3.92196709614164));
#34575=CARTESIAN_POINT('Ctrl Pts',(95.0039891480142,0.153377177908357,-3.91896529005802));
#34576=CARTESIAN_POINT('Ctrl Pts',(95.0002777968106,0.0981784225329755,
-3.9159634839744));
#34577=CARTESIAN_POINT('Ctrl Pts',(94.9965686514802,0.0430124750081214,
-3.9129634620398));
#34578=CARTESIAN_POINT('Ctrl Pts',(94.9959876498898,-0.0123998918430344,
-3.9099634401052));
#34579=CARTESIAN_POINT('Ctrl Pts',(94.9985465998968,-0.0676772282603138,
-3.9069634181706));
#34580=CARTESIAN_POINT('Ctrl Pts',(95.0011050396336,-0.122943542042634,
-3.9039639944585));
#34581=CARTESIAN_POINT('Ctrl Pts',(95.0068021631017,-0.178074351609378,
-3.9009645707464));
#34582=CARTESIAN_POINT('Ctrl Pts',(95.0155977090828,-0.232690075720748,
-3.89796514703431));
#34583=CARTESIAN_POINT('Ctrl Pts',(95.0244013412944,-0.287356011079845,
-3.89496296578655));
#34584=CARTESIAN_POINT('Ctrl Pts',(95.0363090029046,-0.341505392380792,
-3.89196078453879));
#34585=CARTESIAN_POINT('Ctrl Pts',(95.0512289596384,-0.394767119773147,
-3.88895860329103));
#34586=CARTESIAN_POINT('Ctrl Pts',(95.0661557076052,-0.448053090721488,
-3.88595505551701));
#34587=CARTESIAN_POINT('Ctrl Pts',(95.0840973125663,-0.50045010182673,-3.88295150774299));
#34588=CARTESIAN_POINT('Ctrl Pts',(95.1049125948635,-0.551603739743897,
-3.87994795996897));
#34589=CARTESIAN_POINT('Ctrl Pts',(95.1257671625031,-0.602853921543803,
-3.87693874350401));
#34590=CARTESIAN_POINT('Ctrl Pts',(95.1495060148721,-0.652855564092704,
-3.87392952703904));
#34591=CARTESIAN_POINT('Ctrl Pts',(95.1759409019906,-0.701276775707584,
-3.87092031057407));
#34592=CARTESIAN_POINT('Ctrl Pts',(95.1961646740234,-0.73832098705067,-3.86861813665096));
#34593=CARTESIAN_POINT('Ctrl Pts',(95.2179654162278,-0.774440645503443,
-3.86631596272785));
#34594=CARTESIAN_POINT('Ctrl Pts',(95.2412421730209,-0.80949926234802,-3.86401378880474));
#34595=CARTESIAN_POINT('Ctrl Pts',(95.2716768991118,-0.855338956007903,
-3.8610036601435));
#34596=CARTESIAN_POINT('Ctrl Pts',(95.3047643170789,-0.899556196763965,
-3.85799353148226));
#34597=CARTESIAN_POINT('Ctrl Pts',(95.3403054374856,-0.941827517176502,
-3.85498340282102));
#34598=CARTESIAN_POINT('Ctrl Pts',(95.375783391307,-0.984023709541916,-3.85197862400658));
#34599=CARTESIAN_POINT('Ctrl Pts',(95.4137060561745,-1.02428044392341,-3.84897384519213));
#34600=CARTESIAN_POINT('Ctrl Pts',(95.453831740077,-1.06230392026625,-3.84596906637768));
#34601=CARTESIAN_POINT('Ctrl Pts',(95.4939177262631,-1.10028977867875,-3.84296726029406));
#34602=CARTESIAN_POINT('Ctrl Pts',(95.5362020324988,-1.13604639437285,-3.83996545421044));
#34603=CARTESIAN_POINT('Ctrl Pts',(95.5804046079581,-1.16931513413738,-3.83696364812682));
#34604=CARTESIAN_POINT('Ctrl Pts',(95.6245809112401,-1.20256410034297,-3.83396362619221));
#34605=CARTESIAN_POINT('Ctrl Pts',(95.6706728027993,-1.23332780453134,-3.83096360425761));
#34606=CARTESIAN_POINT('Ctrl Pts',(95.7183672599627,-1.26138793465255,-3.82796358232301));
#34607=CARTESIAN_POINT('Ctrl Pts',(95.7660522065629,-1.28944246941416,-3.82496415861092));
#34608=CARTESIAN_POINT('Ctrl Pts',(95.8153386292053,-1.31479423310827,-3.82196473489883));
#34609=CARTESIAN_POINT('Ctrl Pts',(95.8658866198142,-1.33726954388932,-3.81896531118674));
#34610=CARTESIAN_POINT('Ctrl Pts',(95.9164810819792,-1.35976551746334,-3.81596312993898));
#34611=CARTESIAN_POINT('Ctrl Pts',(95.9683389456966,-1.37937953976791,-3.81296094869122));
#34612=CARTESIAN_POINT('Ctrl Pts',(96.0210992816066,-1.39598567322575,-3.80995876744346));
#34613=CARTESIAN_POINT('Ctrl Pts',(96.0738836328503,-1.41259936542691,-3.80695521966944));
#34614=CARTESIAN_POINT('Ctrl Pts',(96.1275707623274,-1.42620230958819,-3.80395167189542));
#34615=CARTESIAN_POINT('Ctrl Pts',(96.1817866993122,-1.43671909741234,-3.8009481241214));
#34616=CARTESIAN_POINT('Ctrl Pts',(96.2361049597538,-1.44725573390359,-3.79793890765644));
#34617=CARTESIAN_POINT('Ctrl Pts',(96.2909534968245,-1.45469450736382,-3.79492969119147));
#34618=CARTESIAN_POINT('Ctrl Pts',(96.3459514832574,-1.459011737905,-3.79192047472651));
#34619=CARTESIAN_POINT('Ctrl Pts',(96.3880271968738,-1.46231459620305,-3.7896183008034));
#34620=CARTESIAN_POINT('Ctrl Pts',(96.4301902228732,-1.46379152747159,-3.78731612688029));
#34621=CARTESIAN_POINT('Ctrl Pts',(96.4722710865471,-1.46345250782874,-3.78501395295718));
#34622=CARTESIAN_POINT('Ctrl Pts',(96.5272924785292,-1.46300923430652,-3.78200382429594));
#34623=CARTESIAN_POINT('Ctrl Pts',(96.582404442967,-1.45945775804878,-3.7789936956347));
#34624=CARTESIAN_POINT('Ctrl Pts',(96.6372273401275,-1.45278799672471,-3.77598356697346));
#34625=CARTESIAN_POINT('Ctrl Pts',(96.6919528015522,-1.44613008944585,-3.77297878815902));
#34626=CARTESIAN_POINT('Ctrl Pts',(96.7463896952375,-1.43636495864272,-3.76997400934458));
#34627=CARTESIAN_POINT('Ctrl Pts',(96.8001598961644,-1.42353449668256,-3.76696923053014));
#34628=CARTESIAN_POINT('Ctrl Pts',(96.8538769003859,-1.41071672833884,-3.76396742444652));
#34629=CARTESIAN_POINT('Ctrl Pts',(96.9069280072805,-1.39483975832016,-3.7609656183629));
#34630=CARTESIAN_POINT('Ctrl Pts',(96.9589435859015,-1.375996820559,-3.75796381227928));
#34631=CARTESIAN_POINT('Ctrl Pts',(97.0109282486201,-1.35716508225845,-3.75496379034469));
#34632=CARTESIAN_POINT('Ctrl Pts',(97.0618781074284,-1.33537104981154,-3.75196376841009));
#34633=CARTESIAN_POINT('Ctrl Pts',(97.1114392857495,-1.3107576032843,-3.74896374647549));
#34634=CARTESIAN_POINT('Ctrl Pts',(97.1609905812721,-1.28614906482699,-3.74596432276339));
#34635=CARTESIAN_POINT('Ctrl Pts',(97.2091532735089,-1.25872246358273,-3.7429648990513));
#34636=CARTESIAN_POINT('Ctrl Pts',(97.2555961748016,-1.22866758263414,-3.7399654753392));
#34637=CARTESIAN_POINT('Ctrl Pts',(97.3020817736152,-1.19858507057575,-3.73696329409144));
#34638=CARTESIAN_POINT('Ctrl Pts',(97.3468439783274,-1.16586973885511,-3.73396111284368));
#34639=CARTESIAN_POINT('Ctrl Pts',(97.3895801024427,-1.13075506372698,-3.73095893159592));
#34640=CARTESIAN_POINT('Ctrl Pts',(97.432335679093,-1.09562440517823,-3.72795538382191));
#34641=CARTESIAN_POINT('Ctrl Pts',(97.4730629477146,-1.05809258465269,-3.72495183604789));
#34642=CARTESIAN_POINT('Ctrl Pts',(97.5114944156926,-1.01843160990011,-3.72194828827388));
#34643=CARTESIAN_POINT('Ctrl Pts',(97.5499984165987,-0.978695781732321,
-3.71893907180891));
#34644=CARTESIAN_POINT('Ctrl Pts',(97.5861976149122,-0.936823172417264,
-3.71592985534394));
#34645=CARTESIAN_POINT('Ctrl Pts',(97.6198640955659,-0.893119796442222,
-3.71292063887898));
#34646=CARTESIAN_POINT('Ctrl Pts',(97.6456203330272,-0.859684922715666,
-3.71061846495586));
#34647=CARTESIAN_POINT('Ctrl Pts',(97.6698950146036,-0.825179243157338,
-3.70831629103274));
#34648=CARTESIAN_POINT('Ctrl Pts',(97.692603895247,-0.789750148308665,-3.70601411710962));
#34649=CARTESIAN_POINT('Ctrl Pts',(97.7229545537649,-0.742398789329823,
-3.70293723737755));
#34650=CARTESIAN_POINT('Ctrl Pts',(97.7506298434866,-0.693205203985186,
-3.69986035764549));
#34651=CARTESIAN_POINT('Ctrl Pts',(97.775407355941,-0.642495755508686,-3.69678347791342));
#34652=CARTESIAN_POINT('Ctrl Pts',(97.8001289484294,-0.591900752364011,
-3.69371354234132));
#34653=CARTESIAN_POINT('Ctrl Pts',(97.8219655452006,-0.539797128016443,
-3.69064360676921));
#34654=CARTESIAN_POINT('Ctrl Pts',(97.8407392857753,-0.486537948525319,
-3.68757367119711));
#34655=CARTESIAN_POINT('Ctrl Pts',(97.8594879712184,-0.433349847876592,
-3.68450783271154));
#34656=CARTESIAN_POINT('Ctrl Pts',(97.8751817456071,-0.379009717014779,
-3.68144199422596));
#34657=CARTESIAN_POINT('Ctrl Pts',(97.8876902586357,-0.323891707420963,
-3.67837615574039));
#34658=CARTESIAN_POINT('Ctrl Pts',(97.9001850500302,-0.268834161382075,
-3.67531368042948));
#34659=CARTESIAN_POINT('Ctrl Pts',(97.9095014086337,-0.213000913674018,
-3.67225120511857));
#34660=CARTESIAN_POINT('Ctrl Pts',(97.9155589979105,-0.156780493869258,
-3.66918872980767));
#34661=CARTESIAN_POINT('Ctrl Pts',(97.9211855523835,-0.104560503363353,
-3.66634416848608));
#34662=CARTESIAN_POINT('Ctrl Pts',(97.9240010364998,-0.0520069428674101,
-3.66349960716449));
#34663=CARTESIAN_POINT('Ctrl Pts',(97.9239808415867,0.000562216580854143,
-3.6606550458429));
#34664=CARTESIAN_POINT('Ctrl Pts',(97.9239808649785,0.000497614024185356,
-3.58934495415707));
#34665=CARTESIAN_POINT('Ctrl Pts',(97.9240001510924,-0.056223508595772,
-3.59241382882926));
#34666=CARTESIAN_POINT('Ctrl Pts',(97.9207175741498,-0.112920864306401,
-3.59548270350144));
#34667=CARTESIAN_POINT('Ctrl Pts',(97.9141675493034,-0.169196689612829,
-3.59855157817363));
#34668=CARTESIAN_POINT('Ctrl Pts',(97.9076060721981,-0.225570909251625,
-3.60162581855787));
#34669=CARTESIAN_POINT('Ctrl Pts',(97.8977657979204,-0.281521635888496,
-3.60470005894212));
#34670=CARTESIAN_POINT('Ctrl Pts',(97.8847328229594,-0.336658359716137,
-3.60777429932636));
#34671=CARTESIAN_POINT('Ctrl Pts',(97.871688408699,-0.391843478134799,-3.61085123803208));
#34672=CARTESIAN_POINT('Ctrl Pts',(97.8554458536868,-0.446212697850251,
-3.61392817673781));
#34673=CARTESIAN_POINT('Ctrl Pts',(97.8361411092636,-0.499391004175057,
-3.61700511544353));
#34674=CARTESIAN_POINT('Ctrl Pts',(97.8167895597394,-0.552698243364627,
-3.6200895143064));
#34675=CARTESIAN_POINT('Ctrl Pts',(97.794361178821,-0.604808344405963,-3.62317391316927));
#34676=CARTESIAN_POINT('Ctrl Pts',(97.7690398263078,-0.65536700872792,-3.62625831203214));
#34677=CARTESIAN_POINT('Ctrl Pts',(97.7478753772047,-0.697625662850288,
-3.62883635768405));
#34678=CARTESIAN_POINT('Ctrl Pts',(97.7246907636451,-0.738800758044961,
-3.63141440333595));
#34679=CARTESIAN_POINT('Ctrl Pts',(97.6996164354008,-0.77870116076208,-3.63399244898786));
#34680=CARTESIAN_POINT('Ctrl Pts',(97.6703396248627,-0.825288910565818,
-3.6370025776491));
#34681=CARTESIAN_POINT('Ctrl Pts',(97.6383703097217,-0.870321171193224,
-3.64001270631033));
#34682=CARTESIAN_POINT('Ctrl Pts',(97.6038993135423,-0.913469591692513,
-3.64302283497157));
#34683=CARTESIAN_POINT('Ctrl Pts',(97.569489582036,-0.956541325290655,-3.64602761378601));
#34684=CARTESIAN_POINT('Ctrl Pts',(97.5325873199565,-0.997735453842115,
-3.64903239260045));
#34685=CARTESIAN_POINT('Ctrl Pts',(97.4934267832603,-1.03675221469564,-3.6520371714149));
#34686=CARTESIAN_POINT('Ctrl Pts',(97.4543049894273,-1.07573037492832,-3.65503897749851));
#34687=CARTESIAN_POINT('Ctrl Pts',(97.4129297190792,-1.11253506380539,-3.65804078358213));
#34688=CARTESIAN_POINT('Ctrl Pts',(97.3695744559394,-1.14690071352742,-3.66104258966574));
#34689=CARTESIAN_POINT('Ctrl Pts',(97.3262449613696,-1.18124593773276,-3.66404261160034));
#34690=CARTESIAN_POINT('Ctrl Pts',(97.2809382195961,-1.21315466871269,-3.66704263353494));
#34691=CARTESIAN_POINT('Ctrl Pts',(97.2339616859562,-1.24240082117255,-3.67004265546953));
#34692=CARTESIAN_POINT('Ctrl Pts',(97.1869945197212,-1.27164114177282,-3.67304207918162));
#34693=CARTESIAN_POINT('Ctrl Pts',(97.1383586709566,-1.29821965930521,-3.6760415028937));
#34694=CARTESIAN_POINT('Ctrl Pts',(97.0883895900285,-1.32195423114661,-3.67904092660579));
#34695=CARTESIAN_POINT('Ctrl Pts',(97.0383745697679,-1.34571062348912,-3.68204310785355));
#34696=CARTESIAN_POINT('Ctrl Pts',(96.98702434659,-1.36661761944437,-3.6850452891013));
#34697=CARTESIAN_POINT('Ctrl Pts',(96.9346965816245,-1.38454027905359,-3.68804747034906));
#34698=CARTESIAN_POINT('Ctrl Pts',(96.8823449982221,-1.40247109665959,-3.69105101812307));
#34699=CARTESIAN_POINT('Ctrl Pts',(96.8290154954596,-1.41741472729064,-3.69405456589709));
#34700=CARTESIAN_POINT('Ctrl Pts',(96.7750800375856,-1.42928641770085,-3.6970581136711));
#34701=CARTESIAN_POINT('Ctrl Pts',(96.7210427856119,-1.4411805139288,-3.70006733013607));
#34702=CARTESIAN_POINT('Ctrl Pts',(96.6663978165935,-1.44999100372014,-3.70307654660103));
#34703=CARTESIAN_POINT('Ctrl Pts',(96.6115252450547,-1.45568467423534,-3.706085763066));
#34704=CARTESIAN_POINT('Ctrl Pts',(96.5695454789716,-1.46004056552455,-3.70838793698914));
#34705=CARTESIAN_POINT('Ctrl Pts',(96.5274326852702,-1.46257329016688,-3.71069011091228));
#34706=CARTESIAN_POINT('Ctrl Pts',(96.4853565353895,-1.46328857551424,-3.71299228483542));
#34707=CARTESIAN_POINT('Ctrl Pts',(96.430341306767,-1.46422382237087,-3.71600241349666));
#34708=CARTESIAN_POINT('Ctrl Pts',(96.3751576682472,-1.46205411097958,-3.7190125421579));
#34709=CARTESIAN_POINT('Ctrl Pts',(96.3201848878356,-1.45675985154034,-3.72202267081915));
#34710=CARTESIAN_POINT('Ctrl Pts',(96.2653098095444,-1.45147500149189,-3.72502744963359));
#34711=CARTESIAN_POINT('Ctrl Pts',(96.2106453670913,-1.44307667398024,-3.72803222844804));
#34712=CARTESIAN_POINT('Ctrl Pts',(96.1565706162991,-1.43159727553768,-3.73103700726248));
#34713=CARTESIAN_POINT('Ctrl Pts',(96.102549363514,-1.42012923405805,-3.7340388133461));
#34714=CARTESIAN_POINT('Ctrl Pts',(96.0491171607622,-1.40558626913281,-3.73704061942973));
#34715=CARTESIAN_POINT('Ctrl Pts',(95.9966458586558,-1.38805232553751,-3.74004242551335));
#34716=CARTESIAN_POINT('Ctrl Pts',(95.9442057433148,-1.37052880339098,-3.74304244744795));
#34717=CARTESIAN_POINT('Ctrl Pts',(95.8927258965131,-1.35001799316413,-3.74604246938254));
#34718=CARTESIAN_POINT('Ctrl Pts',(95.842563663159,-1.32665386485917,-3.74904249131714));
#34719=CARTESIAN_POINT('Ctrl Pts',(95.7924114324574,-1.30329439550263,-3.75204191502923));
#34720=CARTESIAN_POINT('Ctrl Pts',(95.7435767718786,-1.2770829608713,-3.75504133874132));
#34721=CARTESIAN_POINT('Ctrl Pts',(95.6963955195345,-1.24820098766054,-3.75804076245341));
#34722=CARTESIAN_POINT('Ctrl Pts',(95.6491708908625,-1.21929246165864,-3.76104294370117));
#34723=CARTESIAN_POINT('Ctrl Pts',(95.6036031587181,-1.18770876827886,-3.76404512494893));
#34724=CARTESIAN_POINT('Ctrl Pts',(95.5600007635854,-1.15367572767935,-3.76704730619669));
#34725=CARTESIAN_POINT('Ctrl Pts',(95.5163785216103,-1.11962719599523,-3.77005085397072));
#34726=CARTESIAN_POINT('Ctrl Pts',(95.4747237978213,-1.08312744329179,-3.77305440174474));
#34727=CARTESIAN_POINT('Ctrl Pts',(95.4353108151481,-1.04444169079708,-3.77605794951876));
#34728=CARTESIAN_POINT('Ctrl Pts',(95.3958234471031,-1.00568292545508,-3.77906716598373));
#34729=CARTESIAN_POINT('Ctrl Pts',(95.35858662823,-0.964730310280806,-3.7820763824487));
#34730=CARTESIAN_POINT('Ctrl Pts',(95.3238358682598,-0.921884054053179,
-3.78508559891367));
#34731=CARTESIAN_POINT('Ctrl Pts',(95.2972501126844,-0.889104912061163,
-3.78738777283677));
#34732=CARTESIAN_POINT('Ctrl Pts',(95.2721186224739,-0.855218184759803,
-3.78968994675988));
#34733=CARTESIAN_POINT('Ctrl Pts',(95.2485293086253,-0.820369105948374,
-3.79199212068299));
#34734=CARTESIAN_POINT('Ctrl Pts',(95.2176859092619,-0.774803386566738,
-3.79500224934422));
#34735=CARTESIAN_POINT('Ctrl Pts',(95.1893509774879,-0.727400082365858,
-3.79801237800546));
#34736=CARTESIAN_POINT('Ctrl Pts',(95.1637481508373,-0.678466136717841,
-3.80102250666669));
#34737=CARTESIAN_POINT('Ctrl Pts',(95.1381908276239,-0.629619160479316,
-3.80402728548114));
#34738=CARTESIAN_POINT('Ctrl Pts',(95.1153562161736,-0.579247405560317,
-3.80703206429558));
#34739=CARTESIAN_POINT('Ctrl Pts',(95.0954242897573,-0.527686048216158,
-3.81003684311002));
#34740=CARTESIAN_POINT('Ctrl Pts',(95.07551208268,-0.476175702292761,-3.81303864919364));
#34741=CARTESIAN_POINT('Ctrl Pts',(95.0584970613695,-0.423478575525552,
-3.81604045527726));
#34742=CARTESIAN_POINT('Ctrl Pts',(95.0445120975315,-0.369951969905599,
-3.81904226136088));
#34743=CARTESIAN_POINT('Ctrl Pts',(95.030535445776,-0.316457178279727,-3.82204228329547));
#34744=CARTESIAN_POINT('Ctrl Pts',(95.0195854151447,-0.26213439491896,-3.82504230523007));
#34745=CARTESIAN_POINT('Ctrl Pts',(95.0117450540103,-0.207356106484561,
-3.82804232716467));
#34746=CARTESIAN_POINT('Ctrl Pts',(95.0039062562912,-0.152588741172005,
-3.83104175087676));
#34747=CARTESIAN_POINT('Ctrl Pts',(94.9991759713874,-0.0973665736664746,
-3.83404117458884));
#34748=CARTESIAN_POINT('Ctrl Pts',(94.9975857501847,-0.0420700082593357,
-3.83704059830093));
#34749=CARTESIAN_POINT('Ctrl Pts',(94.9959940670039,0.0132773943305955,
-3.84004277954869));
#34750=CARTESIAN_POINT('Ctrl Pts',(94.997548230257,0.0686988024404475,-3.84304496079645));
#34751=CARTESIAN_POINT('Ctrl Pts',(95.0022276401538,0.1238125016156,-3.84604714204421));
#34752=CARTESIAN_POINT('Ctrl Pts',(95.0069091800141,0.178951287323153,-3.84905068981822));
#34753=CARTESIAN_POINT('Ctrl Pts',(95.0147187276608,0.233781561140536,-3.85205423759224));
#34754=CARTESIAN_POINT('Ctrl Pts',(95.0255839875099,0.287928738146205,-3.85505778536626));
#34755=CARTESIAN_POINT('Ctrl Pts',(95.0364697537083,0.342178108835892,-3.85806700183122));
#34756=CARTESIAN_POINT('Ctrl Pts',(95.050422619417,0.395741294961268,-3.86107621829619));
#34757=CARTESIAN_POINT('Ctrl Pts',(95.0673198332966,0.4482570178862,-3.86408543476115));
#34758=CARTESIAN_POINT('Ctrl Pts',(95.080246894417,0.48843369818816,-3.86638760868429));
#34759=CARTESIAN_POINT('Ctrl Pts',(95.0948961929289,0.527997572373446,-3.86868978260742));
#34760=CARTESIAN_POINT('Ctrl Pts',(95.1111941258405,0.56679565743835,-3.87099195653056));
#34761=CARTESIAN_POINT('Ctrl Pts',(95.1325039297971,0.617524764688423,-3.87400208519179));
#34762=CARTESIAN_POINT('Ctrl Pts',(95.1567233773382,0.667157011953762,-3.87701221385303));
#34763=CARTESIAN_POINT('Ctrl Pts',(95.1837175897996,0.715337384127176,-3.88002234251427));
#34764=CARTESIAN_POINT('Ctrl Pts',(95.2106638259394,0.763432126203506,-3.88302712132871));
#34765=CARTESIAN_POINT('Ctrl Pts',(95.2403747842794,0.810079656987281,-3.88603190014316));
#34766=CARTESIAN_POINT('Ctrl Pts',(95.272668082374,0.854946105030524,-3.8890366789576));
#34767=CARTESIAN_POINT('Ctrl Pts',(95.3049294316002,0.899768165156598,-3.89203848504122));
#34768=CARTESIAN_POINT('Ctrl Pts',(95.3397677526525,0.942812206625506,-3.89504029112484));
#34769=CARTESIAN_POINT('Ctrl Pts',(95.376956396076,0.983771717402203,-3.89804209720846));
#34770=CARTESIAN_POINT('Ctrl Pts',(95.4141229361124,1.02470688354471,-3.90104211914306));
#34771=CARTESIAN_POINT('Ctrl Pts',(95.4536366754115,1.06355958447403,-3.90404214107766));
#34772=CARTESIAN_POINT('Ctrl Pts',(95.4952310236744,1.10005673969343,-3.90704216301226));
#34773=CARTESIAN_POINT('Ctrl Pts',(95.5368170777728,1.13654661715947,-3.91004158672435));
#34774=CARTESIAN_POINT('Ctrl Pts',(95.5804825201473,1.17068153361645,-3.91304101043644));
#34775=CARTESIAN_POINT('Ctrl Pts',(95.6259259912463,1.20222721293675,-3.91604043414853));
#34776=CARTESIAN_POINT('Ctrl Pts',(95.671411241035,1.23380189394011,-3.91904261539629));
#34777=CARTESIAN_POINT('Ctrl Pts',(95.7186773505804,1.26278228021673,-3.92204479664405));
#34778=CARTESIAN_POINT('Ctrl Pts',(95.7673933681092,1.28897705736568,-3.9250469778918));
#34779=CARTESIAN_POINT('Ctrl Pts',(95.8161315600878,1.31518375779572,-3.92805052566582));
#34780=CARTESIAN_POINT('Ctrl Pts',(95.8663204962306,1.33860209783507,-3.93105407343984));
#34781=CARTESIAN_POINT('Ctrl Pts',(95.9176069495612,1.35908795525045,-3.93405762121386));
#34782=CARTESIAN_POINT('Ctrl Pts',(95.9689901974413,1.37961247627406,-3.93706683767883));
#34783=CARTESIAN_POINT('Ctrl Pts',(96.0214745984137,1.3971932903609,-3.9400760541438));
#34784=CARTESIAN_POINT('Ctrl Pts',(96.0746905010476,1.41173580383282,-3.94308527060876));
#34785=CARTESIAN_POINT('Ctrl Pts',(96.1154028475223,1.42286142263805,-3.94538744453188));
#34786=CARTESIAN_POINT('Ctrl Pts',(96.1565429761317,1.43220978642091,-3.947689618455));
#34787=CARTESIAN_POINT('Ctrl Pts',(96.1979425431072,1.43975895035534,-3.94999179237811));
#34788=CARTESIAN_POINT('Ctrl Pts',(96.2520731289264,1.44962960109082,-3.95300192103935));
#34789=CARTESIAN_POINT('Ctrl Pts',(96.306874882821,1.45646402702742,-3.9560120497006));
#34790=CARTESIAN_POINT('Ctrl Pts',(96.3619767729118,1.46018121381543,-3.95902217836184));
#34791=CARTESIAN_POINT('Ctrl Pts',(96.4169807314178,1.46389179411512,-3.96202695717628));
#34792=CARTESIAN_POINT('Ctrl Pts',(96.4722832448745,1.46449609459621,-3.96503173599072));
#34793=CARTESIAN_POINT('Ctrl Pts',(96.5275050339065,1.46196443941698,-3.96803651480517));
#34794=CARTESIAN_POINT('Ctrl Pts',(96.582672190127,1.45943528889111,-3.97103832088879));
#34795=CARTESIAN_POINT('Ctrl Pts',(96.63775825516,1.45377635269252,-3.97404012697241));
#34796=CARTESIAN_POINT('Ctrl Pts',(96.6923826765546,1.44500997886685,-3.97704193305603));
#34797=CARTESIAN_POINT('Ctrl Pts',(96.746974631459,1.43624881541015,-3.98004195499063));
#34798=CARTESIAN_POINT('Ctrl Pts',(96.801104966165,1.42438395858349,-3.98304197692523));
#34799=CARTESIAN_POINT('Ctrl Pts',(96.8543993045145,1.40948947482533,-3.98604199885983));
#34800=CARTESIAN_POINT('Ctrl Pts',(96.9076830156505,1.3945979611173,-3.98904142257191));
#34801=CARTESIAN_POINT('Ctrl Pts',(96.9601305531537,1.37667816231497,-3.99204084628399));
#34802=CARTESIAN_POINT('Ctrl Pts',(97.0113810427862,1.35585446759676,-3.99504026999608));
#34803=CARTESIAN_POINT('Ctrl Pts',(97.0626786498209,1.3350116285073,-3.99804245124383));
#34804=CARTESIAN_POINT('Ctrl Pts',(97.112776519982,1.31125975898894,-4.00104463249159));
#34805=CARTESIAN_POINT('Ctrl Pts',(97.1613335915602,1.28477150662102,-4.00404681373935));
#34806=CARTESIAN_POINT('Ctrl Pts',(97.2099127652393,1.25827119738863,-4.00705036151336));
#34807=CARTESIAN_POINT('Ctrl Pts',(97.2569492929646,1.22903230170353,-4.01005390928738));
#34808=CARTESIAN_POINT('Ctrl Pts',(97.3021294666536,1.19727190884227,-4.01305745706139));
#34809=CARTESIAN_POINT('Ctrl Pts',(97.3473949103169,1.16545157358449,-4.01606667352636));
#34810=CARTESIAN_POINT('Ctrl Pts',(97.3907965859239,1.13110056306223,-4.01907588999133));
#34811=CARTESIAN_POINT('Ctrl Pts',(97.4320532926325,1.09447678468282,-4.0220851064563));
#34812=CARTESIAN_POINT('Ctrl Pts',(97.4636163640979,1.06645809326165,-4.02438728037942));
#34813=CARTESIAN_POINT('Ctrl Pts',(97.49392467513,1.03711003762231,-4.02668945430255));
#34814=CARTESIAN_POINT('Ctrl Pts',(97.5228678639721,1.0065616196349,-4.02899162822567));
#34815=CARTESIAN_POINT('Ctrl Pts',(97.5602276477705,0.967129810734345,-4.03196326761564));
#34816=CARTESIAN_POINT('Ctrl Pts',(97.5954772999918,0.925521827568755,-4.03493490700561));
#34817=CARTESIAN_POINT('Ctrl Pts',(97.6283492700598,0.881995371877195,-4.03790654639557));
#34818=CARTESIAN_POINT('Ctrl Pts',(97.6611738936125,0.838531608686043,-4.04087390564142));
#34819=CARTESIAN_POINT('Ctrl Pts',(97.6916272888325,0.793155270469379,-4.04384126488726));
#34820=CARTESIAN_POINT('Ctrl Pts',(97.7194797349499,0.746159707053038,-4.0468086241331));
#34821=CARTESIAN_POINT('Ctrl Pts',(97.7473037456196,0.699212122901529,-4.04977295390754));
#34822=CARTESIAN_POINT('Ctrl Pts',(97.7725317904146,0.650649051771042,-4.05273728368199));
#34823=CARTESIAN_POINT('Ctrl Pts',(97.794976850279,0.600793592683606,-4.05570161345643));
#34824=CARTESIAN_POINT('Ctrl Pts',(97.8174158723574,0.550951544858702,-4.0586651458176));
#34825=CARTESIAN_POINT('Ctrl Pts',(97.8370731533352,0.499818284313263,-4.06162867817877));
#34826=CARTESIAN_POINT('Ctrl Pts',(97.853808172062,0.447740439409174,-4.06459221053994));
#34827=CARTESIAN_POINT('Ctrl Pts',(97.8705396784872,0.39567352446584,-4.06755512092275));
#34828=CARTESIAN_POINT('Ctrl Pts',(97.8843499799722,0.34266293753326,-4.07051803130557));
#34829=CARTESIAN_POINT('Ctrl Pts',(97.895148151909,0.289071390062761,-4.07348094168838));
#34830=CARTESIAN_POINT('Ctrl Pts',(97.9059561540758,0.235431054960567,-4.07644654938798));
#34831=CARTESIAN_POINT('Ctrl Pts',(97.9137464504333,0.181209237719674,-4.07941215708758));
#34832=CARTESIAN_POINT('Ctrl Pts',(97.9184794312525,0.126778063685683,-4.08237776478718));
#34833=CARTESIAN_POINT('Ctrl Pts',(97.9221858749218,0.084152477798513,-4.08470016124381));
#34834=CARTESIAN_POINT('Ctrl Pts',(97.9240184185765,0.0413987541311476,
-4.08702255770044));
#34835=CARTESIAN_POINT('Ctrl Pts',(97.9239803686004,-0.0013040392330809,
-4.08934495415707));
#34836=CARTESIAN_POINT('Origin',(96.460480949577,-8.32667268468867E-16,
1.18130019239114E-14));
#34837=CARTESIAN_POINT('',(97.9239807839468,0.000696275558457232,-4.66065504587649));
#34838=CARTESIAN_POINT('',(97.9239807519797,0.000760504599680839,-4.58934495419114));
#34839=CARTESIAN_POINT('',(97.923980949577,-1.01189432752408E-15,1.19922289829666E-14));
#34840=CARTESIAN_POINT('Ctrl Pts',(97.9239807839465,0.000696276173079623,
-4.6606550458429));
#34841=CARTESIAN_POINT('Ctrl Pts',(97.9239615067044,0.0412150267063342,
-4.65844074632205));
#34842=CARTESIAN_POINT('Ctrl Pts',(97.9222596535451,0.0816919370260447,
-4.65622644680121));
#34843=CARTESIAN_POINT('Ctrl Pts',(97.9188847609986,0.122026934858089,-4.65401214728037));
#34844=CARTESIAN_POINT('Ctrl Pts',(97.9142969169933,0.176858511111745,-4.65100201861913));
#34845=CARTESIAN_POINT('Ctrl Pts',(97.9066028816966,0.231546201030747,-4.64799188995788));
#34846=CARTESIAN_POINT('Ctrl Pts',(97.8958212070784,0.285710684427393,-4.64498176129664));
#34847=CARTESIAN_POINT('Ctrl Pts',(97.8850586945338,0.339778902275131,-4.64197698248219));
#34848=CARTESIAN_POINT('Ctrl Pts',(97.8712195351239,0.393325245199246,-4.63897220366774));
#34849=CARTESIAN_POINT('Ctrl Pts',(97.8543739936292,0.445975819684259,-4.63596742485329));
#34850=CARTESIAN_POINT('Ctrl Pts',(97.8375451180069,0.49857430514863,-4.63296561876967));
#34851=CARTESIAN_POINT('Ctrl Pts',(97.8177159124216,0.550278277197155,-4.62996381268604));
#34852=CARTESIAN_POINT('Ctrl Pts',(97.7950071972413,0.600726180797032,-4.62696200660241));
#34853=CARTESIAN_POINT('Ctrl Pts',(97.7723119791794,0.651144100255606,-4.62396198466781));
#34854=CARTESIAN_POINT('Ctrl Pts',(97.746740860095,0.700306950373101,-4.6209619627332));
#34855=CARTESIAN_POINT('Ctrl Pts',(97.7184629782722,0.747872626507885,-4.61796194079859));
#34856=CARTESIAN_POINT('Ctrl Pts',(97.6901907352301,0.795428817759335,-4.61496251708649));
#34857=CARTESIAN_POINT('Ctrl Pts',(97.6592130710845,0.841388013829169,-4.61196309337439));
#34858=CARTESIAN_POINT('Ctrl Pts',(97.6257441842029,0.885434268610102,-4.60896366966229));
#34859=CARTESIAN_POINT('Ctrl Pts',(97.5922445275275,0.929521017542661,-4.60596148841453));
#34860=CARTESIAN_POINT('Ctrl Pts',(97.5562493925602,0.971690890188859,-4.60295930716676));
#34861=CARTESIAN_POINT('Ctrl Pts',(97.5180143990828,1.01165965283609,-4.59995712591899));
#34862=CARTESIAN_POINT('Ctrl Pts',(97.4797620018851,1.05164660837684,-4.59695357814496));
#34863=CARTESIAN_POINT('Ctrl Pts',(97.4392681006136,1.08943009579091,-4.59395003037094));
#34864=CARTESIAN_POINT('Ctrl Pts',(97.3968240851684,1.12476387852332,-4.59094648259691));
#34865=CARTESIAN_POINT('Ctrl Pts',(97.3542999637872,1.1601643478242,-4.58793726613193));
#34866=CARTESIAN_POINT('Ctrl Pts',(97.3098188012856,1.19310556140108,-4.58492804966696));
#34867=CARTESIAN_POINT('Ctrl Pts',(97.2637029154812,1.22338331012362,-4.58191883320198));
#34868=CARTESIAN_POINT('Ctrl Pts',(97.2284223728636,1.24654702877576,-4.57961665927892));
#34869=CARTESIAN_POINT('Ctrl Pts',(97.1921857029053,1.26815271871278,-4.57731448535586));
#34870=CARTESIAN_POINT('Ctrl Pts',(97.1551462249608,1.28812748017268,-4.5750123114328));
#34871=CARTESIAN_POINT('Ctrl Pts',(97.1067165242152,1.31424479536312,-4.57200218277157));
#34872=CARTESIAN_POINT('Ctrl Pts',(97.0567101214196,1.33768197282204,-4.56899205411033));
#34873=CARTESIAN_POINT('Ctrl Pts',(97.005454844163,1.35824729126172,-4.56598192544909));
#34874=CARTESIAN_POINT('Ctrl Pts',(96.9542906619762,1.37877605933586,-4.56297714663465));
#34875=CARTESIAN_POINT('Ctrl Pts',(96.9018824963136,1.39644290244907,-4.55997236782021));
#34876=CARTESIAN_POINT('Ctrl Pts',(96.8485818854573,1.41110237529701,-4.55696758900576));
#34877=CARTESIAN_POINT('Ctrl Pts',(96.7953340067249,1.42574734502525,-4.55396578292214));
#34878=CARTESIAN_POINT('Ctrl Pts',(96.7411959385386,1.4373906990429,-4.55096397683853));
#34879=CARTESIAN_POINT('Ctrl Pts',(96.6865365087437,1.44593607540922,-4.54796217075491));
#34880=CARTESIAN_POINT('Ctrl Pts',(96.6319095662466,1.45447637275829,-4.54496214882031));
#34881=CARTESIAN_POINT('Ctrl Pts',(96.5767623970712,1.45992226064101,-4.54196212688571));
#34882=CARTESIAN_POINT('Ctrl Pts',(96.5214739395565,1.46222847228925,-4.53896210495112));
#34883=CARTESIAN_POINT('Ctrl Pts',(96.4661965068944,1.46453422406495,-4.53596268123903));
#34884=CARTESIAN_POINT('Ctrl Pts',(96.4107783692063,1.46370152095767,-4.53296325752694));
#34885=CARTESIAN_POINT('Ctrl Pts',(96.3556011770071,1.45973712815208,-4.52996383381485));
#34886=CARTESIAN_POINT('Ctrl Pts',(96.3003732573715,1.45576909066151,-4.52696165256709));
#34887=CARTESIAN_POINT('Ctrl Pts',(96.2453872536722,1.44866364926291,-4.52395947131933));
#34888=CARTESIAN_POINT('Ctrl Pts',(96.1910208889382,1.43847958821824,-4.52095729007157));
#34889=CARTESIAN_POINT('Ctrl Pts',(96.1366297778418,1.42829089161505,-4.51795374229756));
#34890=CARTESIAN_POINT('Ctrl Pts',(96.0828593815767,1.41502090869013,-4.51495019452354));
#34891=CARTESIAN_POINT('Ctrl Pts',(96.0300751441821,1.39877914364003,-4.51194664674952));
#34892=CARTESIAN_POINT('Ctrl Pts',(95.9771912854226,1.38250672499177,-4.50893743028456));
#34893=CARTESIAN_POINT('Ctrl Pts',(95.9252977999323,1.36325150406209,-4.50592821381959));
#34894=CARTESIAN_POINT('Ctrl Pts',(95.8747418315436,1.34117185163032,-4.50291899735463));
#34895=CARTESIAN_POINT('Ctrl Pts',(95.8360644437792,1.3242800126244,-4.5006168234315));
#34896=CARTESIAN_POINT('Ctrl Pts',(95.7981695227691,1.30573609046451,-4.49831464950837));
#34897=CARTESIAN_POINT('Ctrl Pts',(95.7612018971196,1.28562866209272,-4.49601247558525));
#34898=CARTESIAN_POINT('Ctrl Pts',(95.7128661443829,1.25933788282638,-4.49300234692401));
#34899=CARTESIAN_POINT('Ctrl Pts',(95.665913575316,1.23026215642405,-4.48999221826277));
#34900=CARTESIAN_POINT('Ctrl Pts',(95.620683885365,1.19857129155546,-4.48698208960154));
#34901=CARTESIAN_POINT('Ctrl Pts',(95.5755345813174,1.16693675028326,-4.48397731078709));
#34902=CARTESIAN_POINT('Ctrl Pts',(95.5321025087596,1.13269659480699,-4.48097253197265));
#34903=CARTESIAN_POINT('Ctrl Pts',(95.4907015611857,1.09606577715547,-4.47796775315821));
#34904=CARTESIAN_POINT('Ctrl Pts',(95.4493415729904,1.05947119962927,-4.47496594707459));
#34905=CARTESIAN_POINT('Ctrl Pts',(95.4100091227119,1.02049099343673,-4.47196414099097));
#34906=CARTESIAN_POINT('Ctrl Pts',(95.3729864421558,0.979381410038385,-4.46896233490735));
#34907=CARTESIAN_POINT('Ctrl Pts',(95.3359857663454,0.938296260471181,-4.46596231297275));
#34908=CARTESIAN_POINT('Ctrl Pts',(95.3012924919278,0.89508463387512,-4.46296229103815));
#34909=CARTESIAN_POINT('Ctrl Pts',(95.2691515814606,0.85003916772303,-4.45996226910356));
#34910=CARTESIAN_POINT('Ctrl Pts',(95.2370170800852,0.805002683909167,-4.45696284539147));
#34911=CARTESIAN_POINT('Ctrl Pts',(95.2074342384654,0.758133516421519,-4.45396342167937));
#34912=CARTESIAN_POINT('Ctrl Pts',(95.1806059229202,0.709755004308049,-4.45096399796728));
#34913=CARTESIAN_POINT('Ctrl Pts',(95.1537529426247,0.661332015159822,-4.44796181671952));
#34914=CARTESIAN_POINT('Ctrl Pts',(95.1296598044568,0.611397371939726,-4.44495963547177));
#34915=CARTESIAN_POINT('Ctrl Pts',(95.1084836613955,0.560299547340288,-4.44195745422401));
#34916=CARTESIAN_POINT('Ctrl Pts',(95.0872978794238,0.509178464145387,-4.43895390644999));
#34917=CARTESIAN_POINT('Ctrl Pts',(95.0690319138202,0.456893643576649,-4.43595035867597));
#34918=CARTESIAN_POINT('Ctrl Pts',(95.0537937290614,0.40381098751529,-4.43294681090195));
#34919=CARTESIAN_POINT('Ctrl Pts',(95.0385267847933,0.350628146874057,-4.42993759443699));
#34920=CARTESIAN_POINT('Ctrl Pts',(95.0262991537784,0.296644979042319,-4.42692837797202));
#34921=CARTESIAN_POINT('Ctrl Pts',(95.017167874254,0.242238759494667,-4.42391916150706));
#34922=CARTESIAN_POINT('Ctrl Pts',(95.0101820711884,0.200615771797781,-4.42161698758393));
#34923=CARTESIAN_POINT('Ctrl Pts',(95.0050074689897,0.158745429316313,-4.4193148136608));
#34924=CARTESIAN_POINT('Ctrl Pts',(95.0016490158668,0.116797427999157,-4.41701263973768));
#34925=CARTESIAN_POINT('Ctrl Pts',(94.9972577855166,0.0619497556413082,
-4.41400251107644));
#34926=CARTESIAN_POINT('Ctrl Pts',(94.9959547894712,0.00673885265002533,
-4.4109923824152));
#34927=CARTESIAN_POINT('Ctrl Pts',(94.997783416658,-0.0484579941058989,
-4.40798225375396));
#34928=CARTESIAN_POINT('Ctrl Pts',(94.9996087938591,-0.103556740512358,
-4.40497747493951));
#34929=CARTESIAN_POINT('Ctrl Pts',(95.0045547316256,-0.158640956702821,
-4.40197269612507));
#34930=CARTESIAN_POINT('Ctrl Pts',(95.0126127120214,-0.213330299483491,
-4.39896791731062));
#34931=CARTESIAN_POINT('Ctrl Pts',(95.0206627203807,-0.267965536220054,
-4.395966111227));
#34932=CARTESIAN_POINT('Ctrl Pts',(95.0318185957106,-0.322206153522478,
-4.39296430514338));
#34933=CARTESIAN_POINT('Ctrl Pts',(95.0460199308673,-0.375675759865854,
-4.38996249905976));
#34934=CARTESIAN_POINT('Ctrl Pts',(95.0602128253395,-0.429113586093144,
-4.38696247712516));
#34935=CARTESIAN_POINT('Ctrl Pts',(95.0774474566162,-0.481780800255754,
-4.38396245519056));
#34936=CARTESIAN_POINT('Ctrl Pts',(95.0976125795179,-0.53331234365282,-4.38096243325596));
#34937=CARTESIAN_POINT('Ctrl Pts',(95.1177736813723,-0.584833611348646,
-4.37796300954387));
#34938=CARTESIAN_POINT('Ctrl Pts',(95.140863922,-0.635219166491393,-4.37496358583178));
#34939=CARTESIAN_POINT('Ctrl Pts',(95.1667233416066,-0.684122431892717,
-4.37196416211969));
#34940=CARTESIAN_POINT('Ctrl Pts',(95.1926065352042,-0.733070656763449,
-4.36896198087193));
#34941=CARTESIAN_POINT('Ctrl Pts',(95.2212637466744,-0.780533401427555,
-4.36595979962417));
#34942=CARTESIAN_POINT('Ctrl Pts',(95.2524889885297,-0.826188641924519,
-4.36295761837641));
#34943=CARTESIAN_POINT('Ctrl Pts',(95.2837284434219,-0.871864663673477,
-4.35995407060239));
#34944=CARTESIAN_POINT('Ctrl Pts',(95.3175379358857,-0.915731122166067,
-4.35695052282837));
#34945=CARTESIAN_POINT('Ctrl Pts',(95.3536700046144,-0.957497666895822,
-4.35394697505435));
#34946=CARTESIAN_POINT('Ctrl Pts',(95.389870266542,-0.999343038949732,-4.35093775858938));
#34947=CARTESIAN_POINT('Ctrl Pts',(95.4284014928612,-1.03908019999244,-4.34792854212442));
#34948=CARTESIAN_POINT('Ctrl Pts',(95.4689788706773,-1.07645523712673,-4.34491932565945));
#34949=CARTESIAN_POINT('Ctrl Pts',(95.5000222276987,-1.10504867228423,-4.34261715173634));
#34950=CARTESIAN_POINT('Ctrl Pts',(95.5322623840527,-1.13226033165432,-4.34031497781323));
#34951=CARTESIAN_POINT('Ctrl Pts',(95.5655599184972,-1.15799334977846,-4.33801280389012));
#34952=CARTESIAN_POINT('Ctrl Pts',(95.6090969691839,-1.1916396762432,-4.33500267522888));
#34953=CARTESIAN_POINT('Ctrl Pts',(95.6546256344026,-1.22289799115637,-4.33199254656764));
#34954=CARTESIAN_POINT('Ctrl Pts',(95.7018536337863,-1.25152580705963,-4.3289824179064));
#34955=CARTESIAN_POINT('Ctrl Pts',(95.7489976957078,-1.28010274326757,-4.32597763909196));
#34956=CARTESIAN_POINT('Ctrl Pts',(95.7978346502252,-1.30605818676549,-4.32297286027752));
#34957=CARTESIAN_POINT('Ctrl Pts',(95.8480412955106,-1.32919145352617,-4.31996808146307));
#34958=CARTESIAN_POINT('Ctrl Pts',(95.8981982696384,-1.35230183375197,-4.31696627537945));
#34959=CARTESIAN_POINT('Ctrl Pts',(95.9497217728902,-1.37259534829205,-4.31396446929583));
#34960=CARTESIAN_POINT('Ctrl Pts',(96.0022635610076,-1.38991693090367,-4.31096266321221));
#34961=CARTESIAN_POINT('Ctrl Pts',(96.0547741204656,-1.40722821828508,-4.30796264127761));
#34962=CARTESIAN_POINT('Ctrl Pts',(96.1083012646293,-1.42157090982359,-4.30496261934302));
#34963=CARTESIAN_POINT('Ctrl Pts',(96.1624784630826,-1.43283870970991,-4.30196259740842));
#34964=CARTESIAN_POINT('Ctrl Pts',(96.216644858275,-1.44410426272882,-4.29896317369633));
#34965=CARTESIAN_POINT('Ctrl Pts',(96.271460533566,-1.45229603431268,-4.29596374998423));
#34966=CARTESIAN_POINT('Ctrl Pts',(96.3265478198291,-1.45735862667908,-4.29296432627214));
#34967=CARTESIAN_POINT('Ctrl Pts',(96.3816857508732,-1.4624258733659,-4.28996214502438));
#34968=CARTESIAN_POINT('Ctrl Pts',(96.4370952647414,-1.4643581448739,-4.28695996377662));
#34969=CARTESIAN_POINT('Ctrl Pts',(96.4923941069457,-1.46315200863983,-4.28395778252887));
#34970=CARTESIAN_POINT('Ctrl Pts',(96.5477181199555,-1.46194532339932,-4.28095423475485));
#34971=CARTESIAN_POINT('Ctrl Pts',(96.6029308334775,-1.4575974242657,-4.27795068698083));
#34972=CARTESIAN_POINT('Ctrl Pts',(96.6576538592619,-1.45015692036635,-4.27494713920681));
#34973=CARTESIAN_POINT('Ctrl Pts',(96.7124801655479,-1.44270237376806,-4.27193792274184));
#34974=CARTESIAN_POINT('Ctrl Pts',(96.766814418167,-1.43214366353828,-4.26892870627687));
#34975=CARTESIAN_POINT('Ctrl Pts',(96.8202883375866,-1.41858059113104,-4.26591948981191));
#34976=CARTESIAN_POINT('Ctrl Pts',(96.8611980774767,-1.40820428488095,-4.26361731588879));
#34977=CARTESIAN_POINT('Ctrl Pts',(96.9016044694145,-1.39607063011443,-4.26131514196567));
#34978=CARTESIAN_POINT('Ctrl Pts',(96.9413502067518,-1.38224346896779,-4.25901296804255));
#34979=CARTESIAN_POINT('Ctrl Pts',(96.9933183842731,-1.36416423800567,-4.25600283938132));
#34980=CARTESIAN_POINT('Ctrl Pts',(97.0443747482134,-1.34311217613538,-4.25299271072008));
#34981=CARTESIAN_POINT('Ctrl Pts',(97.0941565079554,-1.31919958183506,-4.24998258205884));
#34982=CARTESIAN_POINT('Ctrl Pts',(97.1438497914834,-1.29532948695265,-4.2469778032444));
#34983=CARTESIAN_POINT('Ctrl Pts',(97.1922724941834,-1.26860917563466,-4.24397302442995));
#34984=CARTESIAN_POINT('Ctrl Pts',(97.2390799415717,-1.23919968514556,-4.24096824561551));
#34985=CARTESIAN_POINT('Ctrl Pts',(97.2858410807456,-1.20981929047493,-4.23796643953189));
#34986=CARTESIAN_POINT('Ctrl Pts',(97.3309896852464,-1.17775526653294,-4.23496463344827));
#34987=CARTESIAN_POINT('Ctrl Pts',(97.3742056036268,-1.14321454967189,-4.23196282736466));
#34988=CARTESIAN_POINT('Ctrl Pts',(97.4173958362581,-1.10869436238017,-4.22896280543006));
#34989=CARTESIAN_POINT('Ctrl Pts',(97.4586552478697,-1.07170072892314,-4.22596278349546));
#34990=CARTESIAN_POINT('Ctrl Pts',(97.4976945420802,-1.0324825487758,-4.22296276156086));
#34991=CARTESIAN_POINT('Ctrl Pts',(97.5367260516195,-0.993272188970639,
-4.21996333784877));
#34992=CARTESIAN_POINT('Ctrl Pts',(97.5735379505794,-0.951838537499286,
-4.21696391413667));
#34993=CARTESIAN_POINT('Ctrl Pts',(97.6078774848983,-0.908467633288419,
-4.21396449042458));
#34994=CARTESIAN_POINT('Ctrl Pts',(97.6422485894453,-0.865056855812966,
-4.21096230917682));
#34995=CARTESIAN_POINT('Ctrl Pts',(97.6741424596976,-0.819705682282122,
-4.20796012792906));
#34996=CARTESIAN_POINT('Ctrl Pts',(97.7033473584394,-0.77273238557824,-4.20495794668131));
#34997=CARTESIAN_POINT('Ctrl Pts',(97.7325655506029,-0.725737707672449,
-4.20195439890729));
#34998=CARTESIAN_POINT('Ctrl Pts',(97.7590920779884,-0.677119899143029,
-4.19895085113327));
#34999=CARTESIAN_POINT('Ctrl Pts',(97.7827609021939,-0.627222430169181,
-4.19594730335925));
#35000=CARTESIAN_POINT('Ctrl Pts',(97.8064743973219,-0.577230788120041,
-4.19293808689429));
#35001=CARTESIAN_POINT('Ctrl Pts',(97.8273192156744,-0.525955151437095,
-4.18992887042932));
#35002=CARTESIAN_POINT('Ctrl Pts',(97.8451777171641,-0.473758495262967,
-4.18691965396436));
#35003=CARTESIAN_POINT('Ctrl Pts',(97.8588402027029,-0.433825914101916,
-4.18461748004123));
#35004=CARTESIAN_POINT('Ctrl Pts',(97.8707558342186,-0.393354692066864,
-4.18231530611811));
#35005=CARTESIAN_POINT('Ctrl Pts',(97.8808921294835,-0.352511460801676,
-4.18001313219499));
#35006=CARTESIAN_POINT('Ctrl Pts',(97.8981315172016,-0.283046998585734,
-4.17609769092005));
#35007=CARTESIAN_POINT('Ctrl Pts',(97.9102820849996,-0.212273263424402,
-4.17218224964512));
#35008=CARTESIAN_POINT('Ctrl Pts',(97.917188724932,-0.140835745534943,-4.16826680837019));
#35009=CARTESIAN_POINT('Ctrl Pts',(97.9216643126592,-0.094543354233742,
-4.16572955420779));
#35010=CARTESIAN_POINT('Ctrl Pts',(97.9239387713273,-0.0479725928676012,
-4.1631923000454));
#35011=CARTESIAN_POINT('Ctrl Pts',(97.9239803682192,-0.00130446693377829,
-4.16065504588301));
#35012=CARTESIAN_POINT('Ctrl Pts',(97.9239803685999,-0.00130403978581689,
-4.08934495418713));
#35013=CARTESIAN_POINT('Ctrl Pts',(97.9239152216095,-0.0744172864775993,
-4.0933212267369));
#35014=CARTESIAN_POINT('Ctrl Pts',(97.9183674533638,-0.147291162013056,
-4.09729749928667));
#35015=CARTESIAN_POINT('Ctrl Pts',(97.9074660957169,-0.219240135127319,
-4.10127377183644));
#35016=CARTESIAN_POINT('Ctrl Pts',(97.9013270157352,-0.25975807012678,-4.10351300258204));
#35017=CARTESIAN_POINT('Ctrl Pts',(97.8934909747883,-0.299983198187053,
-4.10575223332764));
#35018=CARTESIAN_POINT('Ctrl Pts',(97.8839874350564,-0.339796315162533,
-4.10799146407324));
#35019=CARTESIAN_POINT('Ctrl Pts',(97.8712121204148,-0.393315857414546,
-4.11100159273448));
#35020=CARTESIAN_POINT('Ctrl Pts',(97.8553875073782,-0.446226378391438,
-4.11401172139571));
#35021=CARTESIAN_POINT('Ctrl Pts',(97.8365889378747,-0.498155652927126,
-4.11702185005695));
#35022=CARTESIAN_POINT('Ctrl Pts',(97.8178237787261,-0.54999263450987,-4.12002662887139));
#35023=CARTESIAN_POINT('Ctrl Pts',(97.7960953306467,-0.600851337971159,
-4.12303140768584));
#35024=CARTESIAN_POINT('Ctrl Pts',(97.7715292457042,-0.650372674104551,
-4.12603618650028));
#35025=CARTESIAN_POINT('Ctrl Pts',(97.7469874648329,-0.699845017080199,
-4.1290379925839));
#35026=CARTESIAN_POINT('Ctrl Pts',(97.7196138419051,-0.747982142955423,
-4.13203979866751));
#35027=CARTESIAN_POINT('Ctrl Pts',(97.6895821564042,-0.79444475791324,-4.13504160475113));
#35028=CARTESIAN_POINT('Ctrl Pts',(97.6595683204915,-0.840879757419996,
-4.13804162668572));
#35029=CARTESIAN_POINT('Ctrl Pts',(97.6268998394661,-0.885641776033794,
-4.14104164862032));
#35030=CARTESIAN_POINT('Ctrl Pts',(97.5917953392551,-0.928418010223474,
-4.14404167055491));
#35031=CARTESIAN_POINT('Ctrl Pts',(97.5566978390935,-0.971185714573505,
-4.147041094267));
#35032=CARTESIAN_POINT('Ctrl Pts',(97.5191656192783,-1.01196801287829,-4.15004051797909));
#35033=CARTESIAN_POINT('Ctrl Pts',(97.4794579233039,-1.05048473430816,-4.15303994169118));
#35034=CARTESIAN_POINT('Ctrl Pts',(97.4397137218542,-1.08903686628464,-4.15604212293894));
#35035=CARTESIAN_POINT('Ctrl Pts',(97.3977904283256,-1.1253188915866,-4.15904430418669));
#35036=CARTESIAN_POINT('Ctrl Pts',(97.3539834718479,-1.15908821609728,-4.16204648543445));
#35037=CARTESIAN_POINT('Ctrl Pts',(97.310156575416,-1.19287291165484,-4.16505003320847));
#35038=CARTESIAN_POINT('Ctrl Pts',(97.2644447435136,-1.2241423277905,-4.16805358098248));
#35039=CARTESIAN_POINT('Ctrl Pts',(97.2171730593664,-1.25269681127658,-4.1710571287565));
#35040=CARTESIAN_POINT('Ctrl Pts',(97.1698121578708,-1.28130518654472,-4.17406634522146));
#35041=CARTESIAN_POINT('Ctrl Pts',(97.1208859910793,-1.3071881456583,-4.17707556168643));
#35042=CARTESIAN_POINT('Ctrl Pts',(97.0707439034656,-1.33019223314197,-4.18008477815139));
#35043=CARTESIAN_POINT('Ctrl Pts',(97.0323831514559,-1.34779130284898,-4.18238695207452));
#35044=CARTESIAN_POINT('Ctrl Pts',(96.9933112546867,-1.36370635768066,-4.18468912599766));
#35045=CARTESIAN_POINT('Ctrl Pts',(96.9536907462404,-1.37788836502644,-4.18699129992079));
#35046=CARTESIAN_POINT('Ctrl Pts',(96.9018863074669,-1.39643156298229,-4.19000142858203));
#35047=CARTESIAN_POINT('Ctrl Pts',(96.8489258157292,-1.41208812463287,-4.19301155724327));
#35048=CARTESIAN_POINT('Ctrl Pts',(96.7951621861553,-1.42471776850098,-4.19602168590452));
#35049=CARTESIAN_POINT('Ctrl Pts',(96.7414941097001,-1.43732496593328,-4.19902646471897));
#35050=CARTESIAN_POINT('Ctrl Pts',(96.687026238061,-1.44691580181003,-4.20203124353341));
#35051=CARTESIAN_POINT('Ctrl Pts',(96.6321279739089,-1.45339930818685,-4.20503602234786));
#35052=CARTESIAN_POINT('Ctrl Pts',(96.577284022494,-1.45987640020825,-4.20803782843149));
#35053=CARTESIAN_POINT('Ctrl Pts',(96.5220110439524,-1.46325219091205,-4.21103963451512));
#35054=CARTESIAN_POINT('Ctrl Pts',(96.4666881584148,-1.46348683648281,-4.21404144059874));
#35055=CARTESIAN_POINT('Ctrl Pts',(96.4113981545055,-1.46372134258997,-4.21704146253335));
#35056=CARTESIAN_POINT('Ctrl Pts',(96.3560588294504,-1.46081840177854,-4.22004148446795));
#35057=CARTESIAN_POINT('Ctrl Pts',(96.3010516209737,-1.45479020452473,-4.22304150640256));
#35058=CARTESIAN_POINT('Ctrl Pts',(96.2460553812668,-1.44876320932988,-4.22604093011465));
#35059=CARTESIAN_POINT('Ctrl Pts',(96.1913916512949,-1.43961225283038,-4.22904035382675));
#35060=CARTESIAN_POINT('Ctrl Pts',(96.1374367312958,-1.42740137418846,-4.23203977753885));
#35061=CARTESIAN_POINT('Ctrl Pts',(96.0834322075626,-1.41517926941224,-4.23504195878662));
#35062=CARTESIAN_POINT('Ctrl Pts',(96.0301383119069,-1.39989173899873,-4.23804414003438));
#35063=CARTESIAN_POINT('Ctrl Pts',(95.9779196447471,-1.3816536603219,-4.24104632128215));
#35064=CARTESIAN_POINT('Ctrl Pts',(95.9256772088093,-1.36340728007651,-4.24404986905617));
#35065=CARTESIAN_POINT('Ctrl Pts',(95.8745114657393,-1.34220787684331,-4.2470534168302));
#35066=CARTESIAN_POINT('Ctrl Pts',(95.8247672546869,-1.31821862683288,-4.25005696460422));
#35067=CARTESIAN_POINT('Ctrl Pts',(95.7749291598078,-1.29418410115029,-4.25306618106919));
#35068=CARTESIAN_POINT('Ctrl Pts',(95.726518419494,-1.26734946696852,-4.25607539753417));
#35069=CARTESIAN_POINT('Ctrl Pts',(95.6798544372851,-1.23792346221688,-4.25908461399914));
#35070=CARTESIAN_POINT('Ctrl Pts',(95.6441545784552,-1.21541136260953,-4.26138678792221));
#35071=CARTESIAN_POINT('Ctrl Pts',(95.6094765607002,-1.19138352101,-4.26368896184529));
#35072=CARTESIAN_POINT('Ctrl Pts',(95.5759502575892,-1.1659492720233,-4.26599113576837));
#35073=CARTESIAN_POINT('Ctrl Pts',(95.5321140882677,-1.13269359091056,-4.2690012644296));
#35074=CARTESIAN_POINT('Ctrl Pts',(95.4900638917384,-1.0968924375822,-4.27201139309084));
#35075=CARTESIAN_POINT('Ctrl Pts',(95.4501099889542,-1.05876473870739,-4.27502152175207));
#35076=CARTESIAN_POINT('Ctrl Pts',(95.410227095513,-1.0207048034967,-4.27802630056651));
#35077=CARTESIAN_POINT('Ctrl Pts',(95.3724334811049,-0.98032689018171,-4.28103107938095));
#35078=CARTESIAN_POINT('Ctrl Pts',(95.3370071740009,-0.937890678913456,
-4.2840358581954));
#35079=CARTESIAN_POINT('Ctrl Pts',(95.3016159153585,-0.895496451245696,
-4.28703766427901));
#35080=CARTESIAN_POINT('Ctrl Pts',(95.2685876612969,-0.851048362947523,
-4.29003947036263));
#35081=CARTESIAN_POINT('Ctrl Pts',(95.2381629318349,-0.80484216682723,-4.29304127644625));
#35082=CARTESIAN_POINT('Ctrl Pts',(95.2077562855701,-0.75866343375327,-4.29604129838084));
#35083=CARTESIAN_POINT('Ctrl Pts',(95.1799503866571,-0.710729104212465,
-4.29904132031544));
#35084=CARTESIAN_POINT('Ctrl Pts',(95.1549434413191,-0.661365303392652,
-4.30204134225003));
#35085=CARTESIAN_POINT('Ctrl Pts',(95.1299414825171,-0.612011346013121,
-4.30504076596212));
#35086=CARTESIAN_POINT('Ctrl Pts',(95.1077376073965,-0.561228954292048,
-4.30804018967421));
#35087=CARTESIAN_POINT('Ctrl Pts',(95.0884837904084,-0.509368280552822,
-4.3110396133863));
#35088=CARTESIAN_POINT('Ctrl Pts',(95.0692122723243,-0.457459928435557,
-4.31404179463405));
#35089=CARTESIAN_POINT('Ctrl Pts',(95.0528964151029,-0.404471809923728,
-4.31704397588181));
#35090=CARTESIAN_POINT('Ctrl Pts',(95.0396392220891,-0.35077205622647,-4.32004615712956));
#35091=CARTESIAN_POINT('Ctrl Pts',(95.0263759946955,-0.297047859593382,
-4.32304970490358));
#35092=CARTESIAN_POINT('Ctrl Pts',(95.0161743042849,-0.242611902045981,
-4.3260532526776));
#35093=CARTESIAN_POINT('Ctrl Pts',(95.0090859051473,-0.187842154493746,
-4.32905680045161));
#35094=CARTESIAN_POINT('Ctrl Pts',(95.0019841278492,-0.132969038260377,
-4.33206601691658));
#35095=CARTESIAN_POINT('Ctrl Pts',(94.9980074177096,-0.0777614015979497,
-4.33507523338154));
#35096=CARTESIAN_POINT('Ctrl Pts',(94.997155471935,-0.022600807152141,-4.3380844498465));
#35097=CARTESIAN_POINT('Ctrl Pts',(94.996503698502,0.0195993082588217,-4.34038662376964));
#35098=CARTESIAN_POINT('Ctrl Pts',(94.9976797297326,0.061771799743154,-4.34268879769278));
#35099=CARTESIAN_POINT('Ctrl Pts',(95.0006629573609,0.10374815469235,-4.34499097161592));
#35100=CARTESIAN_POINT('Ctrl Pts',(95.0045635744675,0.158632899870289,-4.34800110027716));
#35101=CARTESIAN_POINT('Ctrl Pts',(95.0115719415834,0.213412680795123,-4.35101122893839));
#35102=CARTESIAN_POINT('Ctrl Pts',(95.0216742598818,0.267707974644417,-4.35402135759963));
#35103=CARTESIAN_POINT('Ctrl Pts',(95.031758623514,0.321906770457785,-4.35702613641407));
#35104=CARTESIAN_POINT('Ctrl Pts',(95.0449259300541,0.375622272989015,-4.36003091522852));
#35105=CARTESIAN_POINT('Ctrl Pts',(95.0611106039428,0.428479737863484,-4.36303569404296));
#35106=CARTESIAN_POINT('Ctrl Pts',(95.077279265778,0.481284909033545,-4.36603750012658));
#35107=CARTESIAN_POINT('Ctrl Pts',(95.0964592275933,0.533233221657604,-4.3690393062102));
#35108=CARTESIAN_POINT('Ctrl Pts',(95.1185342076463,0.583961635573341,-4.37204111229382));
#35109=CARTESIAN_POINT('Ctrl Pts',(95.1405960672468,0.634659898624063,-4.37504113422842));
#35110=CARTESIAN_POINT('Ctrl Pts',(95.16554932428,0.684139216791593,-4.37804115616302));
#35111=CARTESIAN_POINT('Ctrl Pts',(95.1932291392264,0.732055393507343,-4.38104117809761));
#35112=CARTESIAN_POINT('Ctrl Pts',(95.2209034346504,0.779962015447825,-4.3840406018097));
#35113=CARTESIAN_POINT('Ctrl Pts',(95.2513029442182,0.826305657917133,-4.38704002552179));
#35114=CARTESIAN_POINT('Ctrl Pts',(95.2842174441787,0.870767716367634,-4.39003944923389));
#35115=CARTESIAN_POINT('Ctrl Pts',(95.3171622042546,0.915270651241015,-4.39304163048164));
#35116=CARTESIAN_POINT('Ctrl Pts',(95.3526262592382,0.957888120715592,-4.3960438117294));
#35117=CARTESIAN_POINT('Ctrl Pts',(95.3903575699578,0.998332711270284,-4.39904599297716));
#35118=CARTESIAN_POINT('Ctrl Pts',(95.4281060551324,1.03879571130479,-4.40204954075118));
#35119=CARTESIAN_POINT('Ctrl Pts',(95.4681234710175,1.07708349509045,-4.4050530885252));
#35120=CARTESIAN_POINT('Ctrl Pts',(95.5101215351449,1.11294619519553,-4.40805663629922));
#35121=CARTESIAN_POINT('Ctrl Pts',(95.5521988635503,1.1488765801116,-4.41106585276419));
#35122=CARTESIAN_POINT('Ctrl Pts',(95.5962638862456,1.18237241782698,-4.41407506922915));
#35123=CARTESIAN_POINT('Ctrl Pts',(95.6419968688008,1.21322547760752,-4.41708428569412));
#35124=CARTESIAN_POINT('Ctrl Pts',(95.6769844747412,1.23682933279781,-4.41938645961724));
#35125=CARTESIAN_POINT('Ctrl Pts',(95.7129476501924,1.25888725878573,-4.42168863354036));
#35126=CARTESIAN_POINT('Ctrl Pts',(95.7497340010342,1.27932444092072,-4.42399080746349));
#35127=CARTESIAN_POINT('Ctrl Pts',(95.7978327341053,1.30604637842581,-4.42700093612473));
#35128=CARTESIAN_POINT('Ctrl Pts',(95.8475416191947,1.33010813960356,-4.43001106478597));
#35129=CARTESIAN_POINT('Ctrl Pts',(95.8985352560998,1.35131391156252,-4.43302119344721));
#35130=CARTESIAN_POINT('Ctrl Pts',(95.9494382629437,1.37248199488957,-4.43602597226165));
#35131=CARTESIAN_POINT('Ctrl Pts',(96.0016210065593,1.39080396100805,-4.43903075107609));
#35132=CARTESIAN_POINT('Ctrl Pts',(96.0547337982194,1.40612997235859,-4.44203552989054));
#35133=CARTESIAN_POINT('Ctrl Pts',(96.1077940435715,1.42144082116003,-4.44503733597416));
#35134=CARTESIAN_POINT('Ctrl Pts',(96.1617820093186,1.43376144103936,-4.44803914205778));
#35135=CARTESIAN_POINT('Ctrl Pts',(96.2163301036668,1.44299085736582,-4.4510409481414));
#35136=CARTESIAN_POINT('Ctrl Pts',(96.2708457768904,1.45221478811005,-4.454040970076));
#35137=CARTESIAN_POINT('Ctrl Pts',(96.3259203991757,1.45835106898929,-4.4570409920106));
#35138=CARTESIAN_POINT('Ctrl Pts',(96.3811756289667,1.4613496898836,-4.4600410139452));
#35139=CARTESIAN_POINT('Ctrl Pts',(96.4364198405309,1.46434771283477,-4.4630404376573));
#35140=CARTESIAN_POINT('Ctrl Pts',(96.4918440610336,1.46420928974961,-4.46603986136939));
#35141=CARTESIAN_POINT('Ctrl Pts',(96.5470665851594,1.46093640440328,-4.46903928508148));
#35142=CARTESIAN_POINT('Ctrl Pts',(96.6023398783976,1.45766051011292,-4.47204146632924));
#35143=CARTESIAN_POINT('Ctrl Pts',(96.6574105764688,1.4512444276434,-4.475043647577));
#35144=CARTESIAN_POINT('Ctrl Pts',(96.7119002495997,1.44174220496457,-4.47804582882476));
#35145=CARTESIAN_POINT('Ctrl Pts',(96.7664147252203,1.43223565708491,-4.48104937659878));
#35146=CARTESIAN_POINT('Ctrl Pts',(96.8203471335242,1.41964028905232,-4.4840529243728));
#35147=CARTESIAN_POINT('Ctrl Pts',(96.8733306874039,1.40406101860863,-4.48705647214682));
#35148=CARTESIAN_POINT('Ctrl Pts',(96.9264142388247,1.38845234491386,-4.49006568861178));
#35149=CARTESIAN_POINT('Ctrl Pts',(96.9785448598012,1.36984869672328,-4.49307490507675));
#35150=CARTESIAN_POINT('Ctrl Pts',(97.029373449852,1.34840408377119,-4.49608412154172));
#35151=CARTESIAN_POINT('Ctrl Pts',(97.0682594043608,1.33199807599333,-4.49838629546483));
#35152=CARTESIAN_POINT('Ctrl Pts',(97.1063836489081,1.3139303128472,-4.50068846938794));
#35153=CARTESIAN_POINT('Ctrl Pts',(97.1436002566615,1.29428755007857,-4.50299064331105));
#35154=CARTESIAN_POINT('Ctrl Pts',(97.1922615574208,1.26860432840617,-4.50600077197229));
#35155=CARTESIAN_POINT('Ctrl Pts',(97.2395746696548,1.24011905118202,-4.50901090063353));
#35156=CARTESIAN_POINT('Ctrl Pts',(97.2851977974036,1.20899725843814,-4.51202102929476));
#35157=CARTESIAN_POINT('Ctrl Pts',(97.3307398399993,1.17793077788913,-4.51502580810921));
#35158=CARTESIAN_POINT('Ctrl Pts',(97.3745974259837,1.14423737608224,-4.51803058692365));
#35159=CARTESIAN_POINT('Ctrl Pts',(97.4164539938206,1.10812805608364,-4.5210353657381));
#35160=CARTESIAN_POINT('Ctrl Pts',(97.458269151518,1.07205446027483,-4.52403717182171));
#35161=CARTESIAN_POINT('Ctrl Pts',(97.4980868147994,1.03357002432292,-4.52703897790533));
#35162=CARTESIAN_POINT('Ctrl Pts',(97.5356215639806,0.992927444106501,-4.53004078398895));
#35163=CARTESIAN_POINT('Ctrl Pts',(97.5731340040638,0.952309020153915,-4.53304080592355));
#35164=CARTESIAN_POINT('Ctrl Pts',(97.6083658618605,0.909535381553906,-4.53604082785815));
#35165=CARTESIAN_POINT('Ctrl Pts',(97.6410685282083,0.864896074208625,-4.53904084979275));
#35166=CARTESIAN_POINT('Ctrl Pts',(97.6737646734467,0.820265668211052,-4.54204027350484));
#35167=CARTESIAN_POINT('Ctrl Pts',(97.7039323168962,0.773770758081098,-4.54503969721693));
#35168=CARTESIAN_POINT('Ctrl Pts',(97.7313645577357,0.725732116220329,-4.54803912092901));
#35169=CARTESIAN_POINT('Ctrl Pts',(97.7588220185473,0.677649309786266,-4.55104130217677));
#35170=CARTESIAN_POINT('Ctrl Pts',(97.7835387900433,0.628020395763152,-4.55404348342453));
#35171=CARTESIAN_POINT('Ctrl Pts',(97.8053533663104,0.577191850869178,-4.55704566467229));
#35172=CARTESIAN_POINT('Ctrl Pts',(97.8271778720883,0.526340169949871,-4.56004921244631));
#35173=CARTESIAN_POINT('Ctrl Pts',(97.8460973685622,0.474288266867315,-4.56305276022033));
#35174=CARTESIAN_POINT('Ctrl Pts',(97.8619993161285,0.421400662337796,-4.56605630799434));
#35175=CARTESIAN_POINT('Ctrl Pts',(97.8779312759447,0.368413241355353,-4.56906552445931));
#35176=CARTESIAN_POINT('Ctrl Pts',(97.8908341865632,0.314587482958828,-4.57207474092428));
#35177=CARTESIAN_POINT('Ctrl Pts',(97.9006462881487,0.260299918510812,-4.57508395738924));
#35178=CARTESIAN_POINT('Ctrl Pts',(97.9081529479932,0.218767706828071,-4.57738613131237));
#35179=CARTESIAN_POINT('Ctrl Pts',(97.9138516476614,0.176965471128063,-4.57968830523549));
#35180=CARTESIAN_POINT('Ctrl Pts',(97.9177353135767,0.135062832059178,-4.58199047915861));
#35181=CARTESIAN_POINT('Ctrl Pts',(97.9218708719417,0.0904424107107279,
-4.58444197082477));
#35182=CARTESIAN_POINT('Ctrl Pts',(97.9239574360407,0.0456291932873014,
-4.58689346249092));
#35183=CARTESIAN_POINT('Ctrl Pts',(97.9239807519794,0.000760505223226176,
-4.58934495415707));
#35184=CARTESIAN_POINT('Origin',(96.460480949577,-8.32667268468867E-16,
1.18130019239114E-14));
#35185=CARTESIAN_POINT('',(97.9239808052395,0.000649981535139221,-5.16065504581337));
#35186=CARTESIAN_POINT('',(97.9239808315836,0.000587678971723037,-5.08934495412971));
#35187=CARTESIAN_POINT('',(97.923980949577,-1.01189432752408E-15,1.19922289829666E-14));
#35188=CARTESIAN_POINT('Ctrl Pts',(97.9239808052395,0.000649981535147704,
-5.16065504581337));
#35189=CARTESIAN_POINT('Ctrl Pts',(97.9239538366058,0.0613726164339911,
-5.15736868599221));
#35190=CARTESIAN_POINT('Ctrl Pts',(97.9201434793188,0.12197259959902,-5.15408232617104));
#35191=CARTESIAN_POINT('Ctrl Pts',(97.9126202744233,0.181998986906557,-5.15079596634988));
#35192=CARTESIAN_POINT('Ctrl Pts',(97.9050714331658,0.242229922436747,-5.14749840780278));
#35193=CARTESIAN_POINT('Ctrl Pts',(97.8937845435227,0.301883015490773,-5.14420084925568));
#35194=CARTESIAN_POINT('Ctrl Pts',(97.8788808603027,0.36051899152915,-5.14090329070857));
#35195=CARTESIAN_POINT('Ctrl Pts',(97.8639101969523,0.419418489360427,-5.13759091227445));
#35196=CARTESIAN_POINT('Ctrl Pts',(97.8452903207953,0.477291389051983,-5.13427853384032));
#35197=CARTESIAN_POINT('Ctrl Pts',(97.8231921632558,0.533713779205726,-5.13096615540619));
#35198=CARTESIAN_POINT('Ctrl Pts',(97.8166208628006,0.550492032208917,-5.12998115772604));
#35199=CARTESIAN_POINT('Ctrl Pts',(97.8097422965267,0.567142179412155,-5.12899616004589));
#35200=CARTESIAN_POINT('Ctrl Pts',(97.8025617387441,0.58365349767525,-5.12801116236573));
#35201=CARTESIAN_POINT('Ctrl Pts',(97.7806181309362,0.63411167980101,-5.12500103370449));
#35202=CARTESIAN_POINT('Ctrl Pts',(97.7557788480465,0.68343663933808,-5.12199090504325));
#35203=CARTESIAN_POINT('Ctrl Pts',(97.7281832053769,0.731275078639955,-5.11898077638201));
#35204=CARTESIAN_POINT('Ctrl Pts',(97.7006366079399,0.779028495555788,-5.11597599756757));
#35205=CARTESIAN_POINT('Ctrl Pts',(97.6703436342324,0.8253001814735,-5.11297121875312));
#35206=CARTESIAN_POINT('Ctrl Pts',(97.6374908347472,0.869758575819526,-5.10996643993868));
#35207=CARTESIAN_POINT('Ctrl Pts',(97.6046705376642,0.914172985949913,-5.10696463385506));
#35208=CARTESIAN_POINT('Ctrl Pts',(97.5692957439274,0.956777235594788,-5.10396282777143));
#35209=CARTESIAN_POINT('Ctrl Pts',(97.5315969248381,0.997267675972961,-5.10096102168781));
#35210=CARTESIAN_POINT('Ctrl Pts',(97.493920512363,1.03773405051294,-5.09796099975321));
#35211=CARTESIAN_POINT('Ctrl Pts',(97.4539231715251,1.07608872022588,-5.09496097781861));
#35212=CARTESIAN_POINT('Ctrl Pts',(97.4118748925435,1.11206196557868,-5.09196095588401));
#35213=CARTESIAN_POINT('Ctrl Pts',(97.3698349982429,1.1480280376489,-5.08896153217192));
#35214=CARTESIAN_POINT('Ctrl Pts',(97.3257453790662,1.18161328530533,-5.08596210845983));
#35215=CARTESIAN_POINT('Ctrl Pts',(97.279910305661,1.21258722588844,-5.08296268474774));
#35216=CARTESIAN_POINT('Ctrl Pts',(97.2340330935445,1.24358964252365,-5.07996050349998));
#35217=CARTESIAN_POINT('Ctrl Pts',(97.1864076597451,1.2719756594284,-5.07695832225222));
#35218=CARTESIAN_POINT('Ctrl Pts',(97.1373673266349,1.2975581229962,-5.07395614100446));
#35219=CARTESIAN_POINT('Ctrl Pts',(97.0883046714537,1.32315223113354,-5.07095259323044));
#35220=CARTESIAN_POINT('Ctrl Pts',(97.0378263153113,1.34594002441208,-5.06794904545642));
#35221=CARTESIAN_POINT('Ctrl Pts',(96.986287262866,1.36578181672822,-5.0649454976824));
#35222=CARTESIAN_POINT('Ctrl Pts',(96.9346509391329,1.38566105708812,-5.06193628121743));
#35223=CARTESIAN_POINT('Ctrl Pts',(96.8819504240829,1.40258302750709,-5.05892706475246));
#35224=CARTESIAN_POINT('Ctrl Pts',(96.8285565251034,1.41645777229713,-5.05591784828749));
#35225=CARTESIAN_POINT('Ctrl Pts',(96.7877080041297,1.42707252069334,-5.05361567436439));
#35226=CARTESIAN_POINT('Ctrl Pts',(96.7464539979934,1.4359047947553,-5.05131350044128));
#35227=CARTESIAN_POINT('Ctrl Pts',(96.7049631121538,1.44293476019595,-5.04901132651818));
#35228=CARTESIAN_POINT('Ctrl Pts',(96.6507131254815,1.45212655072403,-5.04600119785694));
#35229=CARTESIAN_POINT('Ctrl Pts',(96.5958300577282,1.45827394706614,-5.04299106919571));
#35230=CARTESIAN_POINT('Ctrl Pts',(96.5406859265152,1.46130058908985,-5.03998094053447));
#35231=CARTESIAN_POINT('Ctrl Pts',(96.4856398019612,1.46432185191787,-5.03697616172003));
#35232=CARTESIAN_POINT('Ctrl Pts',(96.4303340577829,1.46423333870561,-5.03397138290559));
#35233=CARTESIAN_POINT('Ctrl Pts',(96.3751483153409,1.46101012711559,-5.03096660409114));
#35234=CARTESIAN_POINT('Ctrl Pts',(96.3200171700481,1.45779010435944,-5.02796479800752));
#35235=CARTESIAN_POINT('Ctrl Pts',(96.265006315935,1.45144155732336,-5.0249629919239));
#35236=CARTESIAN_POINT('Ctrl Pts',(96.2104959956422,1.44199159942289,-5.02196118584028));
#35237=CARTESIAN_POINT('Ctrl Pts',(96.1560180740227,1.43254725818542,-5.01896116390569));
#35238=CARTESIAN_POINT('Ctrl Pts',(96.1020406158815,1.42000524975325,-5.01596114197109));
#35239=CARTESIAN_POINT('Ctrl Pts',(96.0489370401826,1.40444432450716,-5.01296112003649));
#35240=CARTESIAN_POINT('Ctrl Pts',(95.9958440536577,1.38888650220364,-5.0099616963244));
#35241=CARTESIAN_POINT('Ctrl Pts',(95.9436251100285,1.3703111070388,-5.00696227261231));
#35242=CARTESIAN_POINT('Ctrl Pts',(95.8926394970126,1.34884703904837,-5.00396284890022));
#35243=CARTESIAN_POINT('Ctrl Pts',(95.8416070101103,1.32736323795627,-5.00096066765246));
#35244=CARTESIAN_POINT('Ctrl Pts',(95.7918106069325,1.30298566361317,-4.9979584864047));
#35245=CARTESIAN_POINT('Ctrl Pts',(95.7435891596973,1.27589122248059,-4.99495630515695));
#35246=CARTESIAN_POINT('Ctrl Pts',(95.6953457631296,1.24878444855984,-4.99195275738293));
#35247=CARTESIAN_POINT('Ctrl Pts',(95.6486791973347,1.2189586275611,-4.98894920960891));
#35248=CARTESIAN_POINT('Ctrl Pts',(95.6039004263353,1.1866347615012,-4.98594566183489));
#35249=CARTESIAN_POINT('Ctrl Pts',(95.5590371429416,1.15424988958401,-4.98293644536992));
#35250=CARTESIAN_POINT('Ctrl Pts',(95.5160691827544,1.11935788811184,-4.97992722890496));
#35251=CARTESIAN_POINT('Ctrl Pts',(95.475274493784,1.08222016681624,-4.97691801243999));
#35252=CARTESIAN_POINT('Ctrl Pts',(95.4440648848233,1.05380828800113,-4.97461583851687));
#35253=CARTESIAN_POINT('Ctrl Pts',(95.4141265905881,1.02408286747061,-4.97231366459374));
#35254=CARTESIAN_POINT('Ctrl Pts',(95.3855683481887,0.993174279457893,-4.97001149067062));
#35255=CARTESIAN_POINT('Ctrl Pts',(95.3482279964901,0.952760813854431,-4.96700136200938));
#35256=CARTESIAN_POINT('Ctrl Pts',(95.3130914938384,0.910153680775445,-4.96399123334814));
#35257=CARTESIAN_POINT('Ctrl Pts',(95.2804260628675,0.865622732114266,-4.96098110468691));
#35258=CARTESIAN_POINT('Ctrl Pts',(95.2478186875715,0.821170927496311,-4.95797632587246));
#35259=CARTESIAN_POINT('Ctrl Pts',(95.2176739782589,0.774802515035211,-4.95497154705802));
#35260=CARTESIAN_POINT('Ctrl Pts',(95.1902202316792,0.7268218203698,-4.95196676824358));
#35261=CARTESIAN_POINT('Ctrl Pts',(95.1627936460333,0.678888594652632,-4.94896496215996));
#35262=CARTESIAN_POINT('Ctrl Pts',(95.1380530102981,0.629346702650633,-4.94596315607634));
#35263=CARTESIAN_POINT('Ctrl Pts',(95.1161833793443,0.578529422472609,-4.94296134999272));
#35264=CARTESIAN_POINT('Ctrl Pts',(95.094326746792,0.527742345978014,-4.93996132805812));
#35265=CARTESIAN_POINT('Ctrl Pts',(95.0753379451626,0.475681867920573,-4.93696130612352));
#35266=CARTESIAN_POINT('Ctrl Pts',(95.0593550535487,0.422703765631228,-4.93396128418892));
#35267=CARTESIAN_POINT('Ctrl Pts',(95.0433753490199,0.369736227495716,-4.93096186047683));
#35268=CARTESIAN_POINT('Ctrl Pts',(95.0304005165813,0.31585193384279,-4.92796243676475));
#35269=CARTESIAN_POINT('Ctrl Pts',(95.0205189123824,0.261422228279018,-4.92496301305265));
#35270=CARTESIAN_POINT('Ctrl Pts',(95.0106282234796,0.206942482484551,-4.9219608318049));
#35271=CARTESIAN_POINT('Ctrl Pts',(95.0038365388493,0.151916843731529,-4.91895865055714));
#35272=CARTESIAN_POINT('Ctrl Pts',(95.0001808530182,0.0967257876186296,
-4.91595646930938));
#35273=CARTESIAN_POINT('Ctrl Pts',(94.9965235032002,0.0415096097621443,
-4.91295292153536));
#35274=CARTESIAN_POINT('Ctrl Pts',(94.9960050026317,-0.0138716065345326,
-4.90994937376135));
#35275=CARTESIAN_POINT('Ctrl Pts',(94.9986101656971,-0.0690366658989129,
-4.90694582598733));
#35276=CARTESIAN_POINT('Ctrl Pts',(95.0012202455694,-0.124305840028945,
-4.90393660952236));
#35277=CARTESIAN_POINT('Ctrl Pts',(95.006965711078,-0.179357515711698,-4.90092739305739));
#35278=CARTESIAN_POINT('Ctrl Pts',(95.015779494239,-0.233816070756902,-4.89791817659243));
#35279=CARTESIAN_POINT('Ctrl Pts',(95.0225223995745,-0.275479097254243,
-4.89561600266931));
#35280=CARTESIAN_POINT('Ctrl Pts',(95.0310600728233,-0.316795077490998,
-4.89331382874618));
#35281=CARTESIAN_POINT('Ctrl Pts',(95.0413427355865,-0.357601705241623,
-4.89101165482306));
#35282=CARTESIAN_POINT('Ctrl Pts',(95.0547874790901,-0.410957013685889,
-4.88800152616182));
#35283=CARTESIAN_POINT('Ctrl Pts',(95.0712736526104,-0.463665150538443,
-4.88499139750058));
#35284=CARTESIAN_POINT('Ctrl Pts',(95.0907212573221,-0.515354863636512,
-4.88198126883934));
#35285=CARTESIAN_POINT('Ctrl Pts',(95.1101342981606,-0.566952709549832,
-4.8789764900249));
#35286=CARTESIAN_POINT('Ctrl Pts',(95.132498140675,-0.617535233426132,-4.87597171121045));
#35287=CARTESIAN_POINT('Ctrl Pts',(95.1576826444004,-0.666744948259141,
-4.872966932396));
#35288=CARTESIAN_POINT('Ctrl Pts',(95.1828422322318,-0.715905978232068,
-4.86996512631238));
#35289=CARTESIAN_POINT('Ctrl Pts',(95.2108167138578,-0.763696421811132,
-4.86696332022876));
#35290=CARTESIAN_POINT('Ctrl Pts',(95.2414280731478,-0.809779188711201,
-4.86396151414514));
#35291=CARTESIAN_POINT('Ctrl Pts',(95.2720212383156,-0.855834565926139,
-4.86096149221054));
#35292=CARTESIAN_POINT('Ctrl Pts',(95.3052478831216,-0.90018383917649,-4.85796147027594));
#35293=CARTESIAN_POINT('Ctrl Pts',(95.3408854803501,-0.942516968169074,
-4.85496144834134));
#35294=CARTESIAN_POINT('Ctrl Pts',(95.3765159712264,-0.984841655679857,
-4.85196202462925));
#35295=CARTESIAN_POINT('Ctrl Pts',(95.4145561198351,-1.0251505935611,-4.84896260091716));
#35296=CARTESIAN_POINT('Ctrl Pts',(95.4547431933651,-1.06316688047077,-4.84596317720506));
#35297=CARTESIAN_POINT('Ctrl Pts',(95.4949672130886,-1.10121811784998,-4.8429609959573));
#35298=CARTESIAN_POINT('Ctrl Pts',(95.5373417166254,-1.13697212951738,-4.83995881470954));
#35299=CARTESIAN_POINT('Ctrl Pts',(95.5815682590862,-1.17019004118742,-4.83695663346178));
#35300=CARTESIAN_POINT('Ctrl Pts',(95.6258149324874,-1.20342307291347,-4.83395308568776));
#35301=CARTESIAN_POINT('Ctrl Pts',(95.6719148849319,-1.2341174102732,-4.83094953791374));
#35302=CARTESIAN_POINT('Ctrl Pts',(95.7195405576755,-1.26207748797326,-4.82794599013972));
#35303=CARTESIAN_POINT('Ctrl Pts',(95.7672561158614,-1.2900903356145,-4.82493677367475));
#35304=CARTESIAN_POINT('Ctrl Pts',(95.8165026756475,-1.31535837310519,-4.82192755720979));
#35305=CARTESIAN_POINT('Ctrl Pts',(95.8669289976572,-1.33773253319647,-4.81891834074482));
#35306=CARTESIAN_POINT('Ctrl Pts',(95.9055072006282,-1.35484968263162,-4.81661616682171));
#35307=CARTESIAN_POINT('Ctrl Pts',(95.9447753971582,-1.37027404092256,-4.8143139928986));
#35308=CARTESIAN_POINT('Ctrl Pts',(95.9845704526933,-1.38395861533354,-4.81201181897549));
#35309=CARTESIAN_POINT('Ctrl Pts',(96.036603114535,-1.40185141189327,-4.80900169031426));
#35310=CARTESIAN_POINT('Ctrl Pts',(96.0897555781729,-1.41684331694314,-4.80599156165302));
#35311=CARTESIAN_POINT('Ctrl Pts',(96.1436731988852,-1.42879848092781,-4.80298143299179));
#35312=CARTESIAN_POINT('Ctrl Pts',(96.1974949927932,-1.44073239721747,-4.79997665417734));
#35313=CARTESIAN_POINT('Ctrl Pts',(96.2520787336219,-1.44964016971346,-4.7969718753629));
#35314=CARTESIAN_POINT('Ctrl Pts',(96.3070539081435,-1.45543546506087,-4.79396709654846));
#35315=CARTESIAN_POINT('Ctrl Pts',(96.3619746938377,-1.46122502692367,-4.79096529046484));
#35316=CARTESIAN_POINT('Ctrl Pts',(96.4172856234598,-1.46390815645121,-4.78796348438122));
#35317=CARTESIAN_POINT('Ctrl Pts',(96.4726071075089,-1.46344976213528,-4.78496167829761));
#35318=CARTESIAN_POINT('Ctrl Pts',(96.5278957107626,-1.46299164026993,-4.78196165636301));
#35319=CARTESIAN_POINT('Ctrl Pts',(96.5831943289659,-1.45939569982424,-4.77896163442842));
#35320=CARTESIAN_POINT('Ctrl Pts',(96.6381217070322,-1.45267890853097,-4.77596161249382));
#35321=CARTESIAN_POINT('Ctrl Pts',(96.6930381322474,-1.44596345660649,-4.77296218878173));
#35322=CARTESIAN_POINT('Ctrl Pts',(96.7475829404237,-1.43612845379554,-4.76996276506964));
#35323=CARTESIAN_POINT('Ctrl Pts',(96.8013806630584,-1.42324264809214,-4.76696334135755));
#35324=CARTESIAN_POINT('Ctrl Pts',(96.8552278449069,-1.41034499575678,-4.76396116010979));
#35325=CARTESIAN_POINT('Ctrl Pts',(96.9083260543104,-1.39439106024103,-4.76095897886203));
#35326=CARTESIAN_POINT('Ctrl Pts',(96.9603121585099,-1.3755002771998,-4.75795679761428));
#35327=CARTESIAN_POINT('Ctrl Pts',(97.0123219256299,-1.35660089549348,-4.75495324984026));
#35328=CARTESIAN_POINT('Ctrl Pts',(97.0632180922886,-1.33476221007533,-4.75194970206625));
#35329=CARTESIAN_POINT('Ctrl Pts',(97.1126578904773,-1.31015170410069,-4.74894615429223));
#35330=CARTESIAN_POINT('Ctrl Pts',(97.1621909979647,-1.2854947499378,-4.74593693782727));
#35331=CARTESIAN_POINT('Ctrl Pts',(97.2102617863444,-1.25805578723982,-4.7429277213623));
#35332=CARTESIAN_POINT('Ctrl Pts',(97.2565534919671,-1.22804753867779,-4.73991850489734));
#35333=CARTESIAN_POINT('Ctrl Pts',(97.2919685439525,-1.2050899986926,-4.7376163309742));
#35334=CARTESIAN_POINT('Ctrl Pts',(97.3263428475686,-1.18062963609603,-4.73531415705106));
#35335=CARTESIAN_POINT('Ctrl Pts',(97.3595479090547,-1.15477740382097,-4.73301198312793));
#35336=CARTESIAN_POINT('Ctrl Pts',(97.4030324702889,-1.12092193338683,-4.72999711074245));
#35337=CARTESIAN_POINT('Ctrl Pts',(97.4447047082584,-1.08452667630381,-4.72698223835697));
#35338=CARTESIAN_POINT('Ctrl Pts',(97.4842490377971,-1.04581602184234,-4.7239673659715));
#35339=CARTESIAN_POINT('Ctrl Pts',(97.5232220531078,-1.00766463714034,-4.72099605076627));
#35340=CARTESIAN_POINT('Ctrl Pts',(97.5601278206889,-0.967264685987466,
-4.71802473556104));
#35341=CARTESIAN_POINT('Ctrl Pts',(97.5946952874807,-0.924873010576951,
-4.71505342035581));
#35342=CARTESIAN_POINT('Ctrl Pts',(97.6292292884123,-0.882522375891087,
-4.71208498177501));
#35343=CARTESIAN_POINT('Ctrl Pts',(97.6614291294895,-0.838184251342567,
-4.70911654319421));
#35344=CARTESIAN_POINT('Ctrl Pts',(97.6910615717155,-0.792151237086225,
-4.70614810461341));
#35345=CARTESIAN_POINT('Ctrl Pts',(97.7206776781764,-0.746143599898085,
-4.70318130247267));
#35346=CARTESIAN_POINT('Ctrl Pts',(97.7477288975073,-0.698443378368204,
-4.70021450033193));
#35347=CARTESIAN_POINT('Ctrl Pts',(97.7720246603957,-0.649373039640524,
-4.69724769819118));
#35348=CARTESIAN_POINT('Ctrl Pts',(97.7969967336336,-0.59893675171043,-4.69419831049829));
#35349=CARTESIAN_POINT('Ctrl Pts',(97.8190573105785,-0.54705342191283,-4.6911489228054));
#35350=CARTESIAN_POINT('Ctrl Pts',(97.8380507198851,-0.494098955608387,
-4.68809953511251));
#35351=CARTESIAN_POINT('Ctrl Pts',(97.8565434550433,-0.442540391002808,
-4.68513053054418));
#35352=CARTESIAN_POINT('Ctrl Pts',(97.8721286571858,-0.389967029528204,
-4.68216152597585));
#35353=CARTESIAN_POINT('Ctrl Pts',(97.8847130788941,-0.33674187714174,-4.67919252140752));
#35354=CARTESIAN_POINT('Ctrl Pts',(97.8978085684271,-0.281355190162321,
-4.67610294215235));
#35355=CARTESIAN_POINT('Ctrl Pts',(97.9076541361318,-0.225263256882713,
-4.67301336289717));
#35356=CARTESIAN_POINT('Ctrl Pts',(97.9142039062054,-0.168884029356592,
-4.669923783642));
#35357=CARTESIAN_POINT('Ctrl Pts',(97.9207536762789,-0.112504801830471,
-4.66683420438683));
#35358=CARTESIAN_POINT('Ctrl Pts',(97.9240076811728,-0.0558389356524655,
-4.66374462513166));
#35359=CARTESIAN_POINT('Ctrl Pts',(97.9239807839468,0.000696275558458027,
-4.66065504587649));
#35360=CARTESIAN_POINT('Ctrl Pts',(97.9239807519797,0.000760504599684739,
-4.58934495419114));
#35361=CARTESIAN_POINT('Ctrl Pts',(97.9240091441741,-0.0538768649333986,
-4.59233017755843));
#35362=CARTESIAN_POINT('Ctrl Pts',(97.9209735154324,-0.108635686920582,
-4.59531540092572));
#35363=CARTESIAN_POINT('Ctrl Pts',(97.914859816964,-0.163139082068399,-4.59830062429302));
#35364=CARTESIAN_POINT('Ctrl Pts',(97.9087809889155,-0.217331608716174,
-4.60126882097953));
#35365=CARTESIAN_POINT('Ctrl Pts',(97.8996591242802,-0.271271069183976,
-4.60423701766605));
#35366=CARTESIAN_POINT('Ctrl Pts',(97.8875324670009,-0.324586223703797,
-4.60720521435256));
#35367=CARTESIAN_POINT('Ctrl Pts',(97.8754160378309,-0.377856410082728,
-4.61017090754288));
#35368=CARTESIAN_POINT('Ctrl Pts',(97.8602999526874,-0.430502806405192,
-4.61313660073319));
#35369=CARTESIAN_POINT('Ctrl Pts',(97.8422738547964,-0.482162438484627,
-4.61610229392351));
#35370=CARTESIAN_POINT('Ctrl Pts',(97.8242554245078,-0.53380009656151,-4.61906672562304));
#35371=CARTESIAN_POINT('Ctrl Pts',(97.8033296126891,-0.584451311009786,
-4.62203115732257));
#35372=CARTESIAN_POINT('Ctrl Pts',(97.7796357286456,-0.633768821306631,
-4.6249955890221));
#35373=CARTESIAN_POINT('Ctrl Pts',(97.7556610698103,-0.683670748816948,
-4.62799514952077));
#35374=CARTESIAN_POINT('Ctrl Pts',(97.7288524993572,-0.73220662233431,-4.63099471001945));
#35375=CARTESIAN_POINT('Ctrl Pts',(97.6994031308721,-0.779040485915271,
-4.63399427051812));
#35376=CARTESIAN_POINT('Ctrl Pts',(97.670268647178,-0.825373582515089,-4.63696175847908));
#35377=CARTESIAN_POINT('Ctrl Pts',(97.6385499376378,-0.870040477952918,
-4.63992924644005));
#35378=CARTESIAN_POINT('Ctrl Pts',(97.60447702287,-0.91274598563359,-4.64289673440101));
#35379=CARTESIAN_POINT('Ctrl Pts',(97.5698517192511,-0.956143833446764,
-4.64591233116854));
#35380=CARTESIAN_POINT('Ctrl Pts',(97.5327955634189,-0.997515679528127,
-4.64892792793607));
#35381=CARTESIAN_POINT('Ctrl Pts',(97.4935895731258,-1.0365899970331,-4.65194352470359));
#35382=CARTESIAN_POINT('Ctrl Pts',(97.4543835828327,-1.07566431453807,-4.65495912147112));
#35383=CARTESIAN_POINT('Ctrl Pts',(97.4130282385493,-1.11244077228239,-4.65797471823865));
#35384=CARTESIAN_POINT('Ctrl Pts',(97.3698377702358,-1.14669194761335,-4.66099031500617));
#35385=CARTESIAN_POINT('Ctrl Pts',(97.3267256181196,-1.18088101614369,-4.66400044366741));
#35386=CARTESIAN_POINT('Ctrl Pts',(97.2815920934796,-1.21270720915157,-4.66701057232865));
#35387=CARTESIAN_POINT('Ctrl Pts',(97.2347264161452,-1.24192439685295,-4.67002070098989));
#35388=CARTESIAN_POINT('Ctrl Pts',(97.1879440323248,-1.27108965737927,-4.67302547980433));
#35389=CARTESIAN_POINT('Ctrl Pts',(97.1394360496944,-1.29765483749973,-4.67603025861878));
#35390=CARTESIAN_POINT('Ctrl Pts',(97.0895231307834,-1.32141522023288,-4.67903503743322));
#35391=CARTESIAN_POINT('Ctrl Pts',(97.0396595924364,-1.34515209600379,-4.68203684351684));
#35392=CARTESIAN_POINT('Ctrl Pts',(96.9883943457357,-1.36608944541673,-4.68503864960047));
#35393=CARTESIAN_POINT('Ctrl Pts',(96.9360736651233,-1.38406785199257,-4.68804045568409));
#35394=CARTESIAN_POINT('Ctrl Pts',(96.8837840817532,-1.40203557294928,-4.69104047761869));
#35395=CARTESIAN_POINT('Ctrl Pts',(96.8304408062886,-1.41704766559507,-4.69404049955329));
#35396=CARTESIAN_POINT('Ctrl Pts',(96.7764090088346,-1.42899325098956,-4.69704052148789));
#35397=CARTESIAN_POINT('Ctrl Pts',(96.7223879856477,-1.4409364543621,-4.70003994519998));
#35398=CARTESIAN_POINT('Ctrl Pts',(96.6676792285092,-1.44981425091521,-4.70303936891206));
#35399=CARTESIAN_POINT('Ctrl Pts',(96.6126596829523,-1.45556651620883,-4.70603879262415));
#35400=CARTESIAN_POINT('Ctrl Pts',(96.5575895548922,-1.46132406987723,-4.70904097387191));
#35401=CARTESIAN_POINT('Ctrl Pts',(96.5022085939542,-1.46395029642693,-4.71204315511967));
#35402=CARTESIAN_POINT('Ctrl Pts',(96.4468989816342,-1.46343697511946,-4.71504533636743));
#35403=CARTESIAN_POINT('Ctrl Pts',(96.3915641936065,-1.46292342015954,-4.71804888414145));
#35404=CARTESIAN_POINT('Ctrl Pts',(96.336301346819,-1.45926750354694,-4.72105243191547));
#35405=CARTESIAN_POINT('Ctrl Pts',(96.2814894087509,-1.45251309058222,-4.72405597968949));
#35406=CARTESIAN_POINT('Ctrl Pts',(96.2265740223742,-1.44574592979974,-4.72706519615446));
#35407=CARTESIAN_POINT('Ctrl Pts',(96.1721117656645,-1.43586868506868,-4.73007441261943));
#35408=CARTESIAN_POINT('Ctrl Pts',(96.1184721394553,-1.42297653662988,-4.73308362908439));
#35409=CARTESIAN_POINT('Ctrl Pts',(96.0774356270801,-1.4131135147123,-4.73538580300751));
#35410=CARTESIAN_POINT('Ctrl Pts',(96.0368804091218,-1.40148697680282,-4.73768797693062));
#35411=CARTESIAN_POINT('Ctrl Pts',(95.9969645796261,-1.38815878947169,-4.73999015085374));
#35412=CARTESIAN_POINT('Ctrl Pts',(95.944774003929,-1.37073197463162,-4.74300027951497));
#35413=CARTESIAN_POINT('Ctrl Pts',(95.8934579300621,-1.35032113999202,-4.74601040817621));
#35414=CARTESIAN_POINT('Ctrl Pts',(95.8433805269229,-1.3270340305961,-4.74902053683745));
#35415=CARTESIAN_POINT('Ctrl Pts',(95.7933921254394,-1.30378830895515,-4.75202531565189));
#35416=CARTESIAN_POINT('Ctrl Pts',(95.7446385008558,-1.27767667814304,-4.75503009446634));
#35417=CARTESIAN_POINT('Ctrl Pts',(95.6974663179009,-1.24885584510312,-4.75803487328078));
#35418=CARTESIAN_POINT('Ctrl Pts',(95.650340804006,-1.22006352550266,-4.7610366793644));
#35419=CARTESIAN_POINT('Ctrl Pts',(95.6047940808374,-1.18856758721971,-4.76403848544802));
#35420=CARTESIAN_POINT('Ctrl Pts',(95.5611488669825,-1.15457093988041,-4.76704029153163));
#35421=CARTESIAN_POINT('Ctrl Pts',(95.5175295940325,-1.12059449873814,-4.77004031346623));
#35422=CARTESIAN_POINT('Ctrl Pts',(95.4758100061135,-1.08412061840237,-4.77304033540082));
#35423=CARTESIAN_POINT('Ctrl Pts',(95.4362824948339,-1.04539455484612,-4.77604035733542));
#35424=CARTESIAN_POINT('Ctrl Pts',(95.396762865579,-1.00667621350098,-4.77903978104751));
#35425=CARTESIAN_POINT('Ctrl Pts',(95.3594348219031,-0.965706950209886,
-4.7820392047596));
#35426=CARTESIAN_POINT('Ctrl Pts',(95.3245546812025,-0.922769615243584,
-4.78503862847169));
#35427=CARTESIAN_POINT('Ctrl Pts',(95.2896424732645,-0.879792805616806,
-4.78804080971945));
#35428=CARTESIAN_POINT('Ctrl Pts',(95.2571829981975,-0.834844720244155,
-4.79104299096721));
#35429=CARTESIAN_POINT('Ctrl Pts',(95.22739196356,-0.788240954634715,-4.79404517221497));
#35430=CARTESIAN_POINT('Ctrl Pts',(95.1975873687048,-0.741615976025689,
-4.79704871998899));
#35431=CARTESIAN_POINT('Ctrl Pts',(95.1704538947152,-0.693334276070171,
-4.80005226776301));
#35432=CARTESIAN_POINT('Ctrl Pts',(95.1461618695643,-0.643737218059181,
-4.80305581553703));
#35433=CARTESIAN_POINT('Ctrl Pts',(95.1218239973042,-0.594046553948072,
-4.80606503200199));
#35434=CARTESIAN_POINT('Ctrl Pts',(95.1003384923237,-0.543036060467608,
-4.80907424846695));
#35435=CARTESIAN_POINT('Ctrl Pts',(95.0818275324146,-0.491067210620215,
-4.81208346493192));
#35436=CARTESIAN_POINT('Ctrl Pts',(95.067665889445,-0.451308910635289,-4.81438563885505));
#35437=CARTESIAN_POINT('Ctrl Pts',(95.0552442159601,-0.410990129462408,
-4.81668781277818));
#35438=CARTESIAN_POINT('Ctrl Pts',(95.0445970790082,-0.370277078770857,
-4.8189899867013));
#35439=CARTESIAN_POINT('Ctrl Pts',(95.0306757797627,-0.317044123805158,
-4.82200011536254));
#35440=CARTESIAN_POINT('Ctrl Pts',(95.0197315017751,-0.262913130953223,
-4.82501024402378));
#35441=CARTESIAN_POINT('Ctrl Pts',(95.011872986128,-0.208247972936347,-4.82802037268502));
#35442=CARTESIAN_POINT('Ctrl Pts',(95.0040284372775,-0.153679970308288,
-4.83102515149946));
#35443=CARTESIAN_POINT('Ctrl Pts',(94.9992588417388,-0.0985802050447275,
-4.8340299303139));
#35444=CARTESIAN_POINT('Ctrl Pts',(94.9976223694762,-0.0433246422445049,
-4.83703470912835));
#35445=CARTESIAN_POINT('Ctrl Pts',(94.9959875162319,0.0118762543307089,
-4.84003651521197));
#35446=CARTESIAN_POINT('Ctrl Pts',(94.9974796614516,0.0672321178174589,
-4.84303832129558));
#35447=CARTESIAN_POINT('Ctrl Pts',(95.0021051950319,0.122361793690261,-4.8460401273792));
#35448=CARTESIAN_POINT('Ctrl Pts',(95.0067279793869,0.177458702770457,-4.84904014931379));
#35449=CARTESIAN_POINT('Ctrl Pts',(95.0144804167235,0.23232916548243,-4.85204017124839));
#35450=CARTESIAN_POINT('Ctrl Pts',(95.0253168601906,0.286594289084048,-4.85504019318298));
#35451=CARTESIAN_POINT('Ctrl Pts',(95.0361511428054,0.340848591892115,-4.85803961689508));
#35452=CARTESIAN_POINT('Ctrl Pts',(95.0500681068859,0.394497277710787,-4.86103904060717));
#35453=CARTESIAN_POINT('Ctrl Pts',(95.0669709085371,0.447171125544849,-4.86403846431926));
#35454=CARTESIAN_POINT('Ctrl Pts',(95.0838892498663,0.499893399352681,-4.86704064556702));
#35455=CARTESIAN_POINT('Ctrl Pts',(95.1037987512976,0.551638540699961,-4.87004282681477));
#35456=CARTESIAN_POINT('Ctrl Pts',(95.1265529548619,0.602053448553728,-4.87304500806253));
#35457=CARTESIAN_POINT('Ctrl Pts',(95.1493175156346,0.652491304154378,-4.87604855583654));
#35458=CARTESIAN_POINT('Ctrl Pts',(95.1749291150773,0.701597250182519,-4.87905210361056));
#35459=CARTESIAN_POINT('Ctrl Pts',(95.2031949187827,0.74904211281437,-4.88205565138457));
#35460=CARTESIAN_POINT('Ctrl Pts',(95.2315140694356,0.796576519639843,-4.88506486784954));
#35461=CARTESIAN_POINT('Ctrl Pts',(95.2624971349902,0.842443141689295,-4.8880740843145));
#35462=CARTESIAN_POINT('Ctrl Pts',(95.2959081295444,0.886342144344518,-4.89108330077947));
#35463=CARTESIAN_POINT('Ctrl Pts',(95.321468909669,0.919926680499025,-4.8933854747026));
#35464=CARTESIAN_POINT('Ctrl Pts',(95.3484498203687,0.952360190103343,-4.89568764862573));
#35465=CARTESIAN_POINT('Ctrl Pts',(95.3767305421968,0.983522904920491,-4.89798982254886));
#35466=CARTESIAN_POINT('Ctrl Pts',(95.4137080313777,1.02426864532291,-4.9009999512101));
#35467=CARTESIAN_POINT('Ctrl Pts',(95.4530642841859,1.06301173467717,-4.90401007987134));
#35468=CARTESIAN_POINT('Ctrl Pts',(95.4945539631249,1.09946228077349,-4.90702020853258));
#35469=CARTESIAN_POINT('Ctrl Pts',(95.535969903214,1.13584804397874,-4.91002498734703));
#35470=CARTESIAN_POINT('Ctrl Pts',(95.5795113512401,1.16994900404589,-4.91302976616147));
#35471=CARTESIAN_POINT('Ctrl Pts',(95.6248952101548,1.20151101621011,-4.91603454497592));
#35472=CARTESIAN_POINT('Ctrl Pts',(95.67023416926,1.23304180299228,-4.91903635105954));
#35473=CARTESIAN_POINT('Ctrl Pts',(95.7174114970096,1.2620383177162,-4.92203815714317));
#35474=CARTESIAN_POINT('Ctrl Pts',(95.7661114576449,1.28828694733509,-4.92503996322679));
#35475=CARTESIAN_POINT('Ctrl Pts',(95.8147824730437,1.31451997585735,-4.92803998516139));
#35476=CARTESIAN_POINT('Ctrl Pts',(95.8649738636181,1.33800810637278,-4.93104000709599));
#35477=CARTESIAN_POINT('Ctrl Pts',(95.9163433552392,1.35858254384057,-4.93404002903059));
#35478=CARTESIAN_POINT('Ctrl Pts',(95.9677026034731,1.37915287864111,-4.93703945274268));
#35479=CARTESIAN_POINT('Ctrl Pts',(96.0202389962309,1.39681047800454,-4.94003887645477));
#35480=CARTESIAN_POINT('Ctrl Pts',(96.0735903858681,1.41143471039685,-4.94303830016685));
#35481=CARTESIAN_POINT('Ctrl Pts',(96.126990824381,1.42607238765272,-4.94604048141462));
#35482=CARTESIAN_POINT('Ctrl Pts',(96.1812072462982,1.43767098648151,-4.94904266266238));
#35483=CARTESIAN_POINT('Ctrl Pts',(96.2358638959425,1.44616023635576,-4.95204484391014));
#35484=CARTESIAN_POINT('Ctrl Pts',(96.2905454240803,1.4546533503481,-4.95504839168416));
#35485=CARTESIAN_POINT('Ctrl Pts',(96.3456670528585,1.46003424267022,-4.95805193945818));
#35486=CARTESIAN_POINT('Ctrl Pts',(96.4008477263775,1.46228455804294,-4.9610554872322));
#35487=CARTESIAN_POINT('Ctrl Pts',(96.4561325441311,1.46453912050721,-4.96406470369717));
#35488=CARTESIAN_POINT('Ctrl Pts',(96.5114760998946,1.46365131149304,-4.96707392016214));
#35489=CARTESIAN_POINT('Ctrl Pts',(96.5664983323353,1.45965494708615,-4.97008313662711));
#35490=CARTESIAN_POINT('Ctrl Pts',(96.6085925951411,1.45659756453097,-4.97238531055022));
#35491=CARTESIAN_POINT('Ctrl Pts',(96.6504987960049,1.45172186801079,-4.97468748447332));
#35492=CARTESIAN_POINT('Ctrl Pts',(96.6920508837316,1.44506318740587,-4.97698965839643));
#35493=CARTESIAN_POINT('Ctrl Pts',(96.7463808928353,1.43635685764783,-4.97999978705767));
#35494=CARTESIAN_POINT('Ctrl Pts',(96.8003333748968,1.4245640086614,-4.9830099157189));
#35495=CARTESIAN_POINT('Ctrl Pts',(96.8535314859436,1.40973172123703,-4.98602004438014));
#35496=CARTESIAN_POINT('Ctrl Pts',(96.9066350489574,1.39492579496673,-4.98902482319459));
#35497=CARTESIAN_POINT('Ctrl Pts',(96.9589863970451,1.37709129113013,-4.99202960200903));
#35498=CARTESIAN_POINT('Ctrl Pts',(97.0102179940105,1.35632644742242,-4.99503438082347));
#35499=CARTESIAN_POINT('Ctrl Pts',(97.0613989057984,1.33558214708737,-4.99803618690708));
#35500=CARTESIAN_POINT('Ctrl Pts',(97.1114617739434,1.31191344723268,-5.0010379929907));
#35501=CARTESIAN_POINT('Ctrl Pts',(97.1600551749908,1.28546806772345,-5.00403979907431));
#35502=CARTESIAN_POINT('Ctrl Pts',(97.2086196941363,1.25903840625081,-5.00703982100891));
#35503=CARTESIAN_POINT('Ctrl Pts',(97.2557160143554,1.22983558815536,-5.01003984294351));
#35504=CARTESIAN_POINT('Ctrl Pts',(97.3010157480182,1.19805404828389,-5.01303986487811));
#35505=CARTESIAN_POINT('Ctrl Pts',(97.3463064486402,1.16627884584363,-5.0160392885902));
#35506=CARTESIAN_POINT('Ctrl Pts',(97.3898008420902,1.13192624597563,-5.01903871230228));
#35507=CARTESIAN_POINT('Ctrl Pts',(97.4312000201607,1.09523364448186,-5.02203813601437));
#35508=CARTESIAN_POINT('Ctrl Pts',(97.4726372587793,1.05850730945553,-5.02504031726212));
#35509=CARTESIAN_POINT('Ctrl Pts',(97.5119750375536,1.01943702584515,-5.02804249850988));
#35510=CARTESIAN_POINT('Ctrl Pts',(97.5489491915986,0.978299103602973,-5.03104467975764));
#35511=CARTESIAN_POINT('Ctrl Pts',(97.5859401754578,0.937142456291722,-5.03404822753166));
#35512=CARTESIAN_POINT('Ctrl Pts',(97.6205650591715,0.893916707146538,-5.03705177530568));
#35513=CARTESIAN_POINT('Ctrl Pts',(97.6526002622515,0.848930971486213,-5.0400553230797));
#35514=CARTESIAN_POINT('Ctrl Pts',(97.684695926386,0.803860332820683,-5.04306453954466));
#35515=CARTESIAN_POINT('Ctrl Pts',(97.7141918640548,0.757023520051016,-5.04607375600963));
#35516=CARTESIAN_POINT('Ctrl Pts',(97.7409087331197,0.708757321748395,-5.04908297247459));
#35517=CARTESIAN_POINT('Ctrl Pts',(97.7613482328981,0.671831701941769,-5.05138514639773));
#35518=CARTESIAN_POINT('Ctrl Pts',(97.7801620894879,0.63407006946034,-5.05368732032086));
#35519=CARTESIAN_POINT('Ctrl Pts',(97.7972891628933,0.595630800756833,-5.05598949424399));
#35520=CARTESIAN_POINT('Ctrl Pts',(97.8217753637232,0.540675022209471,-5.05928086175863));
#35521=CARTESIAN_POINT('Ctrl Pts',(97.8429012861721,0.484134691290987,-5.06257222927327));
#35522=CARTESIAN_POINT('Ctrl Pts',(97.8604806286845,0.426418982338702,-5.06586359678791));
#35523=CARTESIAN_POINT('Ctrl Pts',(97.8780070246564,0.368877105093971,-5.06914505116026));
#35524=CARTESIAN_POINT('Ctrl Pts',(97.8920079878108,0.310167235961735,-5.07242650553261));
#35525=CARTESIAN_POINT('Ctrl Pts',(97.9023453525958,0.25071755683876,-5.07570795990496));
#35526=CARTESIAN_POINT('Ctrl Pts',(97.9126346019441,0.191544587238597,-5.07897414069321));
#35527=CARTESIAN_POINT('Ctrl Pts',(97.9192941361081,0.131639017028875,-5.08224032148147));
#35528=CARTESIAN_POINT('Ctrl Pts',(97.9222362222824,0.071440693711251,-5.08550650226972));
#35529=CARTESIAN_POINT('Ctrl Pts',(97.923388746375,0.0478587814731765,-5.08678598622305));
#35530=CARTESIAN_POINT('Ctrl Pts',(97.9239713369921,0.0242321078176,-5.08806547017638));
#35531=CARTESIAN_POINT('Ctrl Pts',(97.9239808315836,0.000587678971723866,
-5.08934495412971));
#35532=CARTESIAN_POINT('Origin',(96.460480949577,-8.32667268468867E-16,
1.18130019239114E-14));
#35533=CARTESIAN_POINT('',(97.9239803738018,-0.00129818862389702,-5.66065504588482));
#35534=CARTESIAN_POINT('',(97.9239803690929,-0.00130348633276278,-5.58934495420992));
#35535=CARTESIAN_POINT('',(97.923980949577,-1.01189432752408E-15,1.19922289829666E-14));
#35536=CARTESIAN_POINT('Ctrl Pts',(97.9239803738025,-0.00129818785261365,
-5.6606550458429));
#35537=CARTESIAN_POINT('Ctrl Pts',(97.9240288523407,0.0533536197810905,
-5.65768502711363));
#35538=CARTESIAN_POINT('Ctrl Pts',(97.9210117416233,0.10807933482888,-5.65471500838436));
#35539=CARTESIAN_POINT('Ctrl Pts',(97.9149308469247,0.16250460333544,-5.65174498965509));
#35540=CARTESIAN_POINT('Ctrl Pts',(97.9088537700624,0.216895701416044,-5.64877683562595));
#35541=CARTESIAN_POINT('Ctrl Pts',(97.8997167787174,0.270986190441221,-5.64580868159681));
#35542=CARTESIAN_POINT('Ctrl Pts',(97.8875736481521,0.324405116595969,-5.64284052756767));
#35543=CARTESIAN_POINT('Ctrl Pts',(97.8754330899258,0.377812726756813,-5.63987300229719));
#35544=CARTESIAN_POINT('Ctrl Pts',(97.8602877763835,0.430548529546161,-5.63690547702672));
#35545=CARTESIAN_POINT('Ctrl Pts',(97.8422424151804,0.482252529462982,-5.63393795175625));
#35546=CARTESIAN_POINT('Ctrl Pts',(97.8241808024205,0.534003093728886,-5.6309677539482));
#35547=CARTESIAN_POINT('Ctrl Pts',(97.8032141053442,0.584719488164546,-5.62799755614015));
#35548=CARTESIAN_POINT('Ctrl Pts',(97.7794961401501,0.634059285112504,-5.6250273583321));
#35549=CARTESIAN_POINT('Ctrl Pts',(97.7557667425137,0.683422864639655,-5.62205572884072));
#35550=CARTESIAN_POINT('Ctrl Pts',(97.7292836989253,0.731408052320245,-5.61908409934935));
#35551=CARTESIAN_POINT('Ctrl Pts',(97.7002464014614,0.777697803979105,-5.61611246985798));
#35552=CARTESIAN_POINT('Ctrl Pts',(97.6711562336171,0.824071838852656,-5.61313542969842));
#35553=CARTESIAN_POINT('Ctrl Pts',(97.6395028433694,0.868743835850687,-5.61015838953886));
#35554=CARTESIAN_POINT('Ctrl Pts',(97.6055275969137,0.911427685240538,-5.60718134937931));
#35555=CARTESIAN_POINT('Ctrl Pts',(97.5858557269457,0.936141888153743,-5.60545762540324));
#35556=CARTESIAN_POINT('Ctrl Pts',(97.5654061942646,0.960190211352029,-5.60373390142718));
#35557=CARTESIAN_POINT('Ctrl Pts',(97.5442313569573,0.983522904920419,-5.60201017745112));
#35558=CARTESIAN_POINT('Ctrl Pts',(97.5072538677764,1.02426864532281,-5.59900004878988));
#35559=CARTESIAN_POINT('Ctrl Pts',(97.4678976149683,1.06301173467705,-5.59598992012864));
#35560=CARTESIAN_POINT('Ctrl Pts',(97.4264079360292,1.09946228077335,-5.5929797914674));
#35561=CARTESIAN_POINT('Ctrl Pts',(97.3849919959402,1.13584804397859,-5.58997501265296));
#35562=CARTESIAN_POINT('Ctrl Pts',(97.3414505479141,1.16994900404574,-5.58697023383851));
#35563=CARTESIAN_POINT('Ctrl Pts',(97.2960666889994,1.20151101620996,-5.58396545502407));
#35564=CARTESIAN_POINT('Ctrl Pts',(97.2507277298942,1.23304180299214,-5.58096364894044));
#35565=CARTESIAN_POINT('Ctrl Pts',(97.2035504021446,1.26203831771606,-5.57796184285682));
#35566=CARTESIAN_POINT('Ctrl Pts',(97.1548504415093,1.28828694733496,-5.5749600367732));
#35567=CARTESIAN_POINT('Ctrl Pts',(97.1061794261105,1.31451997585722,-5.5719600148386));
#35568=CARTESIAN_POINT('Ctrl Pts',(97.0559880355362,1.33800810637265,-5.568959992904));
#35569=CARTESIAN_POINT('Ctrl Pts',(97.0046185439151,1.35858254384045,-5.5659599709694));
#35570=CARTESIAN_POINT('Ctrl Pts',(96.9532592956811,1.37915287864104,-5.56296054725731));
#35571=CARTESIAN_POINT('Ctrl Pts',(96.9007229029232,1.39681047800451,-5.55996112354522));
#35572=CARTESIAN_POINT('Ctrl Pts',(96.8473715132859,1.41143471039685,-5.55696169983312));
#35573=CARTESIAN_POINT('Ctrl Pts',(96.7939710747731,1.42607238765271,-5.55395951858536));
#35574=CARTESIAN_POINT('Ctrl Pts',(96.7397546528558,1.4376709864815,-5.5509573373376));
#35575=CARTESIAN_POINT('Ctrl Pts',(96.6850980032116,1.44616023635575,-5.54795515608984));
#35576=CARTESIAN_POINT('Ctrl Pts',(96.6304164750737,1.45465335034809,-5.54495160831582));
#35577=CARTESIAN_POINT('Ctrl Pts',(96.5752948462955,1.46003424267022,-5.54194806054179));
#35578=CARTESIAN_POINT('Ctrl Pts',(96.5201141727766,1.46228455804294,-5.53894451276777));
#35579=CARTESIAN_POINT('Ctrl Pts',(96.4648293550229,1.46453912050721,-5.5359352963028));
#35580=CARTESIAN_POINT('Ctrl Pts',(96.4094857992594,1.46365131149304,-5.53292607983784));
#35581=CARTESIAN_POINT('Ctrl Pts',(96.3544635668188,1.45965494708616,-5.52991686337287));
#35582=CARTESIAN_POINT('Ctrl Pts',(96.312369304013,1.45659756453098,-5.52761468944977));
#35583=CARTESIAN_POINT('Ctrl Pts',(96.2704631031492,1.4517218680108,-5.52531251552666));
#35584=CARTESIAN_POINT('Ctrl Pts',(96.2289110154224,1.44506318740588,-5.52301034160356));
#35585=CARTESIAN_POINT('Ctrl Pts',(96.1745810063187,1.43635685764784,-5.52000021294232));
#35586=CARTESIAN_POINT('Ctrl Pts',(96.1206285242573,1.42456400866141,-5.51699008428108));
#35587=CARTESIAN_POINT('Ctrl Pts',(96.0674304132104,1.40973172123704,-5.51397995561984));
#35588=CARTESIAN_POINT('Ctrl Pts',(96.0143268501966,1.39492579496673,-5.5109751768054));
#35589=CARTESIAN_POINT('Ctrl Pts',(95.9619755021089,1.37709129113012,-5.50797039799096));
#35590=CARTESIAN_POINT('Ctrl Pts',(95.9107439051434,1.35632644742238,-5.50496561917651));
#35591=CARTESIAN_POINT('Ctrl Pts',(95.8595629933555,1.33558214708731,-5.5019638130929));
#35592=CARTESIAN_POINT('Ctrl Pts',(95.8095001252104,1.3119134472326,-5.49896200700928));
#35593=CARTESIAN_POINT('Ctrl Pts',(95.760906724163,1.28546806772334,-5.49596020092566));
#35594=CARTESIAN_POINT('Ctrl Pts',(95.7123422050175,1.25903840625068,-5.49296017899106));
#35595=CARTESIAN_POINT('Ctrl Pts',(95.6652458847984,1.22983558815522,-5.48996015705646));
#35596=CARTESIAN_POINT('Ctrl Pts',(95.6199461511356,1.19805404828372,-5.48696013512186));
#35597=CARTESIAN_POINT('Ctrl Pts',(95.5746554505134,1.16627884584334,-5.48396071140977));
#35598=CARTESIAN_POINT('Ctrl Pts',(95.5311610570632,1.13192624597521,-5.48096128769767));
#35599=CARTESIAN_POINT('Ctrl Pts',(95.4897618789926,1.09523364448129,-5.47796186398557));
#35600=CARTESIAN_POINT('Ctrl Pts',(95.4483246403741,1.0585073094549,-5.47495968273781));
#35601=CARTESIAN_POINT('Ctrl Pts',(95.4089868615997,1.01943702584445,-5.47195750149005));
#35602=CARTESIAN_POINT('Ctrl Pts',(95.3720127075547,0.978299103602208,-5.46895532024229));
#35603=CARTESIAN_POINT('Ctrl Pts',(95.3350217236955,0.937142456290982,-5.46595177246828));
#35604=CARTESIAN_POINT('Ctrl Pts',(95.300396839982,0.893916707145829,-5.46294822469426));
#35605=CARTESIAN_POINT('Ctrl Pts',(95.268361636902,0.848930971485543,-5.45994467692024));
#35606=CARTESIAN_POINT('Ctrl Pts',(95.2362659727676,0.803860332819978,-5.45693546045528));
#35607=CARTESIAN_POINT('Ctrl Pts',(95.2067700350987,0.757023520050274,-5.45392624399031));
#35608=CARTESIAN_POINT('Ctrl Pts',(95.1800531660339,0.708757321747617,-5.45091702752535));
#35609=CARTESIAN_POINT('Ctrl Pts',(95.1596136662556,0.67183170194124,-5.44861485360223));
#35610=CARTESIAN_POINT('Ctrl Pts',(95.140799809666,0.634070069460073,-5.44631267967911));
#35611=CARTESIAN_POINT('Ctrl Pts',(95.1236727362608,0.595630800756837,-5.44401050575599));
#35612=CARTESIAN_POINT('Ctrl Pts',(95.1012788180504,0.545370851550231,-5.44100037709476));
#35613=CARTESIAN_POINT('Ctrl Pts',(95.081676222055,0.493740629411957,-5.43799024843352));
#35614=CARTESIAN_POINT('Ctrl Pts',(95.0650314229126,0.441081476069969,-5.43498011977228));
#35615=CARTESIAN_POINT('Ctrl Pts',(95.0484162062683,0.38851591288124,-5.43197534095783));
#35616=CARTESIAN_POINT('Ctrl Pts',(95.0347485121264,0.334925547044205,-5.42897056214339));
#35617=CARTESIAN_POINT('Ctrl Pts',(95.0241468841081,0.280671876705698,-5.42596578332895));
#35618=CARTESIAN_POINT('Ctrl Pts',(95.0135557446443,0.226471881385568,-5.42296397724532));
#35619=CARTESIAN_POINT('Ctrl Pts',(95.0060247631399,0.171610397288745,-5.4199621711617));
#35620=CARTESIAN_POINT('Ctrl Pts',(95.0016222366284,0.116462464570799,-5.41696036507808));
#35621=CARTESIAN_POINT('Ctrl Pts',(94.997222326796,0.0613473094965147,-5.41396034314348));
#35622=CARTESIAN_POINT('Ctrl Pts',(94.9959472283989,0.0059465686443272,
-5.41096032120888));
#35623=CARTESIAN_POINT('Ctrl Pts',(94.9978135267317,-0.0493584860709382,
-5.40796029927428));
#35624=CARTESIAN_POINT('Ctrl Pts',(94.9996794529135,-0.104652512624003,
-5.40496087556219));
#35625=CARTESIAN_POINT('Ctrl Pts',(95.0046855139934,-0.159850363413252,
-5.4019614518501));
#35626=CARTESIAN_POINT('Ctrl Pts',(95.0127962068697,-0.214571982636142,
-5.39896202813801));
#35627=CARTESIAN_POINT('Ctrl Pts',(95.0209143563533,-0.269343910462044,
-5.39595984689025));
#35628=CARTESIAN_POINT('Ctrl Pts',(95.0321427624758,-0.323638208470656,
-5.39295766564249));
#35629=CARTESIAN_POINT('Ctrl Pts',(95.046394346872,-0.377082656788055,-5.38995548439472));
#35630=CARTESIAN_POINT('Ctrl Pts',(95.0606524182732,-0.43055143183191,-5.38695193662071));
#35631=CARTESIAN_POINT('Ctrl Pts',(95.077936245977,-0.483169083444685,-5.38394838884669));
#35632=CARTESIAN_POINT('Ctrl Pts',(95.0981091010857,-0.534579457553749,
-5.38094484107267));
#35633=CARTESIAN_POINT('Ctrl Pts',(95.1183200290636,-0.586086860091949,
-5.3779356246077));
#35634=CARTESIAN_POINT('Ctrl Pts',(95.1414306557218,-0.636381952346079,
-5.37492640814274));
#35635=CARTESIAN_POINT('Ctrl Pts',(95.1672569034086,-0.685130510495474,
-5.37191719167777));
#35636=CARTESIAN_POINT('Ctrl Pts',(95.187015041332,-0.722425155353208,-5.36961501775466));
#35637=CARTESIAN_POINT('Ctrl Pts',(95.2083616074269,-0.758815074333219,
-5.36731284383154));
#35638=CARTESIAN_POINT('Ctrl Pts',(95.2311973638051,-0.794162524771665,
-5.36501066990843));
#35639=CARTESIAN_POINT('Ctrl Pts',(95.2610554749082,-0.840379872904287,
-5.36200054124719));
#35640=CARTESIAN_POINT('Ctrl Pts',(95.2935863939703,-0.88500812530993,-5.35899041258595));
#35641=CARTESIAN_POINT('Ctrl Pts',(95.3285951991964,-0.927721347218681,
-5.35598028392472));
#35642=CARTESIAN_POINT('Ctrl Pts',(95.3635417839111,-0.970358655696832,
-5.35297550511027));
#35643=CARTESIAN_POINT('Ctrl Pts',(95.4009571831488,-1.01108728289679,-5.34997072629583));
#35644=CARTESIAN_POINT('Ctrl Pts',(95.4406034042517,-1.04961042417708,-5.34696594748138));
#35645=CARTESIAN_POINT('Ctrl Pts',(95.4802104019871,-1.08809545319132,-5.34396414139776));
#35646=CARTESIAN_POINT('Ctrl Pts',(95.5220434726716,-1.12437895242759,-5.34096233531414));
#35647=CARTESIAN_POINT('Ctrl Pts',(95.5658258273125,-1.1581988008135,-5.33796052923052));
#35648=CARTESIAN_POINT('Ctrl Pts',(95.6095821595379,-1.1919985480844,-5.33496050729593));
#35649=CARTESIAN_POINT('Ctrl Pts',(95.6552850622396,-1.22333722462838,-5.33196048536133));
#35650=CARTESIAN_POINT('Ctrl Pts',(95.7026242720679,-1.25199261433716,-5.32896046342673));
#35651=CARTESIAN_POINT('Ctrl Pts',(95.7499540421715,-1.28064228998804,-5.32596103971464));
#35652=CARTESIAN_POINT('Ctrl Pts',(95.7989190198661,-1.30660946809156,-5.32296161600254));
#35653=CARTESIAN_POINT('Ctrl Pts',(95.849181499433,-1.3297162224526,-5.31996219229045));
#35654=CARTESIAN_POINT('Ctrl Pts',(95.8994901880697,-1.35284422012747,-5.31696001104269));
#35655=CARTESIAN_POINT('Ctrl Pts',(95.951098280898,-1.37310631910394,-5.31395782979493));
#35656=CARTESIAN_POINT('Ctrl Pts',(96.0036464544788,-1.39037207037842,-5.31095564854717));
#35657=CARTESIAN_POINT('Ctrl Pts',(96.0562185468218,-1.4076456806396,-5.30795210077315));
#35658=CARTESIAN_POINT('Ctrl Pts',(96.1097310617508,-1.42192008806373,-5.30494855299913));
#35659=CARTESIAN_POINT('Ctrl Pts',(96.1638110025119,-1.43311520559528,-5.30194500522512));
#35660=CARTESIAN_POINT('Ctrl Pts',(96.21799301006,-1.44433145202711,-5.29893578876015));
#35661=CARTESIAN_POINT('Ctrl Pts',(96.2727440590942,-1.4524567211945,-5.29592657229519));
#35662=CARTESIAN_POINT('Ctrl Pts',(96.3276836488634,-1.45746256450146,-5.29291735583022));
#35663=CARTESIAN_POINT('Ctrl Pts',(96.3697146866388,-1.46129223978693,-5.2906151819071));
#35664=CARTESIAN_POINT('Ctrl Pts',(96.4118559030601,-1.46329722506164,-5.28831300798398));
#35665=CARTESIAN_POINT('Ctrl Pts',(96.4539377117467,-1.46348537267671,-5.28601083406087));
#35666=CARTESIAN_POINT('Ctrl Pts',(96.5089603393478,-1.46373137864655,-5.28300070539963));
#35667=CARTESIAN_POINT('Ctrl Pts',(96.5641124682866,-1.46087056035062,-5.27999057673839));
#35668=CARTESIAN_POINT('Ctrl Pts',(96.619014614918,-1.45488808055931,-5.27698044807715));
#35669=CARTESIAN_POINT('Ctrl Pts',(96.6738191849651,-1.44891623332027,-5.27397566926271));
#35670=CARTESIAN_POINT('Ctrl Pts',(96.7283741336371,-1.43983379151761,-5.27097089044826));
#35671=CARTESIAN_POINT('Ctrl Pts',(96.7823008408051,-1.42767790751623,-5.26796611163381));
#35672=CARTESIAN_POINT('Ctrl Pts',(96.8361741964306,-1.41553404974816,-5.2649643055502));
#35673=CARTESIAN_POINT('Ctrl Pts',(96.8894200291381,-1.40032288874674,-5.26196249946658));
#35674=CARTESIAN_POINT('Ctrl Pts',(96.941667569056,-1.38213302081762,-5.25896069338296));
#35675=CARTESIAN_POINT('Ctrl Pts',(96.9938840552034,-1.36395396419143,-5.25596067144835));
#35676=CARTESIAN_POINT('Ctrl Pts',(97.0451029268492,-1.34279988301938,-5.25296064951375));
#35677=CARTESIAN_POINT('Ctrl Pts',(97.0949685453458,-1.31880921319783,-5.24996062757914));
#35678=CARTESIAN_POINT('Ctrl Pts',(97.1448242203366,-1.29482332726092,-5.24696120386705));
#35679=CARTESIAN_POINT('Ctrl Pts',(97.193326702446,-1.26800220482898,-5.24396178015496));
#35680=CARTESIAN_POINT('Ctrl Pts',(97.2401424526182,-1.23853146535546,-5.24096235644287));
#35681=CARTESIAN_POINT('Ctrl Pts',(97.287001243092,-1.20903363180549,-5.23796017519511));
#35682=CARTESIAN_POINT('Ctrl Pts',(97.3321697556253,-1.17688159647601,-5.23495799394735));
#35683=CARTESIAN_POINT('Ctrl Pts',(97.3753424027505,-1.14230502559401,-5.23195581269959));
#35684=CARTESIAN_POINT('Ctrl Pts',(97.4185347011063,-1.10771271622452,-5.22895226492557));
#35685=CARTESIAN_POINT('Ctrl Pts',(97.4597289295779,-1.07069402497319,-5.22594871715155));
#35686=CARTESIAN_POINT('Ctrl Pts',(97.498654209139,-1.03151758740718,-5.22294516937753));
#35687=CARTESIAN_POINT('Ctrl Pts',(97.5376529536145,-0.992267210908366,
-5.21993595291257));
#35688=CARTESIAN_POINT('Ctrl Pts',(97.5743738434778,-0.950851349007003,
-5.2169267364476));
#35689=CARTESIAN_POINT('Ctrl Pts',(97.6085851481477,-0.907573137121431,
-5.21391751998263));
#35690=CARTESIAN_POINT('Ctrl Pts',(97.6347581983098,-0.874463531348052,
-5.21161534605952));
#35691=CARTESIAN_POINT('Ctrl Pts',(97.6594632226598,-0.840264644534702,
-5.20931317213641));
#35692=CARTESIAN_POINT('Ctrl Pts',(97.6826141364205,-0.805122800332881,
-5.2070109982133));
#35693=CARTESIAN_POINT('Ctrl Pts',(97.7134385129978,-0.758333051535094,
-5.20394575954988));
#35694=CARTESIAN_POINT('Ctrl Pts',(97.7416323362563,-0.709679539907104,
-5.20088052088647));
#35695=CARTESIAN_POINT('Ctrl Pts',(97.7669701794824,-0.659483238711326,
-5.19781528222305));
#35696=CARTESIAN_POINT('Ctrl Pts',(97.7925679753649,-0.608771950437985,
-5.19471859585804));
#35697=CARTESIAN_POINT('Ctrl Pts',(97.8152504927981,-0.556486417249488,
-5.19162190949302));
#35698=CARTESIAN_POINT('Ctrl Pts',(97.834829882593,-0.502988330200432,-5.18852522312801));
#35699=CARTESIAN_POINT('Ctrl Pts',(97.8541435920563,-0.450216179437119,
-5.18547055690095));
#35700=CARTESIAN_POINT('Ctrl Pts',(97.870437679572,-0.396264660733034,-5.18241589067389));
#35701=CARTESIAN_POINT('Ctrl Pts',(97.8835787106893,-0.341504044364106,
-5.17936122444683));
#35702=CARTESIAN_POINT('Ctrl Pts',(97.8969908948064,-0.285613493421438,
-5.17624352801284));
#35703=CARTESIAN_POINT('Ctrl Pts',(97.9071181978082,-0.22888056250821,-5.17312583157885));
#35704=CARTESIAN_POINT('Ctrl Pts',(97.9138720971347,-0.171716109322641,
-5.17000813514486));
#35705=CARTESIAN_POINT('Ctrl Pts',(97.9206259964612,-0.11455165613708,-5.16689043871087));
#35706=CARTESIAN_POINT('Ctrl Pts',(97.9240063897609,-0.0569562315344563,
-5.16377274227688));
#35707=CARTESIAN_POINT('Ctrl Pts',(97.9239808052397,0.000649980989679657,
-5.16065504584289));
#35708=CARTESIAN_POINT('Ctrl Pts',(97.9239808315838,0.000587678466145934,
-5.08934495415707));
#35709=CARTESIAN_POINT('Ctrl Pts',(97.9240035209153,-0.05591572584774,-5.09240255388167));
#35710=CARTESIAN_POINT('Ctrl Pts',(97.9207496103773,-0.112403252583685,
-5.09546015360626));
#35711=CARTESIAN_POINT('Ctrl Pts',(97.9142508208512,-0.168479706123258,
-5.09851775333086));
#35712=CARTESIAN_POINT('Ctrl Pts',(97.9077417371337,-0.224644985704266,
-5.10158019634462));
#35713=CARTESIAN_POINT('Ctrl Pts',(97.8979775678897,-0.280397394683033,
-5.10464263935838));
#35714=CARTESIAN_POINT('Ctrl Pts',(97.8850417680253,-0.335348661160212,
-5.10770508237214));
#35715=CARTESIAN_POINT('Ctrl Pts',(97.8720960647367,-0.390341997374302,
-5.11076986993918));
#35716=CARTESIAN_POINT('Ctrl Pts',(97.8559740363391,-0.444532490215592,
-5.11383465750622));
#35717=CARTESIAN_POINT('Ctrl Pts',(97.8368090965327,-0.497547065007448,
-5.11689944507326));
#35718=CARTESIAN_POINT('Ctrl Pts',(97.817598117962,-0.550688993474006,-5.11997159499226));
#35719=CARTESIAN_POINT('Ctrl Pts',(97.7953298137575,-0.602648896761696,
-5.12304374491126));
#35720=CARTESIAN_POINT('Ctrl Pts',(97.7701856592661,-0.653074133171955,
-5.12611589483027));
#35721=CARTESIAN_POINT('Ctrl Pts',(97.745977310828,-0.701622661359947,-5.12907370658403));
#35722=CARTESIAN_POINT('Ctrl Pts',(97.719103703838,-0.748748447528192,-5.13203151833779));
#35723=CARTESIAN_POINT('Ctrl Pts',(97.6897645353489,-0.794162524771699,
-5.13498933009155));
#35724=CARTESIAN_POINT('Ctrl Pts',(97.6599064242457,-0.840379872904354,
-5.13799945875279));
#35725=CARTESIAN_POINT('Ctrl Pts',(97.6273755051837,-0.885008125310025,
-5.14100958741403));
#35726=CARTESIAN_POINT('Ctrl Pts',(97.5923666999576,-0.927721347218802,
-5.14401971607527));
#35727=CARTESIAN_POINT('Ctrl Pts',(97.5574201152428,-0.970358655696963,
-5.14702449488971));
#35728=CARTESIAN_POINT('Ctrl Pts',(97.5200047160051,-1.01108728289694,-5.15002927370416));
#35729=CARTESIAN_POINT('Ctrl Pts',(97.4803584949022,-1.04961042417723,-5.15303405251861));
#35730=CARTESIAN_POINT('Ctrl Pts',(97.4407514971667,-1.0880954531915,-5.15603585860223));
#35731=CARTESIAN_POINT('Ctrl Pts',(97.3989184264822,-1.12437895242778,-5.15903766468585));
#35732=CARTESIAN_POINT('Ctrl Pts',(97.3551360718413,-1.15819880081371,-5.16203947076947));
#35733=CARTESIAN_POINT('Ctrl Pts',(97.3113797396159,-1.1919985480846,-5.16503949270407));
#35734=CARTESIAN_POINT('Ctrl Pts',(97.2656768369141,-1.22333722462856,-5.16803951463867));
#35735=CARTESIAN_POINT('Ctrl Pts',(97.2183376270859,-1.25199261433733,-5.17103953657327));
#35736=CARTESIAN_POINT('Ctrl Pts',(97.1710078569822,-1.28064228998816,-5.17403896028536));
#35737=CARTESIAN_POINT('Ctrl Pts',(97.1220428792877,-1.30660946809164,-5.17703838399745));
#35738=CARTESIAN_POINT('Ctrl Pts',(97.0717803997209,-1.32971622245264,-5.18003780770954));
#35739=CARTESIAN_POINT('Ctrl Pts',(97.0214717110841,-1.35284422012752,-5.1830399889573));
#35740=CARTESIAN_POINT('Ctrl Pts',(96.9698636182559,-1.37310631910399,-5.18604217020506));
#35741=CARTESIAN_POINT('Ctrl Pts',(96.9173154446751,-1.39037207037847,-5.18904435145282));
#35742=CARTESIAN_POINT('Ctrl Pts',(96.8647433523321,-1.40764568063965,-5.19204789922684));
#35743=CARTESIAN_POINT('Ctrl Pts',(96.811230837403,-1.42192008806378,-5.19505144700086));
#35744=CARTESIAN_POINT('Ctrl Pts',(96.7571508966418,-1.43311520559533,-5.19805499477488));
#35745=CARTESIAN_POINT('Ctrl Pts',(96.7029688890938,-1.44433145202716,-5.20106421123985));
#35746=CARTESIAN_POINT('Ctrl Pts',(96.6482178400595,-1.45245672119454,-5.20407342770482));
#35747=CARTESIAN_POINT('Ctrl Pts',(96.5932782502903,-1.4574625645015,-5.20708264416979));
#35748=CARTESIAN_POINT('Ctrl Pts',(96.551247212515,-1.46129223978694,-5.2093848180929));
#35749=CARTESIAN_POINT('Ctrl Pts',(96.5091059960939,-1.46329722506164,-5.211686992016));
#35750=CARTESIAN_POINT('Ctrl Pts',(96.4670241874073,-1.46348537267671,-5.21398916593911));
#35751=CARTESIAN_POINT('Ctrl Pts',(96.4120015598063,-1.46373137864655,-5.21699929460035));
#35752=CARTESIAN_POINT('Ctrl Pts',(96.3568494308675,-1.46087056035062,-5.22000942326159));
#35753=CARTESIAN_POINT('Ctrl Pts',(96.3019472842361,-1.45488808055932,-5.22301955192283));
#35754=CARTESIAN_POINT('Ctrl Pts',(96.2471427141891,-1.44891623332029,-5.22602433073727));
#35755=CARTESIAN_POINT('Ctrl Pts',(96.192587765517,-1.43983379151764,-5.22902910955171));
#35756=CARTESIAN_POINT('Ctrl Pts',(96.138661058349,-1.42767790751627,-5.23203388836616));
#35757=CARTESIAN_POINT('Ctrl Pts',(96.0847877027236,-1.41553404974821,-5.23503569444978));
#35758=CARTESIAN_POINT('Ctrl Pts',(96.0315418700161,-1.4003228887468,-5.2380375005334));
#35759=CARTESIAN_POINT('Ctrl Pts',(95.9792943300983,-1.38213302081769,-5.24103930661701));
#35760=CARTESIAN_POINT('Ctrl Pts',(95.9270778439509,-1.36395396419155,-5.24403932855161));
#35761=CARTESIAN_POINT('Ctrl Pts',(95.8758589723052,-1.34279988301956,-5.24703935048621));
#35762=CARTESIAN_POINT('Ctrl Pts',(95.8259933538087,-1.31880921319808,-5.25003937242081));
#35763=CARTESIAN_POINT('Ctrl Pts',(95.776137678818,-1.29482332726122,-5.25303879613289));
#35764=CARTESIAN_POINT('Ctrl Pts',(95.7276351967086,-1.26800220482933,-5.25603821984498));
#35765=CARTESIAN_POINT('Ctrl Pts',(95.6808194465364,-1.23853146535586,-5.25903764355707));
#35766=CARTESIAN_POINT('Ctrl Pts',(95.6339606560627,-1.20903363180593,-5.26203982480482));
#35767=CARTESIAN_POINT('Ctrl Pts',(95.5887921435294,-1.17688159647649,-5.26504200605258));
#35768=CARTESIAN_POINT('Ctrl Pts',(95.5456194964042,-1.14230502559454,-5.26804418730034));
#35769=CARTESIAN_POINT('Ctrl Pts',(95.5024271980484,-1.10771271622507,-5.27104773507436));
#35770=CARTESIAN_POINT('Ctrl Pts',(95.4612329695767,-1.07069402497377,-5.27405128284838));
#35771=CARTESIAN_POINT('Ctrl Pts',(95.4223076900156,-1.03151758740778,-5.27705483062239));
#35772=CARTESIAN_POINT('Ctrl Pts',(95.3833089455401,-0.992267210909005,
-5.28006404708736));
#35773=CARTESIAN_POINT('Ctrl Pts',(95.3465880556767,-0.950851349007679,
-5.28307326355232));
#35774=CARTESIAN_POINT('Ctrl Pts',(95.3123767510069,-0.907573137122142,
-5.28608248001729));
#35775=CARTESIAN_POINT('Ctrl Pts',(95.2862037008445,-0.874463531348529,
-5.28838465394042));
#35776=CARTESIAN_POINT('Ctrl Pts',(95.2614986764943,-0.840264644534928,
-5.29068682786355));
#35777=CARTESIAN_POINT('Ctrl Pts',(95.2383477627335,-0.805122800332843,
-5.29298900178667));
#35778=CARTESIAN_POINT('Ctrl Pts',(95.2080775783894,-0.759174285592585,
-5.29599913044791));
#35779=CARTESIAN_POINT('Ctrl Pts',(95.1803386839591,-0.711419753414071,
-5.29900925910915));
#35780=CARTESIAN_POINT('Ctrl Pts',(95.1553508543956,-0.662168924559175,
-5.30201938777039));
#35781=CARTESIAN_POINT('Ctrl Pts',(95.1304074352461,-0.613005628304544,
-5.30502416658483));
#35782=CARTESIAN_POINT('Ctrl Pts',(95.1082056148983,-0.562351780010962,
-5.30802894539927));
#35783=CARTESIAN_POINT('Ctrl Pts',(95.0889211537989,-0.510544784132586,
-5.31103372421372));
#35784=CARTESIAN_POINT('Ctrl Pts',(95.0696557714787,-0.458789042693585,
-5.31403553029734));
#35785=CARTESIAN_POINT('Ctrl Pts',(95.0533022142256,-0.405882906141247,
-5.31703733638096));
#35786=CARTESIAN_POINT('Ctrl Pts',(95.0399888674516,-0.35218531289517,-5.32003914246458));
#35787=CARTESIAN_POINT('Ctrl Pts',(95.0266834335787,-0.298519635271133,
-5.32303916439918));
#35788=CARTESIAN_POINT('Ctrl Pts',(95.016414755477,-0.244063944907904,-5.32603918633378));
#35789=CARTESIAN_POINT('Ctrl Pts',(95.0092612089185,-0.189191739574413,
-5.32903920826838));
#35790=CARTESIAN_POINT('Ctrl Pts',(95.0021090888205,-0.134330476090436,
-5.33203863198046));
#35791=CARTESIAN_POINT('Ctrl Pts',(94.9980709348699,-0.0790533859721265,
-5.33503805569255));
#35792=CARTESIAN_POINT('Ctrl Pts',(94.9971735302096,-0.0237412388959985,
-5.33803747940464));
#35793=CARTESIAN_POINT('Ctrl Pts',(94.9962753005157,0.0316217596880619,
-5.3410396606524));
#35794=CARTESIAN_POINT('Ctrl Pts',(94.9985235974758,0.0870193504396207,
-5.34404184190015));
#35795=CARTESIAN_POINT('Ctrl Pts',(95.0038930412365,0.142070106905398,-5.34704402314791));
#35796=CARTESIAN_POINT('Ctrl Pts',(95.0092649290487,0.19714592125349,-5.35004757092193));
#35797=CARTESIAN_POINT('Ctrl Pts',(95.0177607145291,0.251874063834909,-5.35305111869595));
#35798=CARTESIAN_POINT('Ctrl Pts',(95.0293034153971,0.305880884755493,-5.35605466646997));
#35799=CARTESIAN_POINT('Ctrl Pts',(95.0408679011704,0.359989634461566,-5.35906388293494));
#35800=CARTESIAN_POINT('Ctrl Pts',(95.055490650066,0.413373832349386,-5.3620730993999));
#35801=CARTESIAN_POINT('Ctrl Pts',(95.0730443946928,0.465673765817796,-5.36508231586487));
#35802=CARTESIAN_POINT('Ctrl Pts',(95.0864737287415,0.505685358341554,-5.36738448978799));
#35803=CARTESIAN_POINT('Ctrl Pts',(95.1016174885178,0.545062618622844,-5.36968666371111));
#35804=CARTESIAN_POINT('Ctrl Pts',(95.1184001604099,0.58365349767525,-5.37198883763424));
#35805=CARTESIAN_POINT('Ctrl Pts',(95.1403437682178,0.634111679801023,-5.37499896629548));
#35806=CARTESIAN_POINT('Ctrl Pts',(95.1651830511075,0.683436639338107,-5.37800909495672));
#35807=CARTESIAN_POINT('Ctrl Pts',(95.1927786937771,0.731275078639996,-5.38101922361796));
#35808=CARTESIAN_POINT('Ctrl Pts',(95.2203252912141,0.779028495555819,-5.3840240024324));
#35809=CARTESIAN_POINT('Ctrl Pts',(95.2506182649216,0.825300181473522,-5.38702878124685));
#35810=CARTESIAN_POINT('Ctrl Pts',(95.2834710644068,0.86975857581954,-5.3900335600613));
#35811=CARTESIAN_POINT('Ctrl Pts',(95.3162913614897,0.914172985949891,-5.39303536614492));
#35812=CARTESIAN_POINT('Ctrl Pts',(95.3516661552266,0.956777235594734,-5.39603717222854));
#35813=CARTESIAN_POINT('Ctrl Pts',(95.3893649743159,0.997267675972879,-5.39903897831215));
#35814=CARTESIAN_POINT('Ctrl Pts',(95.4270413867909,1.03773405051287,-5.40203900024676));
#35815=CARTESIAN_POINT('Ctrl Pts',(95.4670387276289,1.07608872022583,-5.40503902218136));
#35816=CARTESIAN_POINT('Ctrl Pts',(95.5090870066105,1.11206196557865,-5.40803904411596));
#35817=CARTESIAN_POINT('Ctrl Pts',(95.5511269009111,1.14802803764882,-5.41103846782805));
#35818=CARTESIAN_POINT('Ctrl Pts',(95.5952165200877,1.18161328530521,-5.41403789154014));
#35819=CARTESIAN_POINT('Ctrl Pts',(95.6410515934928,1.21258722588828,-5.41703731525223));
#35820=CARTESIAN_POINT('Ctrl Pts',(95.6869288056093,1.24358964252351,-5.42003949649999));
#35821=CARTESIAN_POINT('Ctrl Pts',(95.7345542394087,1.27197565942828,-5.42304167774775));
#35822=CARTESIAN_POINT('Ctrl Pts',(95.7835945725189,1.2975581229961,-5.42604385899551));
#35823=CARTESIAN_POINT('Ctrl Pts',(95.8326572277,1.3231522311334,-5.42904740676953));
#35824=CARTESIAN_POINT('Ctrl Pts',(95.8831355838423,1.34594002441192,-5.43205095454354));
#35825=CARTESIAN_POINT('Ctrl Pts',(95.9346746362876,1.36578181672804,-5.43505450231756));
#35826=CARTESIAN_POINT('Ctrl Pts',(95.9863109600207,1.38566105708795,-5.43806371878253));
#35827=CARTESIAN_POINT('Ctrl Pts',(96.0390114750706,1.40258302750693,-5.44107293524749));
#35828=CARTESIAN_POINT('Ctrl Pts',(96.0924053740501,1.41645777229698,-5.44408215171246));
#35829=CARTESIAN_POINT('Ctrl Pts',(96.133253895024,1.42707252069326,-5.44638432563558));
#35830=CARTESIAN_POINT('Ctrl Pts',(96.1745079011604,1.43590479475527,-5.44868649955869));
#35831=CARTESIAN_POINT('Ctrl Pts',(96.2159987870002,1.44293476019596,-5.45098867348181));
#35832=CARTESIAN_POINT('Ctrl Pts',(96.2702487736725,1.45212655072404,-5.45399880214304));
#35833=CARTESIAN_POINT('Ctrl Pts',(96.3251318414259,1.45827394706615,-5.45700893080428));
#35834=CARTESIAN_POINT('Ctrl Pts',(96.380275972639,1.46130058908986,-5.46001905946552));
#35835=CARTESIAN_POINT('Ctrl Pts',(96.435322097193,1.46432185191788,-5.46302383827997));
#35836=CARTESIAN_POINT('Ctrl Pts',(96.4906278413713,1.46423333870561,-5.46602861709441));
#35837=CARTESIAN_POINT('Ctrl Pts',(96.5458135838134,1.46101012711558,-5.46903339590885));
#35838=CARTESIAN_POINT('Ctrl Pts',(96.6009447291061,1.45779010435941,-5.47203520199247));
#35839=CARTESIAN_POINT('Ctrl Pts',(96.6559555832192,1.45144155732333,-5.47503700807609));
#35840=CARTESIAN_POINT('Ctrl Pts',(96.710465903512,1.44199159942286,-5.47803881415971));
#35841=CARTESIAN_POINT('Ctrl Pts',(96.7649438251316,1.43254725818537,-5.48103883609431));
#35842=CARTESIAN_POINT('Ctrl Pts',(96.8189212832728,1.42000524975318,-5.48403885802891));
#35843=CARTESIAN_POINT('Ctrl Pts',(96.8720248589717,1.40444432450706,-5.48703887996351));
#35844=CARTESIAN_POINT('Ctrl Pts',(96.9251178454966,1.38888650220354,-5.4900383036756));
#35845=CARTESIAN_POINT('Ctrl Pts',(96.9773367891258,1.37031110703871,-5.49303772738769));
#35846=CARTESIAN_POINT('Ctrl Pts',(97.0283224021416,1.34884703904829,-5.49603715109977));
#35847=CARTESIAN_POINT('Ctrl Pts',(97.0793548890439,1.32736323795619,-5.49903933234753));
#35848=CARTESIAN_POINT('Ctrl Pts',(97.1291512922216,1.30298566361309,-5.50204151359529));
#35849=CARTESIAN_POINT('Ctrl Pts',(97.1773727394569,1.2758912224805,-5.50504369484304));
#35850=CARTESIAN_POINT('Ctrl Pts',(97.2256161360245,1.24878444855975,-5.50804724261706));
#35851=CARTESIAN_POINT('Ctrl Pts',(97.2722827018194,1.218958627561,-5.51105079039108));
#35852=CARTESIAN_POINT('Ctrl Pts',(97.3170614728188,1.18663476150111,-5.5140543381651));
#35853=CARTESIAN_POINT('Ctrl Pts',(97.3619247562125,1.15424988958391,-5.51706355463006));
#35854=CARTESIAN_POINT('Ctrl Pts',(97.4048927163997,1.11935788811173,-5.52007277109503));
#35855=CARTESIAN_POINT('Ctrl Pts',(97.4456874053701,1.08222016681613,-5.52308198755999));
#35856=CARTESIAN_POINT('Ctrl Pts',(97.4768970143308,1.05380828800104,-5.52538416148312));
#35857=CARTESIAN_POINT('Ctrl Pts',(97.506835308566,1.02408286747054,-5.52768633540624));
#35858=CARTESIAN_POINT('Ctrl Pts',(97.5353935509653,0.993174279457849,-5.52998850932936));
#35859=CARTESIAN_POINT('Ctrl Pts',(97.5722927650602,0.953238257117894,-5.5329630764363));
#35860=CARTESIAN_POINT('Ctrl Pts',(97.6070498726323,0.911149160200333,-5.53593764354323));
#35861=CARTESIAN_POINT('Ctrl Pts',(97.6394002965644,0.867168624489368,-5.53891221065017));
#35862=CARTESIAN_POINT('Ctrl Pts',(97.6717038201296,0.823251850021986,-5.54188246534719));
#35863=CARTESIAN_POINT('Ctrl Pts',(97.7016072483117,0.777449496312327,-5.54485272004423));
#35864=CARTESIAN_POINT('Ctrl Pts',(97.7288843008441,0.730058345952218,-5.54782297474125));
#35865=CARTESIAN_POINT('Ctrl Pts',(97.7561332027838,0.682716104430883,-5.550790164062));
#35866=CARTESIAN_POINT('Ctrl Pts',(97.7807608285218,0.633788780753312,-5.55375735338275));
#35867=CARTESIAN_POINT('Ctrl Pts',(97.8025839793593,0.583602353875609,-5.5567245427035));
#35868=CARTESIAN_POINT('Ctrl Pts',(97.8244001929085,0.533431880593121,-5.55969078879438));
#35869=CARTESIAN_POINT('Ctrl Pts',(97.8434134677593,0.482003586648015,-5.56265703488525));
#35870=CARTESIAN_POINT('Ctrl Pts',(97.8594874089156,0.429666355128056,-5.56562328097612));
#35871=CARTESIAN_POINT('Ctrl Pts',(97.8755578133273,0.377340639353834,-5.56858887440473));
#35872=CARTESIAN_POINT('Ctrl Pts',(97.8886900146702,0.324106902664976,-5.57155446783335));
#35873=CARTESIAN_POINT('Ctrl Pts',(97.8987973994405,0.270329502740709,-5.57452006126196));
#35874=CARTESIAN_POINT('Ctrl Pts',(97.9089129448949,0.21650868304136,-5.57748804910532));
#35875=CARTESIAN_POINT('Ctrl Pts',(97.9159987049772,0.162143858228707,-5.58045603694869));
#35876=CARTESIAN_POINT('Ctrl Pts',(97.9200194895277,0.107608087050669,-5.58342402479205));
#35877=CARTESIAN_POINT('Ctrl Pts',(97.9226932180571,0.0713430632866484,
-5.58539766791373));
#35878=CARTESIAN_POINT('Ctrl Pts',(97.9240127055925,0.0350025971491351,
-5.5873713110354));
#35879=CARTESIAN_POINT('Ctrl Pts',(97.9239803690938,-0.00130348536077301,
-5.58934495415708));
#35880=CARTESIAN_POINT('Origin',(96.460480949577,-8.32667268468867E-16,
1.18130019239114E-14));
#35881=CARTESIAN_POINT('',(97.9239808258401,0.000601812115854682,-6.16065504587429));
#35882=CARTESIAN_POINT('',(97.923980796324,0.000669754741461998,-6.08934495418968));
#35883=CARTESIAN_POINT('',(97.923980949577,-1.01189432752408E-15,1.19922289829666E-14));
#35884=CARTESIAN_POINT('Ctrl Pts',(97.9239808258399,0.000601812690350752,
-6.16065504584289));
#35885=CARTESIAN_POINT('Ctrl Pts',(97.9239666682132,0.0350306063101608,
-6.15877304002328));
#35886=CARTESIAN_POINT('Ctrl Pts',(97.922737702697,0.0694328740323531,-6.15689103420366));
#35887=CARTESIAN_POINT('Ctrl Pts',(97.9202989417931,0.103748154692315,-6.15500902838404));
#35888=CARTESIAN_POINT('Ctrl Pts',(97.9163983246865,0.158632899870198,-6.1519988997228));
#35889=CARTESIAN_POINT('Ctrl Pts',(97.9093899575706,0.21341268079498,-6.14898877106156));
#35890=CARTESIAN_POINT('Ctrl Pts',(97.8992876392723,0.267707974644227,-6.14597864240033));
#35891=CARTESIAN_POINT('Ctrl Pts',(97.8892032756401,0.321906770457557,-6.14297386358588));
#35892=CARTESIAN_POINT('Ctrl Pts',(97.8760359690999,0.375622272988754,-6.13996908477144));
#35893=CARTESIAN_POINT('Ctrl Pts',(97.8598512952113,0.428479737863195,-6.13696430595699));
#35894=CARTESIAN_POINT('Ctrl Pts',(97.8436826333761,0.481284909033203,-6.13396249987338));
#35895=CARTESIAN_POINT('Ctrl Pts',(97.8245026715609,0.533233221657217,-6.13096069378976));
#35896=CARTESIAN_POINT('Ctrl Pts',(97.8024276915079,0.583961635572912,-6.12795888770614));
#35897=CARTESIAN_POINT('Ctrl Pts',(97.7803658319074,0.634659898623632,-6.12495886577155));
#35898=CARTESIAN_POINT('Ctrl Pts',(97.7554125748742,0.684139216791161,-6.12195884383695));
#35899=CARTESIAN_POINT('Ctrl Pts',(97.7277327599278,0.732055393506915,-6.11895882190236));
#35900=CARTESIAN_POINT('Ctrl Pts',(97.7000584645039,0.779962015447368,-6.11595939819027));
#35901=CARTESIAN_POINT('Ctrl Pts',(97.6696589549361,0.826305657916654,-6.11295997447818));
#35902=CARTESIAN_POINT('Ctrl Pts',(97.6367444549757,0.870767716367136,-6.1099605507661));
#35903=CARTESIAN_POINT('Ctrl Pts',(97.6037996948998,0.915270651240504,-6.10695836951834));
#35904=CARTESIAN_POINT('Ctrl Pts',(97.5683356399163,0.957888120715072,-6.10395618827059));
#35905=CARTESIAN_POINT('Ctrl Pts',(97.5306043291967,0.998332711269761,-6.10095400702284));
#35906=CARTESIAN_POINT('Ctrl Pts',(97.4928558440221,1.03879571130427,-6.09795045924882));
#35907=CARTESIAN_POINT('Ctrl Pts',(97.4528384281371,1.07708349508994,-6.09494691147481));
#35908=CARTESIAN_POINT('Ctrl Pts',(97.4108403640097,1.11294619519502,-6.0919433637008));
#35909=CARTESIAN_POINT('Ctrl Pts',(97.3687630356043,1.14887658011109,-6.08893414723584));
#35910=CARTESIAN_POINT('Ctrl Pts',(97.3246980129091,1.18237241782646,-6.08592493077087));
#35911=CARTESIAN_POINT('Ctrl Pts',(97.2789650303539,1.21322547760701,-6.08291571430591));
#35912=CARTESIAN_POINT('Ctrl Pts',(97.2439774244133,1.23682933279751,-6.08061354038278));
#35913=CARTESIAN_POINT('Ctrl Pts',(97.2080142489618,1.2588872587856,-6.07831136645964));
#35914=CARTESIAN_POINT('Ctrl Pts',(97.1712278981197,1.27932444092076,-6.0760091925365));
#35915=CARTESIAN_POINT('Ctrl Pts',(97.1231291650486,1.30604637842591,-6.07299906387526));
#35916=CARTESIAN_POINT('Ctrl Pts',(97.073420279959,1.33010813960371,-6.06998893521401));
#35917=CARTESIAN_POINT('Ctrl Pts',(97.0224266430538,1.35131391156271,-6.06697880655277));
#35918=CARTESIAN_POINT('Ctrl Pts',(96.9715236362098,1.3724819948898,-6.06397402773831));
#35919=CARTESIAN_POINT('Ctrl Pts',(96.9193408925939,1.3908039610083,-6.06096924892386));
#35920=CARTESIAN_POINT('Ctrl Pts',(96.8662281009337,1.40612997235885,-6.05796447010941));
#35921=CARTESIAN_POINT('Ctrl Pts',(96.8131678555815,1.42144082116029,-6.05496266402578));
#35922=CARTESIAN_POINT('Ctrl Pts',(96.7591798898342,1.43376144103961,-6.05196085794215));
#35923=CARTESIAN_POINT('Ctrl Pts',(96.7046317954859,1.44299085736604,-6.04895905185852));
#35924=CARTESIAN_POINT('Ctrl Pts',(96.6501161222621,1.45221478811025,-6.04595902992391));
#35925=CARTESIAN_POINT('Ctrl Pts',(96.5950414999767,1.45835106898945,-6.04295900798931));
#35926=CARTESIAN_POINT('Ctrl Pts',(96.5397862701856,1.46134968988369,-6.0399589860547));
#35927=CARTESIAN_POINT('Ctrl Pts',(96.4845420586212,1.46434771283481,-6.03695956234259));
#35928=CARTESIAN_POINT('Ctrl Pts',(96.4291178381183,1.46420928974957,-6.03396013863049));
#35929=CARTESIAN_POINT('Ctrl Pts',(96.3738953139924,1.46093640440315,-6.03096071491839));
#35930=CARTESIAN_POINT('Ctrl Pts',(96.3186220207541,1.4576605101127,-6.02795853367062));
#35931=CARTESIAN_POINT('Ctrl Pts',(96.2635513226828,1.45124442764307,-6.02495635242285));
#35932=CARTESIAN_POINT('Ctrl Pts',(96.2090616495517,1.44174220496412,-6.02195417117508));
#35933=CARTESIAN_POINT('Ctrl Pts',(96.154547173931,1.43223565708433,-6.01895062340105));
#35934=CARTESIAN_POINT('Ctrl Pts',(96.1006147656269,1.4196402890516,-6.01594707562702));
#35935=CARTESIAN_POINT('Ctrl Pts',(96.0476312117472,1.40406101860775,-6.01294352785299));
#35936=CARTESIAN_POINT('Ctrl Pts',(95.9945476603262,1.38845234491283,-6.00993431138801));
#35937=CARTESIAN_POINT('Ctrl Pts',(95.9424170393497,1.36984869672209,-6.00692509492304));
#35938=CARTESIAN_POINT('Ctrl Pts',(95.8915884492988,1.34840408376983,-6.00391587845806));
#35939=CARTESIAN_POINT('Ctrl Pts',(95.8527024947912,1.33199807599234,-6.00161370453501));
#35940=CARTESIAN_POINT('Ctrl Pts',(95.814578250245,1.31393031284668,-5.99931153061197));
#35941=CARTESIAN_POINT('Ctrl Pts',(95.7773616424926,1.29428755007862,-5.99700935668892));
#35942=CARTESIAN_POINT('Ctrl Pts',(95.7287003417334,1.26860432840625,-5.99399922802769));
#35943=CARTESIAN_POINT('Ctrl Pts',(95.6813872294994,1.24011905118213,-5.99098909936645));
#35944=CARTESIAN_POINT('Ctrl Pts',(95.6357641017506,1.2089972584383,-5.98797897070522));
#35945=CARTESIAN_POINT('Ctrl Pts',(95.590222059155,1.17793077788934,-5.98497419189078));
#35946=CARTESIAN_POINT('Ctrl Pts',(95.5463644731706,1.14423737608251,-5.98196941307634));
#35947=CARTESIAN_POINT('Ctrl Pts',(95.5045079053338,1.10812805608397,-5.9789646342619));
#35948=CARTESIAN_POINT('Ctrl Pts',(95.4626927476364,1.07205446027521,-5.97596282817829));
#35949=CARTESIAN_POINT('Ctrl Pts',(95.4228750843551,1.03357002432336,-5.97296102209467));
#35950=CARTESIAN_POINT('Ctrl Pts',(95.3853403351739,0.992927444106999,-5.96995921601105));
#35951=CARTESIAN_POINT('Ctrl Pts',(95.3478278950906,0.952309020154461,-5.96695919407646));
#35952=CARTESIAN_POINT('Ctrl Pts',(95.312596037294,0.909535381554504,-5.96395917214186));
#35953=CARTESIAN_POINT('Ctrl Pts',(95.2798933709462,0.864896074209275,-5.96095915020727));
#35954=CARTESIAN_POINT('Ctrl Pts',(95.2471972257077,0.820265668211757,-5.95795972649518));
#35955=CARTESIAN_POINT('Ctrl Pts',(95.2170295822583,0.773770758081859,-5.9549603027831));
#35956=CARTESIAN_POINT('Ctrl Pts',(95.1895973414188,0.725732116221149,-5.95196087907101));
#35957=CARTESIAN_POINT('Ctrl Pts',(95.1621398806071,0.677649309787143,-5.94895869782326));
#35958=CARTESIAN_POINT('Ctrl Pts',(95.1374231091112,0.62802039576409,-5.9459565165755));
#35959=CARTESIAN_POINT('Ctrl Pts',(95.1156085328441,0.577191850870175,-5.94295433532775));
#35960=CARTESIAN_POINT('Ctrl Pts',(95.0937840270661,0.526340169950935,-5.93995078755373));
#35961=CARTESIAN_POINT('Ctrl Pts',(95.0748645305922,0.474288266868446,-5.93694723977972));
#35962=CARTESIAN_POINT('Ctrl Pts',(95.0589625830258,0.421400662338995,-5.9339436920057));
#35963=CARTESIAN_POINT('Ctrl Pts',(95.0430306232096,0.368413241356617,-5.93093447554074));
#35964=CARTESIAN_POINT('Ctrl Pts',(95.0301277125911,0.314587482960157,-5.92792525907578));
#35965=CARTESIAN_POINT('Ctrl Pts',(95.0203156110056,0.260299918512206,-5.92491604261082));
#35966=CARTESIAN_POINT('Ctrl Pts',(95.0128089511609,0.218767706829014,-5.92261386868767));
#35967=CARTESIAN_POINT('Ctrl Pts',(95.0071102514927,0.176965471128548,-5.92031169476452));
#35968=CARTESIAN_POINT('Ctrl Pts',(95.0032265855773,0.135062832059204,-5.91800952084137));
#35969=CARTESIAN_POINT('Ctrl Pts',(94.9981486312295,0.0802744715553483,
-5.91499939218014));
#35970=CARTESIAN_POINT('Ctrl Pts',(94.9961541187356,0.0250842230714438,
-5.9119892635189));
#35971=CARTESIAN_POINT('Ctrl Pts',(94.9972911598343,-0.0301311996537504,
-5.90897913485766));
#35972=CARTESIAN_POINT('Ctrl Pts',(94.9984261800905,-0.0852484890147449,
-5.90597435604322));
#35973=CARTESIAN_POINT('Ctrl Pts',(95.0026816980782,-0.140390340093219,
-5.90296957722878));
#35974=CARTESIAN_POINT('Ctrl Pts',(95.0100539610316,-0.195176332835741,
-5.89996479841433));
#35975=CARTESIAN_POINT('Ctrl Pts',(95.0174189303522,-0.249908123915031,
-5.89696299233071));
#35976=CARTESIAN_POINT('Ctrl Pts',(95.027894466283,-0.304284233252548,-5.8939611862471));
#35977=CARTESIAN_POINT('Ctrl Pts',(95.0414248814198,-0.357927542145374,
-5.89095938016348));
#35978=CARTESIAN_POINT('Ctrl Pts',(95.0549472546391,-0.411538967680527,
-5.88795935822888));
#35979=CARTESIAN_POINT('Ctrl Pts',(95.0715207793374,-0.464417944996317,
-5.88495933629428));
#35980=CARTESIAN_POINT('Ctrl Pts',(95.0910387920996,-0.516198050484219,
-5.88195931435968));
#35981=CARTESIAN_POINT('Ctrl Pts',(95.1105529128521,-0.567967830706091,
-5.87895989064759));
#35982=CARTESIAN_POINT('Ctrl Pts',(95.1330101694463,-0.61863868036885,-5.8759604669355));
#35983=CARTESIAN_POINT('Ctrl Pts',(95.1582549561594,-0.667862045685692,
-5.87296104322341));
#35984=CARTESIAN_POINT('Ctrl Pts',(95.1835229517974,-0.717130664757451,
-5.86995886197565));
#35985=CARTESIAN_POINT('Ctrl Pts',(95.2115833560347,-0.764948669884523,
-5.86695668072789));
#35986=CARTESIAN_POINT('Ctrl Pts',(95.2422342314922,-0.810991481999388,
-5.86395449948013));
#35987=CARTESIAN_POINT('Ctrl Pts',(95.2728990585477,-0.857055251780253,
-5.86095095170611));
#35988=CARTESIAN_POINT('Ctrl Pts',(95.3061563896463,-0.901341794764974,
-5.85794740393209));
#35989=CARTESIAN_POINT('Ctrl Pts',(95.3417624200753,-0.943557683318552,
-5.85494385615807));
#35990=CARTESIAN_POINT('Ctrl Pts',(95.3774356508944,-0.985853247257124,
-5.85193463969311));
#35991=CARTESIAN_POINT('Ctrl Pts',(95.4154660724507,-1.02606996524403,-5.84892542322814));
#35992=CARTESIAN_POINT('Ctrl Pts',(95.455572074926,-1.06395037649674,-5.84591620676318));
#35993=CARTESIAN_POINT('Ctrl Pts',(95.4862548104933,-1.09293044356687,-5.84361403284005));
#35994=CARTESIAN_POINT('Ctrl Pts',(95.5181515607852,-1.12054383539475,-5.84131185891693));
#35995=CARTESIAN_POINT('Ctrl Pts',(95.5511241289182,-1.14669194761334,-5.8390096849938));
#35996=CARTESIAN_POINT('Ctrl Pts',(95.5942362810344,-1.1808810161437,-5.83599955633256));
#35997=CARTESIAN_POINT('Ctrl Pts',(95.6393698056744,-1.21270720915158,-5.83298942767132));
#35998=CARTESIAN_POINT('Ctrl Pts',(95.6862354830088,-1.24192439685297,-5.82997929901008));
#35999=CARTESIAN_POINT('Ctrl Pts',(95.7330178668292,-1.2710896573793,-5.82697452019564));
#36000=CARTESIAN_POINT('Ctrl Pts',(95.7815258494597,-1.29765483749976,-5.82396974138119));
#36001=CARTESIAN_POINT('Ctrl Pts',(95.8314387683707,-1.32141522023292,-5.82096496256675));
#36002=CARTESIAN_POINT('Ctrl Pts',(95.8813023067177,-1.34515209600382,-5.81796315648312));
#36003=CARTESIAN_POINT('Ctrl Pts',(95.9325675534184,-1.36608944541675,-5.81496135039951));
#36004=CARTESIAN_POINT('Ctrl Pts',(95.9848882340308,-1.38406785199259,-5.81195954431588));
#36005=CARTESIAN_POINT('Ctrl Pts',(96.0371778174009,-1.40203557294931,-5.80895952238128));
#36006=CARTESIAN_POINT('Ctrl Pts',(96.0905210928655,-1.41704766559509,-5.80595950044668));
#36007=CARTESIAN_POINT('Ctrl Pts',(96.1445528903195,-1.42899325098958,-5.80295947851208));
#36008=CARTESIAN_POINT('Ctrl Pts',(96.1985739135064,-1.44093645436212,-5.79996005479999));
#36009=CARTESIAN_POINT('Ctrl Pts',(96.253282670645,-1.44981425091524,-5.7969606310879));
#36010=CARTESIAN_POINT('Ctrl Pts',(96.308302216202,-1.45556651620885,-5.79396120737581));
#36011=CARTESIAN_POINT('Ctrl Pts',(96.3633723442621,-1.46132406987725,-5.79095902612805));
#36012=CARTESIAN_POINT('Ctrl Pts',(96.4187533052,-1.46395029642693,-5.78795684488029));
#36013=CARTESIAN_POINT('Ctrl Pts',(96.4740629175201,-1.46343697511946,-5.78495466363253));
#36014=CARTESIAN_POINT('Ctrl Pts',(96.5293977055478,-1.46292342015952,-5.78195111585851));
#36015=CARTESIAN_POINT('Ctrl Pts',(96.5846605523354,-1.45926750354692,-5.77894756808449));
#36016=CARTESIAN_POINT('Ctrl Pts',(96.6394724904034,-1.45251309058218,-5.77594402031047));
#36017=CARTESIAN_POINT('Ctrl Pts',(96.6943878767801,-1.44574592979969,-5.7729348038455));
#36018=CARTESIAN_POINT('Ctrl Pts',(96.7488501334898,-1.43586868506862,-5.76992558738053));
#36019=CARTESIAN_POINT('Ctrl Pts',(96.802489759699,-1.42297653662981,-5.76691637091556));
#36020=CARTESIAN_POINT('Ctrl Pts',(96.8435262720741,-1.41311351471224,-5.76461419699245));
#36021=CARTESIAN_POINT('Ctrl Pts',(96.8840814900324,-1.40148697680278,-5.76231202306935));
#36022=CARTESIAN_POINT('Ctrl Pts',(96.923997319528,-1.38815878947168,-5.76000984914624));
#36023=CARTESIAN_POINT('Ctrl Pts',(96.976187895225,-1.3707319746316,-5.756999720485));
#36024=CARTESIAN_POINT('Ctrl Pts',(97.027503969092,-1.350321139992,-5.75398959182376));
#36025=CARTESIAN_POINT('Ctrl Pts',(97.0775813722312,-1.32703403059606,-5.75097946316252));
#36026=CARTESIAN_POINT('Ctrl Pts',(97.1275697737147,-1.30378830895512,-5.74797468434808));
#36027=CARTESIAN_POINT('Ctrl Pts',(97.1763233982983,-1.27767667814301,-5.74496990553364));
#36028=CARTESIAN_POINT('Ctrl Pts',(97.2234955812531,-1.2488558451031,-5.74196512671919));
#36029=CARTESIAN_POINT('Ctrl Pts',(97.2706210951481,-1.22006352550264,-5.73896332063557));
#36030=CARTESIAN_POINT('Ctrl Pts',(97.3161678183167,-1.18856758721968,-5.73596151455196));
#36031=CARTESIAN_POINT('Ctrl Pts',(97.3598130321715,-1.15457093988038,-5.73295970846834));
#36032=CARTESIAN_POINT('Ctrl Pts',(97.4034323051216,-1.12059449873807,-5.72995968653374));
#36033=CARTESIAN_POINT('Ctrl Pts',(97.4451518930407,-1.08412061840226,-5.72695966459914));
#36034=CARTESIAN_POINT('Ctrl Pts',(97.4846794043202,-1.04539455484597,-5.72395964266454));
#36035=CARTESIAN_POINT('Ctrl Pts',(97.5241990335751,-1.00667621350084,-5.72096021895246));
#36036=CARTESIAN_POINT('Ctrl Pts',(97.561527077251,-0.965706950209761,-5.71796079524037));
#36037=CARTESIAN_POINT('Ctrl Pts',(97.5964072179516,-0.922769615243472,
-5.71496137152828));
#36038=CARTESIAN_POINT('Ctrl Pts',(97.6313194258896,-0.879792805616685,
-5.71195919028052));
#36039=CARTESIAN_POINT('Ctrl Pts',(97.6637789009566,-0.834844720244027,
-5.70895700903276));
#36040=CARTESIAN_POINT('Ctrl Pts',(97.6935699355941,-0.788240954634579,
-5.705954827785));
#36041=CARTESIAN_POINT('Ctrl Pts',(97.7233745304493,-0.741615976025545,
-5.70295128001098));
#36042=CARTESIAN_POINT('Ctrl Pts',(97.7505080044389,-0.69333427607002,-5.69994773223696));
#36043=CARTESIAN_POINT('Ctrl Pts',(97.7748000295898,-0.643737218059023,
-5.69694418446294));
#36044=CARTESIAN_POINT('Ctrl Pts',(97.7991379018499,-0.594046553947895,
-5.69393496799798));
#36045=CARTESIAN_POINT('Ctrl Pts',(97.8206234068304,-0.543036060467411,
-5.69092575153301));
#36046=CARTESIAN_POINT('Ctrl Pts',(97.8391343667395,-0.491067210619997,
-5.68791653506804));
#36047=CARTESIAN_POINT('Ctrl Pts',(97.853296009709,-0.451308910635165,-5.68561436114492));
#36048=CARTESIAN_POINT('Ctrl Pts',(97.8657176831939,-0.41099012946238,-5.6833121872218));
#36049=CARTESIAN_POINT('Ctrl Pts',(97.8763648201458,-0.370277078770926,
-5.68101001329868));
#36050=CARTESIAN_POINT('Ctrl Pts',(97.8941165227751,-0.302397237243981,
-5.67717165684012));
#36051=CARTESIAN_POINT('Ctrl Pts',(97.9069947864868,-0.233194083262063,
-5.67333330038157));
#36052=CARTESIAN_POINT('Ctrl Pts',(97.9148439409853,-0.163280553715951,
-5.66949494392301));
#36053=CARTESIAN_POINT('Ctrl Pts',(97.9208695864408,-0.10960927718987,-5.66654831124361));
#36054=CARTESIAN_POINT('Ctrl Pts',(97.923932276957,-0.055519665670863,-5.66360167856421));
#36055=CARTESIAN_POINT('Ctrl Pts',(97.9239803738018,-0.00129818862390677,
-5.66065504588482));
#36056=CARTESIAN_POINT('Ctrl Pts',(97.9239803690929,-0.00130348633276346,
-5.58934495420992));
#36057=CARTESIAN_POINT('Ctrl Pts',(97.9239165941649,-0.0729072828784039,
-5.59323742430783));
#36058=CARTESIAN_POINT('Ctrl Pts',(97.9185940325572,-0.144280430134909,
-5.59712989440575));
#36059=CARTESIAN_POINT('Ctrl Pts',(97.9081361102898,-0.214771473109514,
-5.60102236450367));
#36060=CARTESIAN_POINT('Ctrl Pts',(97.9010020279403,-0.262858358116362,
-5.60367769139475));
#36061=CARTESIAN_POINT('Ctrl Pts',(97.8914791845124,-0.310535349866628,
-5.60633301828584));
#36062=CARTESIAN_POINT('Ctrl Pts',(97.8796191635676,-0.357601705241597,
-5.60898834517693));
#36063=CARTESIAN_POINT('Ctrl Pts',(97.8661744200639,-0.410957013685808,
-5.61199847383816));
#36064=CARTESIAN_POINT('Ctrl Pts',(97.8496882465437,-0.463665150538308,
-5.6150086024994));
#36065=CARTESIAN_POINT('Ctrl Pts',(97.8302406418319,-0.51535486363633,-5.61801873116064));
#36066=CARTESIAN_POINT('Ctrl Pts',(97.8108276009935,-0.566952709549609,
-5.62102350997508));
#36067=CARTESIAN_POINT('Ctrl Pts',(97.7884637584791,-0.617535233425873,
-5.62402828878952));
#36068=CARTESIAN_POINT('Ctrl Pts',(97.7632792547537,-0.666744948258849,
-5.62703306760397));
#36069=CARTESIAN_POINT('Ctrl Pts',(97.7381196669224,-0.715905978231743,
-5.63003487368758));
#36070=CARTESIAN_POINT('Ctrl Pts',(97.7101451852964,-0.763696421810779,
-5.6330366797712));
#36071=CARTESIAN_POINT('Ctrl Pts',(97.6795338260064,-0.809779188710823,
-5.63603848585482));
#36072=CARTESIAN_POINT('Ctrl Pts',(97.6489406608386,-0.855834565925755,
-5.63903850778942));
#36073=CARTESIAN_POINT('Ctrl Pts',(97.6157140160327,-0.900183839176101,
-5.64203852972402));
#36074=CARTESIAN_POINT('Ctrl Pts',(97.5800764188042,-0.942516968168683,
-5.64503855165861));
#36075=CARTESIAN_POINT('Ctrl Pts',(97.544445927928,-0.984841655679431,-5.6480379753707));
#36076=CARTESIAN_POINT('Ctrl Pts',(97.5064057793194,-1.02515059356064,-5.65103739908279));
#36077=CARTESIAN_POINT('Ctrl Pts',(97.4662187057894,-1.06316688047029,-5.65403682279488));
#36078=CARTESIAN_POINT('Ctrl Pts',(97.4259946860659,-1.10121811784949,-5.65703900404263));
#36079=CARTESIAN_POINT('Ctrl Pts',(97.3836201825292,-1.13697212951688,-5.66004118529039));
#36080=CARTESIAN_POINT('Ctrl Pts',(97.3393936400685,-1.17019004118692,-5.66304336653815));
#36081=CARTESIAN_POINT('Ctrl Pts',(97.2951469666673,-1.20342307291299,-5.66604691431216));
#36082=CARTESIAN_POINT('Ctrl Pts',(97.2490470142228,-1.23411741027274,-5.66905046208618));
#36083=CARTESIAN_POINT('Ctrl Pts',(97.2014213414792,-1.26207748797282,-5.6720540098602));
#36084=CARTESIAN_POINT('Ctrl Pts',(97.1537057832934,-1.29009033561407,-5.67506322632516));
#36085=CARTESIAN_POINT('Ctrl Pts',(97.1044592235074,-1.31535837310478,-5.67807244279013));
#36086=CARTESIAN_POINT('Ctrl Pts',(97.0540329014977,-1.33773253319607,-5.6810816592551));
#36087=CARTESIAN_POINT('Ctrl Pts',(97.0154546985263,-1.35484968263142,-5.68338383317823));
#36088=CARTESIAN_POINT('Ctrl Pts',(96.976186501996,-1.37027404092252,-5.68568600710135));
#36089=CARTESIAN_POINT('Ctrl Pts',(96.9363914464605,-1.38395861533362,-5.68798818102448));
#36090=CARTESIAN_POINT('Ctrl Pts',(96.8843587846187,-1.40185141189338,-5.69099830968572));
#36091=CARTESIAN_POINT('Ctrl Pts',(96.8312063209807,-1.41684331694327,-5.69400843834697));
#36092=CARTESIAN_POINT('Ctrl Pts',(96.7772887002682,-1.42879848092794,-5.69701856700821));
#36093=CARTESIAN_POINT('Ctrl Pts',(96.7234669063601,-1.4407323972176,-5.70002334582266));
#36094=CARTESIAN_POINT('Ctrl Pts',(96.6688831655312,-1.44964016971358,-5.70302812463711));
#36095=CARTESIAN_POINT('Ctrl Pts',(96.6139079910096,-1.45543546506097,-5.70603290345156));
#36096=CARTESIAN_POINT('Ctrl Pts',(96.5589872053152,-1.46122502692374,-5.70903470953518));
#36097=CARTESIAN_POINT('Ctrl Pts',(96.503676275693,-1.46390815645125,-5.71203651561881));
#36098=CARTESIAN_POINT('Ctrl Pts',(96.4483547916438,-1.46344976213527,-5.71503832170243));
#36099=CARTESIAN_POINT('Ctrl Pts',(96.39306618839,-1.46299164026986,-5.71803834363704));
#36100=CARTESIAN_POINT('Ctrl Pts',(96.3377675701865,-1.45939569982411,-5.72103836557164));
#36101=CARTESIAN_POINT('Ctrl Pts',(96.2828401921201,-1.45267890853076,-5.72403838750624));
#36102=CARTESIAN_POINT('Ctrl Pts',(96.2279237669048,-1.4459634566062,-5.72703781121834));
#36103=CARTESIAN_POINT('Ctrl Pts',(96.1733789587284,-1.43612845379516,-5.73003723493044));
#36104=CARTESIAN_POINT('Ctrl Pts',(96.1195812360937,-1.42324264809166,-5.73303665864253));
#36105=CARTESIAN_POINT('Ctrl Pts',(96.065734054245,-1.4103449957562,-5.7360388398903));
#36106=CARTESIAN_POINT('Ctrl Pts',(96.0126358448415,-1.39439106024033,-5.73904102113806));
#36107=CARTESIAN_POINT('Ctrl Pts',(95.9606497406419,-1.37550027719898,-5.74204320238583));
#36108=CARTESIAN_POINT('Ctrl Pts',(95.9086399735217,-1.35660089549253,-5.74504675015985));
#36109=CARTESIAN_POINT('Ctrl Pts',(95.857743806863,-1.33476221007424,-5.74805029793388));
#36110=CARTESIAN_POINT('Ctrl Pts',(95.8083040086742,-1.31015170409946,-5.7510538457079));
#36111=CARTESIAN_POINT('Ctrl Pts',(95.7587709011868,-1.28549474993643,-5.75406306217287));
#36112=CARTESIAN_POINT('Ctrl Pts',(95.710700112807,-1.25805578723829,-5.75707227863784));
#36113=CARTESIAN_POINT('Ctrl Pts',(95.6644084071843,-1.2280475386761,-5.76008149510281));
#36114=CARTESIAN_POINT('Ctrl Pts',(95.6289933551998,-1.2050899986914,-5.76238366902589));
#36115=CARTESIAN_POINT('Ctrl Pts',(95.5946190515846,-1.18062963609541,-5.76468584294898));
#36116=CARTESIAN_POINT('Ctrl Pts',(95.5614139900993,-1.15477740382099,-5.76698801687206));
#36117=CARTESIAN_POINT('Ctrl Pts',(95.5179978492627,-1.12097520297683,-5.76999814553329));
#36118=CARTESIAN_POINT('Ctrl Pts',(95.4763994278315,-1.08465010225798,-5.77300827419453));
#36119=CARTESIAN_POINT('Ctrl Pts',(95.4369262799483,-1.04602489849969,-5.77601840285576));
#36120=CARTESIAN_POINT('Ctrl Pts',(95.3975232869712,-1.00746834261188,-5.7790231816702));
#36121=CARTESIAN_POINT('Ctrl Pts',(95.3602384460574,-0.966620162582308,
-5.78202796048465));
#36122=CARTESIAN_POINT('Ctrl Pts',(95.3253465106882,-0.923743501004823,
-5.78503273929909));
#36123=CARTESIAN_POINT('Ctrl Pts',(95.2904890951085,-0.880909258780438,
-5.7880345453827));
#36124=CARTESIAN_POINT('Ctrl Pts',(95.2580202271021,-0.836050918083252,
-5.79103635146632));
#36125=CARTESIAN_POINT('Ctrl Pts',(95.2281767029648,-0.789467221473735,
-5.79403815754994));
#36126=CARTESIAN_POINT('Ctrl Pts',(95.1983509165803,-0.742911212281183,
-5.79703817948454));
#36127=CARTESIAN_POINT('Ctrl Pts',(95.1711476655756,-0.694632323544357,
-5.80003820141913));
#36128=CARTESIAN_POINT('Ctrl Pts',(95.1467610553005,-0.644959137761565,
-5.80303822335373));
#36129=CARTESIAN_POINT('Ctrl Pts',(95.1223793078629,-0.59529585711228,-5.80603764706582));
#36130=CARTESIAN_POINT('Ctrl Pts',(95.1008133183402,-0.544239305376108,
-5.8090370707779));
#36131=CARTESIAN_POINT('Ctrl Pts',(95.0822106629532,-0.49214151116318,-5.81203649448999));
#36132=CARTESIAN_POINT('Ctrl Pts',(95.063590905119,-0.439995820574301,-5.81503867573775));
#36133=CARTESIAN_POINT('Ctrl Pts',(95.0479401023057,-0.386807473433288,
-5.8180408569855));
#36134=CARTESIAN_POINT('Ctrl Pts',(95.035356638252,-0.332945862371634,-5.82104303823326));
#36135=CARTESIAN_POINT('Ctrl Pts',(95.0227674464847,-0.279059734700263,
-5.82404658600728));
#36136=CARTESIAN_POINT('Ctrl Pts',(95.0132484676021,-0.224500253376058,
-5.82705013378129));
#36137=CARTESIAN_POINT('Ctrl Pts',(95.0068467170481,-0.169646007969578,
-5.83005368155531));
#36138=CARTESIAN_POINT('Ctrl Pts',(95.0004328842673,-0.114688234406487,
-5.83306289802027));
#36139=CARTESIAN_POINT('Ctrl Pts',(94.9971480639266,-0.0594351139089585,
-5.83607211448524));
#36140=CARTESIAN_POINT('Ctrl Pts',(94.9969871734786,-0.00426817539066629,
-5.8390813309502));
#36141=CARTESIAN_POINT('Ctrl Pts',(94.996864085692,0.0379367934957089,-5.84138350487334));
#36142=CARTESIAN_POINT('Ctrl Pts',(94.9985683131112,0.0800912439885254,
-5.84368567879648));
#36143=CARTESIAN_POINT('Ctrl Pts',(95.0020771381554,0.122026934858111,-5.84598785271961));
#36144=CARTESIAN_POINT('Ctrl Pts',(95.0066649821607,0.17685851111159,-5.84899798138085));
#36145=CARTESIAN_POINT('Ctrl Pts',(95.0143590174573,0.231546201030424,-5.85200811004209));
#36146=CARTESIAN_POINT('Ctrl Pts',(95.0251406920756,0.285710684426911,-5.85501823870333));
#36147=CARTESIAN_POINT('Ctrl Pts',(95.0359032046201,0.339778902274502,-5.85802301751777));
#36148=CARTESIAN_POINT('Ctrl Pts',(95.0497423640299,0.393325245198479,-5.86102779633221));
#36149=CARTESIAN_POINT('Ctrl Pts',(95.0665879055246,0.445975819683366,-5.86403257514666));
#36150=CARTESIAN_POINT('Ctrl Pts',(95.0834167811468,0.498574305147611,-5.86703438123028));
#36151=CARTESIAN_POINT('Ctrl Pts',(95.103245986732,0.55027827719602,-5.87003618731389));
#36152=CARTESIAN_POINT('Ctrl Pts',(95.1259547019121,0.600726180795795,-5.87303799339751));
#36153=CARTESIAN_POINT('Ctrl Pts',(95.1486499199739,0.651144100254258,-5.87603801533211));
#36154=CARTESIAN_POINT('Ctrl Pts',(95.1742210390583,0.700306950371653,-5.87903803726671));
#36155=CARTESIAN_POINT('Ctrl Pts',(95.2024989208809,0.747872626506352,-5.88203805920131));
#36156=CARTESIAN_POINT('Ctrl Pts',(95.2307711639229,0.795428817757702,-5.8850374829134));
#36157=CARTESIAN_POINT('Ctrl Pts',(95.2617488280683,0.841388013827451,-5.88803690662549));
#36158=CARTESIAN_POINT('Ctrl Pts',(95.2952177149497,0.885434268608315,-5.89103633033758));
#36159=CARTESIAN_POINT('Ctrl Pts',(95.328717371625,0.929521017540821,-5.89403851158534));
#36160=CARTESIAN_POINT('Ctrl Pts',(95.3647125065922,0.97169089018698,-5.8970406928331));
#36161=CARTESIAN_POINT('Ctrl Pts',(95.4029475000694,1.01165965283419,-5.90004287408086));
#36162=CARTESIAN_POINT('Ctrl Pts',(95.4411998972669,1.0516466083749,-5.90304642185487));
#36163=CARTESIAN_POINT('Ctrl Pts',(95.4816937985382,1.08943009578894,-5.90604996962889));
#36164=CARTESIAN_POINT('Ctrl Pts',(95.5241378139832,1.12476387852135,-5.90905351740291));
#36165=CARTESIAN_POINT('Ctrl Pts',(95.5666619353643,1.16016434782222,-5.91206273386788));
#36166=CARTESIAN_POINT('Ctrl Pts',(95.6111430978656,1.19310556139912,-5.91507195033284));
#36167=CARTESIAN_POINT('Ctrl Pts',(95.6572589836699,1.2233833101217,-5.91808116679781));
#36168=CARTESIAN_POINT('Ctrl Pts',(95.6925395262884,1.24654702877457,-5.92038334072093));
#36169=CARTESIAN_POINT('Ctrl Pts',(95.7287761962478,1.26815271871225,-5.92268551464406));
#36170=CARTESIAN_POINT('Ctrl Pts',(95.7658156741933,1.28812748017271,-5.92498768856718));
#36171=CARTESIAN_POINT('Ctrl Pts',(95.8142453749389,1.31424479536318,-5.92799781722842));
#36172=CARTESIAN_POINT('Ctrl Pts',(95.8642517777346,1.33768197282213,-5.93100794588966));
#36173=CARTESIAN_POINT('Ctrl Pts',(95.9155070549913,1.35824729126183,-5.9340180745509));
#36174=CARTESIAN_POINT('Ctrl Pts',(95.9666712371782,1.37877605933599,-5.93702285336535));
#36175=CARTESIAN_POINT('Ctrl Pts',(96.0190794028408,1.3964429024492,-5.94002763217979));
#36176=CARTESIAN_POINT('Ctrl Pts',(96.0723800136972,1.41110237529713,-5.94303241099424));
#36177=CARTESIAN_POINT('Ctrl Pts',(96.1256278924296,1.42574734502538,-5.94603421707786));
#36178=CARTESIAN_POINT('Ctrl Pts',(96.179765960616,1.43739069904301,-5.94903602316148));
#36179=CARTESIAN_POINT('Ctrl Pts',(96.2344253904109,1.44593607540932,-5.9520378292451));
#36180=CARTESIAN_POINT('Ctrl Pts',(96.2890523329081,1.45447637275838,-5.9550378511797));
#36181=CARTESIAN_POINT('Ctrl Pts',(96.3441995020836,1.45992226064108,-5.95803787311431));
#36182=CARTESIAN_POINT('Ctrl Pts',(96.3994879595983,1.46222847228929,-5.96103789504891));
#36183=CARTESIAN_POINT('Ctrl Pts',(96.4547653922605,1.46453422406495,-5.964037318761));
#36184=CARTESIAN_POINT('Ctrl Pts',(96.5101835299486,1.46370152095764,-5.96703674247309));
#36185=CARTESIAN_POINT('Ctrl Pts',(96.5653607221479,1.45973712815201,-5.97003616618518));
#36186=CARTESIAN_POINT('Ctrl Pts',(96.6205886417835,1.4557690906614,-5.97303834743294));
#36187=CARTESIAN_POINT('Ctrl Pts',(96.6755746454829,1.44866364926276,-5.9760405286807));
#36188=CARTESIAN_POINT('Ctrl Pts',(96.7299410102169,1.43847958821803,-5.97904270992846));
#36189=CARTESIAN_POINT('Ctrl Pts',(96.7843321213133,1.42829089161479,-5.98204625770248));
#36190=CARTESIAN_POINT('Ctrl Pts',(96.8381025175785,1.41502090868982,-5.98504980547651));
#36191=CARTESIAN_POINT('Ctrl Pts',(96.8908867549732,1.39877914363966,-5.98805335325053));
#36192=CARTESIAN_POINT('Ctrl Pts',(96.9437706137327,1.38250672499134,-5.99106256971549));
#36193=CARTESIAN_POINT('Ctrl Pts',(96.995664099223,1.36325150406159,-5.99407178618046));
#36194=CARTESIAN_POINT('Ctrl Pts',(97.0462200676117,1.34117185162974,-5.99708100264543));
#36195=CARTESIAN_POINT('Ctrl Pts',(97.0848974553757,1.32428001262397,-5.99938317656853));
#36196=CARTESIAN_POINT('Ctrl Pts',(97.1227923763854,1.30573609046428,-6.00168535049163));
#36197=CARTESIAN_POINT('Ctrl Pts',(97.1597600020344,1.28562866209272,-6.00398752441473));
#36198=CARTESIAN_POINT('Ctrl Pts',(97.2080957547711,1.25933788282639,-6.00699765307597));
#36199=CARTESIAN_POINT('Ctrl Pts',(97.255048323838,1.23026215642407,-6.0100077817372));
#36200=CARTESIAN_POINT('Ctrl Pts',(97.300278013789,1.19857129155549,-6.01301791039844));
#36201=CARTESIAN_POINT('Ctrl Pts',(97.3454273178366,1.16693675028329,-6.01602268921288));
#36202=CARTESIAN_POINT('Ctrl Pts',(97.3888593903943,1.13269659480702,-6.01902746802733));
#36203=CARTESIAN_POINT('Ctrl Pts',(97.4302603379682,1.09606577715551,-6.02203224684177));
#36204=CARTESIAN_POINT('Ctrl Pts',(97.4716203261636,1.0594711996293,-6.02503405292539));
#36205=CARTESIAN_POINT('Ctrl Pts',(97.5109527764421,1.02049099343675,-6.02803585900901));
#36206=CARTESIAN_POINT('Ctrl Pts',(97.5479754569982,0.979381410038397,-6.03103766509263));
#36207=CARTESIAN_POINT('Ctrl Pts',(97.5849761328086,0.938296260471195,-6.03403768702722));
#36208=CARTESIAN_POINT('Ctrl Pts',(97.6196694072262,0.895084633875136,-6.03703770896183));
#36209=CARTESIAN_POINT('Ctrl Pts',(97.6518103176934,0.850039167723047,-6.04003773089642));
#36210=CARTESIAN_POINT('Ctrl Pts',(97.6839448190689,0.80500268390918,-6.04303715460851));
#36211=CARTESIAN_POINT('Ctrl Pts',(97.7135276606886,0.758133516421528,-6.0460365783206));
#36212=CARTESIAN_POINT('Ctrl Pts',(97.7403559762338,0.709755004308052,-6.04903600203269));
#36213=CARTESIAN_POINT('Ctrl Pts',(97.7672089565293,0.661332015159835,-6.05203818328045));
#36214=CARTESIAN_POINT('Ctrl Pts',(97.7913020946972,0.61139737193975,-6.05504036452821));
#36215=CARTESIAN_POINT('Ctrl Pts',(97.8124782377585,0.560299547340323,-6.05804254577597));
#36216=CARTESIAN_POINT('Ctrl Pts',(97.8336640197302,0.509178464145439,-6.06104609354998));
#36217=CARTESIAN_POINT('Ctrl Pts',(97.8519299853338,0.456893643576719,-6.064049641324));
#36218=CARTESIAN_POINT('Ctrl Pts',(97.8671681700926,0.403810987515378,-6.06705318909802));
#36219=CARTESIAN_POINT('Ctrl Pts',(97.8824351143606,0.350628146874156,-6.07006240556298));
#36220=CARTESIAN_POINT('Ctrl Pts',(97.8946627453756,0.29664497904243,-6.07307162202795));
#36221=CARTESIAN_POINT('Ctrl Pts',(97.9037940249,0.242238759494788,-6.07608083849291));
#36222=CARTESIAN_POINT('Ctrl Pts',(97.9107798279656,0.200615771797842,-6.07838301241604));
#36223=CARTESIAN_POINT('Ctrl Pts',(97.9159544301644,0.158745429316313,-6.08068518633917));
#36224=CARTESIAN_POINT('Ctrl Pts',(97.9193128832873,0.116797427999095,-6.0829873602623));
#36225=CARTESIAN_POINT('Ctrl Pts',(97.9224044077598,0.0781834387904871,
-6.08510655822723));
#36226=CARTESIAN_POINT('Ctrl Pts',(97.9239630511916,0.0394451060571853,
-6.08722575619215));
#36227=CARTESIAN_POINT('Ctrl Pts',(97.9239807963238,0.000669755337866506,
-6.08934495415708));
#36228=CARTESIAN_POINT('Origin',(96.460480949577,-8.32667268468867E-16,
1.18130019239114E-14));
#36229=CARTESIAN_POINT('',(97.9239807654655,0.000734094157886227,-6.66065504581088));
#36230=CARTESIAN_POINT('',(97.9239807941682,0.000674448999180449,-6.58934495412678));
#36231=CARTESIAN_POINT('',(97.923980949577,-1.01189432752408E-15,1.19922289829666E-14));
#36232=CARTESIAN_POINT('Ctrl Pts',(97.9239807654655,0.00073409415789471,
-6.66065504581088));
#36233=CARTESIAN_POINT('Ctrl Pts',(97.9239500697605,0.0619294573548053,
-6.65734240038256));
#36234=CARTESIAN_POINT('Ctrl Pts',(97.920076940596,0.122993979023221,-6.65402975495424));
#36235=CARTESIAN_POINT('Ctrl Pts',(97.9124351738156,0.183469835983322,-6.65071710952592));
#36236=CARTESIAN_POINT('Ctrl Pts',(97.9047640051462,0.244178375316814,-6.6473917186114));
#36237=CARTESIAN_POINT('Ctrl Pts',(97.8932952909286,0.304293403245994,-6.64406632769688));
#36238=CARTESIAN_POINT('Ctrl Pts',(97.8781534976419,0.363368678428781,-6.64074093678236));
#36239=CARTESIAN_POINT('Ctrl Pts',(97.8629398160292,0.422724423867994,-6.63739975798975));
#36240=CARTESIAN_POINT('Ctrl Pts',(97.8440182538604,0.481030224079548,-6.63405857919715));
#36241=CARTESIAN_POINT('Ctrl Pts',(97.82156295279,0.537855027428008,-6.63071740040454));
#36242=CARTESIAN_POINT('Ctrl Pts',(97.8177335533478,0.547545606484042,-6.6301476147595));
#36243=CARTESIAN_POINT('Ctrl Pts',(97.8138014947121,0.557193171847244,-6.62957782911446));
#36244=CARTESIAN_POINT('Ctrl Pts',(97.8097677733136,0.566795657438289,-6.62900804346942));
#36245=CARTESIAN_POINT('Ctrl Pts',(97.788457969357,0.61752476468832,-6.62599791480819));
#36246=CARTESIAN_POINT('Ctrl Pts',(97.7642385218159,0.667157011953622,-6.62298778614695));
#36247=CARTESIAN_POINT('Ctrl Pts',(97.7372443093545,0.715337384127,-6.61997765748572));
#36248=CARTESIAN_POINT('Ctrl Pts',(97.7102980732148,0.763432126203284,-6.61697287867128));
#36249=CARTESIAN_POINT('Ctrl Pts',(97.6805871148748,0.810079656987014,-6.61396809985684));
#36250=CARTESIAN_POINT('Ctrl Pts',(97.6482938167803,0.854946105030219,-6.61096332104239));
#36251=CARTESIAN_POINT('Ctrl Pts',(97.6160324675541,0.899768165156256,-6.60796151495878));
#36252=CARTESIAN_POINT('Ctrl Pts',(97.5811941465018,0.942812206625132,-6.60495970887516));
#36253=CARTESIAN_POINT('Ctrl Pts',(97.5440055030784,0.983771717401802,-6.60195790279155));
#36254=CARTESIAN_POINT('Ctrl Pts',(97.5068389630419,1.0247068835443,-6.59895788085695));
#36255=CARTESIAN_POINT('Ctrl Pts',(97.467325223743,1.06355958447362,-6.59595785892235));
#36256=CARTESIAN_POINT('Ctrl Pts',(97.4257308754801,1.10005673969302,-6.59295783698776));
#36257=CARTESIAN_POINT('Ctrl Pts',(97.3841448213818,1.13654661715901,-6.58995841327567));
#36258=CARTESIAN_POINT('Ctrl Pts',(97.3404793790073,1.17068153361597,-6.58695898956358));
#36259=CARTESIAN_POINT('Ctrl Pts',(97.2950359079084,1.20222721293624,-6.5839595658515));
#36260=CARTESIAN_POINT('Ctrl Pts',(97.2495506581198,1.23380189393962,-6.58095738460374));
#36261=CARTESIAN_POINT('Ctrl Pts',(97.2022845485745,1.26278228021625,-6.57795520335599));
#36262=CARTESIAN_POINT('Ctrl Pts',(97.1535685310457,1.28897705736522,-6.57495302210823));
#36263=CARTESIAN_POINT('Ctrl Pts',(97.1048303390671,1.31518375779526,-6.57194947433421));
#36264=CARTESIAN_POINT('Ctrl Pts',(97.0546414029244,1.33860209783461,-6.5689459265602));
#36265=CARTESIAN_POINT('Ctrl Pts',(97.0033549495939,1.35908795525001,-6.56594237878618));
#36266=CARTESIAN_POINT('Ctrl Pts',(96.9519717017138,1.37961247627365,-6.56293316232122));
#36267=CARTESIAN_POINT('Ctrl Pts',(96.8994873007415,1.39719329036052,-6.55992394585626));
#36268=CARTESIAN_POINT('Ctrl Pts',(96.8462713981076,1.41173580383248,-6.55691472939129));
#36269=CARTESIAN_POINT('Ctrl Pts',(96.8055590516326,1.42286142263786,-6.55461255546815));
#36270=CARTESIAN_POINT('Ctrl Pts',(96.7644189230227,1.43220978642083,-6.55231038154501));
#36271=CARTESIAN_POINT('Ctrl Pts',(96.7230193560468,1.43975895035534,-6.55000820762187));
#36272=CARTESIAN_POINT('Ctrl Pts',(96.6688887702276,1.44962960109082,-6.54699807896063));
#36273=CARTESIAN_POINT('Ctrl Pts',(96.614087016333,1.45646402702743,-6.54398795029939));
#36274=CARTESIAN_POINT('Ctrl Pts',(96.5589851262422,1.46018121381543,-6.54097782163815));
#36275=CARTESIAN_POINT('Ctrl Pts',(96.5039811677362,1.46389179411512,-6.5379730428237));
#36276=CARTESIAN_POINT('Ctrl Pts',(96.4486786542793,1.46449609459621,-6.53496826400925));
#36277=CARTESIAN_POINT('Ctrl Pts',(96.3934568652473,1.46196443941696,-6.5319634851948));
#36278=CARTESIAN_POINT('Ctrl Pts',(96.3382897090267,1.45943528889109,-6.52896167911118));
#36279=CARTESIAN_POINT('Ctrl Pts',(96.2832036439936,1.45377635269247,-6.52595987302756));
#36280=CARTESIAN_POINT('Ctrl Pts',(96.2285792225989,1.44500997886678,-6.52295806694393));
#36281=CARTESIAN_POINT('Ctrl Pts',(96.1739872676945,1.43624881541007,-6.51995804500933));
#36282=CARTESIAN_POINT('Ctrl Pts',(96.1198569329886,1.42438395858338,-6.51695802307473));
#36283=CARTESIAN_POINT('Ctrl Pts',(96.0665625946391,1.40948947482519,-6.51395800114012));
#36284=CARTESIAN_POINT('Ctrl Pts',(96.0132788835028,1.39459796111709,-6.51095857742803));
#36285=CARTESIAN_POINT('Ctrl Pts',(95.9608313459994,1.37667816231465,-6.50795915371594));
#36286=CARTESIAN_POINT('Ctrl Pts',(95.9095808563667,1.35585446759632,-6.50495973000384));
#36287=CARTESIAN_POINT('Ctrl Pts',(95.8582832493319,1.33501162850679,-6.50195754875608));
#36288=CARTESIAN_POINT('Ctrl Pts',(95.8081853791708,1.31125975898834,-6.49895536750831));
#36289=CARTESIAN_POINT('Ctrl Pts',(95.7596283075926,1.28477150662033,-6.49595318626055));
#36290=CARTESIAN_POINT('Ctrl Pts',(95.7110491339133,1.25827119738783,-6.49294963848653));
#36291=CARTESIAN_POINT('Ctrl Pts',(95.664012606188,1.22903230170261,-6.4899460907125));
#36292=CARTESIAN_POINT('Ctrl Pts',(95.6188324324989,1.19727190884122,-6.48694254293848));
#36293=CARTESIAN_POINT('Ctrl Pts',(95.5735669888356,1.16545157358335,-6.48393332647351));
#36294=CARTESIAN_POINT('Ctrl Pts',(95.5301653132286,1.13110056306101,-6.48092411000854));
#36295=CARTESIAN_POINT('Ctrl Pts',(95.48890860652,1.0944767846815,-6.47791489354357));
#36296=CARTESIAN_POINT('Ctrl Pts',(95.4573455350552,1.06645809326073,-6.47561271962048));
#36297=CARTESIAN_POINT('Ctrl Pts',(95.4270372240236,1.03711003762185,-6.47331054569739));
#36298=CARTESIAN_POINT('Ctrl Pts',(95.3980940351819,1.00656161963493,-6.4710083717743));
#36299=CARTESIAN_POINT('Ctrl Pts',(95.360250359947,0.966619082011855,-6.46799824311307));
#36300=CARTESIAN_POINT('Ctrl Pts',(95.3245828810931,0.924455441751405,-6.46498811445183));
#36301=CARTESIAN_POINT('Ctrl Pts',(95.2913621806809,0.88033718211545,-6.4619779857906));
#36302=CARTESIAN_POINT('Ctrl Pts',(95.258200522814,0.836297333058049,-6.45897320697615));
#36303=CARTESIAN_POINT('Ctrl Pts',(95.2274773286411,0.790310177095552,-6.45596842816171));
#36304=CARTESIAN_POINT('Ctrl Pts',(95.1994246892403,0.742677156149086,-6.45296364934727));
#36305=CARTESIAN_POINT('Ctrl Pts',(95.1713998032787,0.695091260185318,-6.44996184326365));
#36306=CARTESIAN_POINT('Ctrl Pts',(95.1460405049562,0.645863177668212,-6.44696003718003));
#36307=CARTESIAN_POINT('Ctrl Pts',(95.1235360095484,0.595323842401656,-6.44395823109641));
#36308=CARTESIAN_POINT('Ctrl Pts',(95.1010448898792,0.544814545619602,-6.44095820916181));
#36309=CARTESIAN_POINT('Ctrl Pts',(95.0814054244011,0.49299602230385,-6.43795818722721));
#36310=CARTESIAN_POINT('Ctrl Pts',(95.0647601381418,0.440222292173557,-6.43495816529262));
#36311=CARTESIAN_POINT('Ctrl Pts',(95.0481181710531,0.38745908544404,-6.43195874158052));
#36312=CARTESIAN_POINT('Ctrl Pts',(95.0344693562214,0.333741553548245,-6.42895931786843));
#36313=CARTESIAN_POINT('Ctrl Pts',(95.0239066946291,0.2794399041314,-6.42595989415634));
#36314=CARTESIAN_POINT('Ctrl Pts',(95.0133343221994,0.225088332212951,-6.42295771290859));
#36315=CARTESIAN_POINT('Ctrl Pts',(95.0058538725625,0.170152089407996,-6.41995553166083));
#36316=CARTESIAN_POINT('Ctrl Pts',(95.0015071035033,0.115011158036669,-6.41695335041307));
#36317=CARTESIAN_POINT('Ctrl Pts',(94.9971583558914,0.0598451277374262,
-6.41394980263905));
#36318=CARTESIAN_POINT('Ctrl Pts',(94.9959461438304,0.00447475205460546,
-6.41094625486504));
#36319=CARTESIAN_POINT('Ctrl Pts',(94.9978600580734,-0.050718613321517,
-6.40794270709102));
#36320=CARTESIAN_POINT('Ctrl Pts',(94.9997775845075,-0.106016146886121,
-6.40493349062605));
#36321=CARTESIAN_POINT('Ctrl Pts',(95.0048329751331,-0.161135475574066,
-6.40192427416109));
#36322=CARTESIAN_POINT('Ctrl Pts',(95.0129638725916,-0.21570016651737,-6.39891505769612));
#36323=CARTESIAN_POINT('Ctrl Pts',(95.0191843423779,-0.257444391326635,
-6.39661288377299));
#36324=CARTESIAN_POINT('Ctrl Pts',(95.027203786649,-0.298864079893977,-6.39431070984987));
#36325=CARTESIAN_POINT('Ctrl Pts',(95.0369744640976,-0.339796315162534,
-6.39200853592674));
#36326=CARTESIAN_POINT('Ctrl Pts',(95.0497497787392,-0.393315857414546,
-6.3889984072655));
#36327=CARTESIAN_POINT('Ctrl Pts',(95.0655743917758,-0.446226378391436,
-6.38598827860426));
#36328=CARTESIAN_POINT('Ctrl Pts',(95.0843729612793,-0.498155652927122,
-6.38297814994303));
#36329=CARTESIAN_POINT('Ctrl Pts',(95.1031381204279,-0.549992634509871,
-6.37997337112859));
#36330=CARTESIAN_POINT('Ctrl Pts',(95.1248665685073,-0.600851337971165,
-6.37696859231414));
#36331=CARTESIAN_POINT('Ctrl Pts',(95.1494326534498,-0.650372674104561,
-6.3739638134997));
#36332=CARTESIAN_POINT('Ctrl Pts',(95.1739744343211,-0.699845017080219,
-6.37096200741608));
#36333=CARTESIAN_POINT('Ctrl Pts',(95.2013480572489,-0.747982142955453,
-6.36796020133246));
#36334=CARTESIAN_POINT('Ctrl Pts',(95.2313797427498,-0.794444757913278,
-6.36495839524884));
#36335=CARTESIAN_POINT('Ctrl Pts',(95.2613935786625,-0.84087975742006,-6.36195837331425));
#36336=CARTESIAN_POINT('Ctrl Pts',(95.2940620596879,-0.885641776033881,
-6.35895835137965));
#36337=CARTESIAN_POINT('Ctrl Pts',(95.329166559899,-0.928418010223583,-6.35595832944505));
#36338=CARTESIAN_POINT('Ctrl Pts',(95.3642640600605,-0.971185714573611,
-6.35295890573296));
#36339=CARTESIAN_POINT('Ctrl Pts',(95.4017962798758,-1.0119680128784,-6.34995948202087));
#36340=CARTESIAN_POINT('Ctrl Pts',(95.4415039758503,-1.05048473430826,-6.34696005830879));
#36341=CARTESIAN_POINT('Ctrl Pts',(95.4812481772999,-1.08903686628473,-6.34395787706103));
#36342=CARTESIAN_POINT('Ctrl Pts',(95.5231714708285,-1.12531889158668,-6.34095569581327));
#36343=CARTESIAN_POINT('Ctrl Pts',(95.5669784273062,-1.15908821609735,-6.33795351456551));
#36344=CARTESIAN_POINT('Ctrl Pts',(95.6108053237381,-1.19287291165491,-6.3349499667915));
#36345=CARTESIAN_POINT('Ctrl Pts',(95.6565171556405,-1.22414232779057,-6.33194641901748));
#36346=CARTESIAN_POINT('Ctrl Pts',(95.7037888397877,-1.25269681127665,-6.32894287124346));
#36347=CARTESIAN_POINT('Ctrl Pts',(95.7511497412833,-1.28130518654478,-6.3259336547785));
#36348=CARTESIAN_POINT('Ctrl Pts',(95.8000759080748,-1.30718814565836,-6.32292443831353));
#36349=CARTESIAN_POINT('Ctrl Pts',(95.8502179956886,-1.33019223314202,-6.31991522184857));
#36350=CARTESIAN_POINT('Ctrl Pts',(95.8885787476981,-1.347791302849,-6.31761304792544));
#36351=CARTESIAN_POINT('Ctrl Pts',(95.9276506444673,-1.36370635768065,-6.31531087400231));
#36352=CARTESIAN_POINT('Ctrl Pts',(95.9672711529135,-1.37788836502641,-6.31300870007918));
#36353=CARTESIAN_POINT('Ctrl Pts',(96.019075591687,-1.39643156298224,-6.30999857141794));
#36354=CARTESIAN_POINT('Ctrl Pts',(96.0720360834246,-1.41208812463281,-6.3069884427567));
#36355=CARTESIAN_POINT('Ctrl Pts',(96.1257997129984,-1.42471776850091,-6.30397831409546));
#36356=CARTESIAN_POINT('Ctrl Pts',(96.1794677894535,-1.43732496593321,-6.30097353528102));
#36357=CARTESIAN_POINT('Ctrl Pts',(96.2339356610926,-1.44691580180996,-6.29796875646657));
#36358=CARTESIAN_POINT('Ctrl Pts',(96.2888339252446,-1.45339930818679,-6.29496397765213));
#36359=CARTESIAN_POINT('Ctrl Pts',(96.3436778766594,-1.4598764002082,-6.29196217156851));
#36360=CARTESIAN_POINT('Ctrl Pts',(96.3989508552009,-1.46325219091202,-6.28896036548488));
#36361=CARTESIAN_POINT('Ctrl Pts',(96.4542737407385,-1.4634868364828,-6.28595855940126));
#36362=CARTESIAN_POINT('Ctrl Pts',(96.5095637446478,-1.46372134258999,-6.28295853746666));
#36363=CARTESIAN_POINT('Ctrl Pts',(96.5649030697027,-1.4608184017786,-6.27995851553206));
#36364=CARTESIAN_POINT('Ctrl Pts',(96.6199102781794,-1.45479020452483,-6.27695849359746));
#36365=CARTESIAN_POINT('Ctrl Pts',(96.6749065178862,-1.44876320933003,-6.27395906988537));
#36366=CARTESIAN_POINT('Ctrl Pts',(96.729570247858,-1.43961225283058,-6.27095964617328));
#36367=CARTESIAN_POINT('Ctrl Pts',(96.7835251678571,-1.42740137418871,-6.26796022246119));
#36368=CARTESIAN_POINT('Ctrl Pts',(96.8375296915902,-1.41517926941256,-6.26495804121343));
#36369=CARTESIAN_POINT('Ctrl Pts',(96.8908235872459,-1.39989173899911,-6.26195585996567));
#36370=CARTESIAN_POINT('Ctrl Pts',(96.9430422544056,-1.38165366032234,-6.2589536787179));
#36371=CARTESIAN_POINT('Ctrl Pts',(96.9952846903434,-1.36340728007702,-6.25595013094388));
#36372=CARTESIAN_POINT('Ctrl Pts',(97.0464504334134,-1.3422078768439,-6.25294658316986));
#36373=CARTESIAN_POINT('Ctrl Pts',(97.0961946444657,-1.31821862683356,-6.24994303539584));
#36374=CARTESIAN_POINT('Ctrl Pts',(97.1460327393448,-1.29418410115106,-6.24693381893088));
#36375=CARTESIAN_POINT('Ctrl Pts',(97.1944434796585,-1.26734946696937,-6.24392460246591));
#36376=CARTESIAN_POINT('Ctrl Pts',(97.2411074618674,-1.23792346221783,-6.24091538600094));
#36377=CARTESIAN_POINT('Ctrl Pts',(97.2768073206978,-1.2154113626102,-6.23861321207783));
#36378=CARTESIAN_POINT('Ctrl Pts',(97.3114853384534,-1.19138352101034,-6.23631103815472));
#36379=CARTESIAN_POINT('Ctrl Pts',(97.3450116415648,-1.16594927202327,-6.23400886423161));
#36380=CARTESIAN_POINT('Ctrl Pts',(97.3895217877492,-1.13218228803036,-6.23095245513339));
#36381=CARTESIAN_POINT('Ctrl Pts',(97.4322008967868,-1.09578275819487,-6.22789604603517));
#36382=CARTESIAN_POINT('Ctrl Pts',(97.472718199951,-1.05698060481507,-6.22483963693695));
#36383=CARTESIAN_POINT('Ctrl Pts',(97.5121538043451,-1.01921436049912,-6.22186482542061));
#36384=CARTESIAN_POINT('Ctrl Pts',(97.5495411637813,-0.979172570374641,
-6.21889001390427));
#36385=CARTESIAN_POINT('Ctrl Pts',(97.5846061097723,-0.937109851733445,
-6.21591520238793));
#36386=CARTESIAN_POINT('Ctrl Pts',(97.6196372587544,-0.895087674836593,
-6.21294325811489));
#36387=CARTESIAN_POINT('Ctrl Pts',(97.6523500816875,-0.851048838165583,
-6.20997131384185));
#36388=CARTESIAN_POINT('Ctrl Pts',(97.682507860416,-0.805284098430678,-6.20699936956881));
#36389=CARTESIAN_POINT('Ctrl Pts',(97.7126490811507,-0.759544485621851,
-6.2040290570285));
#36390=CARTESIAN_POINT('Ctrl Pts',(97.7402377405751,-0.712081297143327,
-6.2010587444882));
#36391=CARTESIAN_POINT('Ctrl Pts',(97.7650794754836,-0.663215603105351,
-6.19808843194789));
#36392=CARTESIAN_POINT('Ctrl Pts',(97.7911684880299,-0.611896413461828,
-6.19496898310842));
#36393=CARTESIAN_POINT('Ctrl Pts',(97.8142270779522,-0.559030689985845,
-6.19184953426896));
#36394=CARTESIAN_POINT('Ctrl Pts',(97.8340851191835,-0.505018648407742,
-6.18873008542949));
#36395=CARTESIAN_POINT('Ctrl Pts',(97.8530084023842,-0.453549062504344,
-6.18575747533509));
#36396=CARTESIAN_POINT('Ctrl Pts',(97.8690256010605,-0.401039230351928,
-6.18278486524069));
#36397=CARTESIAN_POINT('Ctrl Pts',(97.8820403515782,-0.347852147588492,
-6.17981225514629));
#36398=CARTESIAN_POINT('Ctrl Pts',(97.8950625388923,-0.294634673039838,
-6.17683794646414));
#36399=CARTESIAN_POINT('Ctrl Pts',(97.9050787684695,-0.240739708873497,
-6.17386363778198));
#36400=CARTESIAN_POINT('Ctrl Pts',(97.9120440368436,-0.18653914786186,-6.17088932909983));
#36401=CARTESIAN_POINT('Ctrl Pts',(97.919020403135,-0.132252227889061,-6.1679102813854));
#36402=CARTESIAN_POINT('Ctrl Pts',(97.9229360828988,-0.0776592775315085,
-6.16493123367097));
#36403=CARTESIAN_POINT('Ctrl Pts',(97.9237980922905,-0.0231341704168234,
-6.16195218595654));
#36404=CARTESIAN_POINT('Ctrl Pts',(97.9239232046351,-0.0152203772959857,
-6.16151980592912));
#36405=CARTESIAN_POINT('Ctrl Pts',(97.9239840784704,-0.00730800547042104,
-6.16108742590171));
#36406=CARTESIAN_POINT('Ctrl Pts',(97.9239808258401,0.000601812115853528,
-6.16065504587429));
#36407=CARTESIAN_POINT('Ctrl Pts',(97.923980796324,0.000669754741469797,
-6.08934495418968));
#36408=CARTESIAN_POINT('Ctrl Pts',(97.9240061409169,-0.0547114251152243,
-6.09237171426968));
#36409=CARTESIAN_POINT('Ctrl Pts',(97.9208833585887,-0.110218119586203,
-6.09539847434969));
#36410=CARTESIAN_POINT('Ctrl Pts',(97.914597801083,-0.165458249012885,-6.0984252344297));
#36411=CARTESIAN_POINT('Ctrl Pts',(97.9084269093797,-0.219690647022858,
-6.10139677810715));
#36412=CARTESIAN_POINT('Ctrl Pts',(97.8992077170686,-0.273665561285684,
-6.10436832178461));
#36413=CARTESIAN_POINT('Ctrl Pts',(97.8869787414137,-0.327011161713091,
-6.10733986546207));
#36414=CARTESIAN_POINT('Ctrl Pts',(97.8747603913136,-0.380310411030574,
-6.11030882721437));
#36415=CARTESIAN_POINT('Ctrl Pts',(97.8595375552866,-0.432980903985484,
-6.11327778896667));
#36416=CARTESIAN_POINT('Ctrl Pts',(97.8414001466125,-0.484659077351177,
-6.11624675071897));
#36417=CARTESIAN_POINT('Ctrl Pts',(97.8232709470958,-0.536313860701884,
-6.11921436869197));
#36418=CARTESIAN_POINT('Ctrl Pts',(97.8022299677344,-0.586976704809362,
-6.12218198666496));
#36419=CARTESIAN_POINT('Ctrl Pts',(97.7784167915995,-0.636299745648629,
-6.12514960463796));
#36420=CARTESIAN_POINT('Ctrl Pts',(97.7537836778224,-0.687321082321191,
-6.12821940392729));
#36421=CARTESIAN_POINT('Ctrl Pts',(97.7261841503896,-0.736908073167478,
-6.13128920321661));
#36422=CARTESIAN_POINT('Ctrl Pts',(97.6958254384189,-0.784701372426493,
-6.13435900250594));
#36423=CARTESIAN_POINT('Ctrl Pts',(97.6664480597674,-0.830949772249572,
-6.13732957175122));
#36424=CARTESIAN_POINT('Ctrl Pts',(97.6344875686607,-0.875518274432512,
-6.1403001409965));
#36425=CARTESIAN_POINT('Ctrl Pts',(97.600175234414,-0.918111750883227,-6.14327071024178));
#36426=CARTESIAN_POINT('Ctrl Pts',(97.5641436264403,-0.962839440776835,
-6.14639012455313));
#36427=CARTESIAN_POINT('Ctrl Pts',(97.5255186926607,-1.00538843252877,-6.14950953886447));
#36428=CARTESIAN_POINT('Ctrl Pts',(97.4846125658143,-1.04546003396744,-6.15262895317582));
#36429=CARTESIAN_POINT('Ctrl Pts',(97.4437064389679,-1.0855316354061,-6.15574836748717));
#36430=CARTESIAN_POINT('Ctrl Pts',(97.4005196863332,-1.12312546069117,-6.15886778179852));
#36431=CARTESIAN_POINT('Ctrl Pts',(97.3554019806568,-1.15799334977843,-6.16198719610987));
#36432=CARTESIAN_POINT('Ctrl Pts',(97.3118649299702,-1.19163967624316,-6.1649973247711));
#36433=CARTESIAN_POINT('Ctrl Pts',(97.2663362647515,-1.22289799115632,-6.16800745343234));
#36434=CARTESIAN_POINT('Ctrl Pts',(97.2191082653678,-1.25152580705956,-6.17101758209358));
#36435=CARTESIAN_POINT('Ctrl Pts',(97.1719642034464,-1.2801027432675,-6.17402236090802));
#36436=CARTESIAN_POINT('Ctrl Pts',(97.123127248929,-1.30605818676541,-6.17702713972246));
#36437=CARTESIAN_POINT('Ctrl Pts',(97.0729206036436,-1.3291914535261,-6.18003191853691));
#36438=CARTESIAN_POINT('Ctrl Pts',(97.0227636295158,-1.3523018337519,-6.18303372462052));
#36439=CARTESIAN_POINT('Ctrl Pts',(96.971240126264,-1.37259534829198,-6.18603553070414));
#36440=CARTESIAN_POINT('Ctrl Pts',(96.9186983381466,-1.3899169309036,-6.18903733678776));
#36441=CARTESIAN_POINT('Ctrl Pts',(96.8661877786886,-1.40722821828501,-6.19203735872236));
#36442=CARTESIAN_POINT('Ctrl Pts',(96.8126606345249,-1.42157090982353,-6.19503738065695));
#36443=CARTESIAN_POINT('Ctrl Pts',(96.7584834360717,-1.43283870970985,-6.19803740259155));
#36444=CARTESIAN_POINT('Ctrl Pts',(96.7043170408793,-1.44410426272875,-6.20103682630364));
#36445=CARTESIAN_POINT('Ctrl Pts',(96.6495013655885,-1.45229603431262,-6.20403625001572));
#36446=CARTESIAN_POINT('Ctrl Pts',(96.5944140793254,-1.45735862667903,-6.20703567372781));
#36447=CARTESIAN_POINT('Ctrl Pts',(96.5392761482814,-1.46242587336587,-6.21003785497557));
#36448=CARTESIAN_POINT('Ctrl Pts',(96.4838666344131,-1.46435814487389,-6.21304003622333));
#36449=CARTESIAN_POINT('Ctrl Pts',(96.4285677922088,-1.46315200863984,-6.21604221747108));
#36450=CARTESIAN_POINT('Ctrl Pts',(96.3732437791991,-1.46194532339935,-6.2190457652451));
#36451=CARTESIAN_POINT('Ctrl Pts',(96.318031065677,-1.45759742426576,-6.22204931301913));
#36452=CARTESIAN_POINT('Ctrl Pts',(96.2633080398926,-1.45015692036642,-6.22505286079315));
#36453=CARTESIAN_POINT('Ctrl Pts',(96.2084817336066,-1.44270237376816,-6.22806207725811));
#36454=CARTESIAN_POINT('Ctrl Pts',(96.1541474809876,-1.4321436635384,-6.23107129372307));
#36455=CARTESIAN_POINT('Ctrl Pts',(96.1006735615679,-1.41858059113119,-6.23408051018804));
#36456=CARTESIAN_POINT('Ctrl Pts',(96.0597638216776,-1.40820428488106,-6.23638268411117));
#36457=CARTESIAN_POINT('Ctrl Pts',(96.0193574297397,-1.39607063011449,-6.2386848580343));
#36458=CARTESIAN_POINT('Ctrl Pts',(95.9796116924021,-1.38224346896778,-6.24098703195743));
#36459=CARTESIAN_POINT('Ctrl Pts',(95.9276435148809,-1.36416423800564,-6.24399716061866));
#36460=CARTESIAN_POINT('Ctrl Pts',(95.8765871509405,-1.34311217613533,-6.2470072892799));
#36461=CARTESIAN_POINT('Ctrl Pts',(95.8268053911985,-1.319199581835,-6.25001741794114));
#36462=CARTESIAN_POINT('Ctrl Pts',(95.7771121076705,-1.29532948695258,-6.25302219675559));
#36463=CARTESIAN_POINT('Ctrl Pts',(95.7286894049705,-1.26860917563456,-6.25602697557003));
#36464=CARTESIAN_POINT('Ctrl Pts',(95.6818819575821,-1.23919968514544,-6.25903175438448));
#36465=CARTESIAN_POINT('Ctrl Pts',(95.6351208184082,-1.20981929047479,-6.2620335604681));
#36466=CARTESIAN_POINT('Ctrl Pts',(95.5899722139074,-1.17775526653278,-6.26503536655172));
#36467=CARTESIAN_POINT('Ctrl Pts',(95.5467562955269,-1.14321454967169,-6.26803717263534));
#36468=CARTESIAN_POINT('Ctrl Pts',(95.5035660628957,-1.10869436237996,-6.27103719456994));
#36469=CARTESIAN_POINT('Ctrl Pts',(95.4623066512841,-1.07170072892293,-6.27403721650454));
#36470=CARTESIAN_POINT('Ctrl Pts',(95.4232673570736,-1.03248254877558,-6.27703723843914));
#36471=CARTESIAN_POINT('Ctrl Pts',(95.3842358475343,-0.993272188970415,
-6.28003666215123));
#36472=CARTESIAN_POINT('Ctrl Pts',(95.3474239485744,-0.951838537499062,
-6.28303608586332));
#36473=CARTESIAN_POINT('Ctrl Pts',(95.3130844142555,-0.908467633288195,
-6.28603550957541));
#36474=CARTESIAN_POINT('Ctrl Pts',(95.2787133097086,-0.865056855812712,
-6.28903769082317));
#36475=CARTESIAN_POINT('Ctrl Pts',(95.2468194394562,-0.819705682281835,
-6.29203987207093));
#36476=CARTESIAN_POINT('Ctrl Pts',(95.2176145407144,-0.772732385577921,
-6.29504205331869));
#36477=CARTESIAN_POINT('Ctrl Pts',(95.188396348551,-0.725737707672089,-6.29804560109271));
#36478=CARTESIAN_POINT('Ctrl Pts',(95.1618698211654,-0.677119899142627,
-6.30104914886673));
#36479=CARTESIAN_POINT('Ctrl Pts',(95.1382009969599,-0.627222430168735,
-6.30405269664075));
#36480=CARTESIAN_POINT('Ctrl Pts',(95.1144875018319,-0.577230788119558,
-6.30706191310572));
#36481=CARTESIAN_POINT('Ctrl Pts',(95.0936426834794,-0.525955151436571,
-6.31007112957069));
#36482=CARTESIAN_POINT('Ctrl Pts',(95.0757841819897,-0.473758495262404,
-6.31308034603565));
#36483=CARTESIAN_POINT('Ctrl Pts',(95.0621216964509,-0.433825914101524,
-6.31538251995877));
#36484=CARTESIAN_POINT('Ctrl Pts',(95.0502060649354,-0.39335469206665,-6.31768469388188));
#36485=CARTESIAN_POINT('Ctrl Pts',(95.0400697696705,-0.352511460801641,
-6.319986867805));
#36486=CARTESIAN_POINT('Ctrl Pts',(95.0268164039759,-0.299108292685668,
-6.32299699646623));
#36487=CARTESIAN_POINT('Ctrl Pts',(95.0165510755356,-0.244844449845191,
-6.32600712512747));
#36488=CARTESIAN_POINT('Ctrl Pts',(95.0093779587212,-0.190085138633783,
-6.3290172537887));
#36489=CARTESIAN_POINT('Ctrl Pts',(95.0022175905566,-0.135423150147869,
-6.33202203260315));
#36490=CARTESIAN_POINT('Ctrl Pts',(94.998138595741,-0.0802679602288693,
-6.33502681141759));
#36491=CARTESIAN_POINT('Ctrl Pts',(94.9971944300164,-0.0249962331622791,
-6.33803159023204));
#36492=CARTESIAN_POINT('Ctrl Pts',(94.9962511983874,0.0302208116874317,
-6.34103339631566));
#36493=CARTESIAN_POINT('Ctrl Pts',(94.9984366611126,0.0855536398493844,
-6.34403520239928));
#36494=CARTESIAN_POINT('Ctrl Pts',(95.0037524329219,0.140621046659748,-6.3470370084829));
#36495=CARTESIAN_POINT('Ctrl Pts',(95.0090650452568,0.195655723687715,-6.35003703041749));
#36496=CARTESIAN_POINT('Ctrl Pts',(95.0175042283483,0.250424767422655,-6.35303705235209));
#36497=CARTESIAN_POINT('Ctrl Pts',(95.0290195925948,0.30454988666314,-6.35603707428669));
#36498=CARTESIAN_POINT('Ctrl Pts',(95.0405326606079,0.358664213027637,-6.35903649799878));
#36499=CARTESIAN_POINT('Ctrl Pts',(95.055120581734,0.412134353634326,-6.36203592171087));
#36500=CARTESIAN_POINT('Ctrl Pts',(95.072681894501,0.464592329607494,-6.36503534542295));
#36501=CARTESIAN_POINT('Ctrl Pts',(95.0902593523515,0.517098533091617,-6.36803752667071));
#36502=CARTESIAN_POINT('Ctrl Pts',(95.110815495214,0.568590210971758,-6.37103970791847));
#36503=CARTESIAN_POINT('Ctrl Pts',(95.1341994533675,0.618716124577668,-6.37404188916623));
#36504=CARTESIAN_POINT('Ctrl Pts',(95.1575940553797,0.668864854386714,-6.37704543694025));
#36505=CARTESIAN_POINT('Ctrl Pts',(95.1838187880407,0.717646114704595,-6.38004898471427));
#36506=CARTESIAN_POINT('Ctrl Pts',(95.2126767085625,0.764733173143499,-6.38305253248829));
#36507=CARTESIAN_POINT('Ctrl Pts',(95.2415890935527,0.8119091004808,-6.38606174895325));
#36508=CARTESIAN_POINT('Ctrl Pts',(95.2731442923336,0.857384003441493,-6.38907096541822));
#36509=CARTESIAN_POINT('Ctrl Pts',(95.3071025815364,0.900861027093556,-6.39208018188318));
#36510=CARTESIAN_POINT('Ctrl Pts',(95.3330820644971,0.934122732016443,-6.39438235580631));
#36511=CARTESIAN_POINT('Ctrl Pts',(95.3604671478669,0.966215710941009,-6.39668452972943));
#36512=CARTESIAN_POINT('Ctrl Pts',(95.3891360213213,0.997021712251413,-6.39898670365255));
#36513=CARTESIAN_POINT('Ctrl Pts',(95.4266210248666,1.03730104412603,-6.40199683231379));
#36514=CARTESIAN_POINT('Ctrl Pts',(95.466459518483,1.07554808367407,-6.40500696097503));
#36515=CARTESIAN_POINT('Ctrl Pts',(95.508402552488,1.11147603473779,-6.40801708963627));
#36516=CARTESIAN_POINT('Ctrl Pts',(95.5502710419033,1.14734013170907,-6.41102186845071));
#36517=CARTESIAN_POINT('Ctrl Pts',(95.594236251094,1.1808929788986,-6.41402664726515));
#36518=CARTESIAN_POINT('Ctrl Pts',(95.6400119215914,1.21188399779696,-6.4170314260796));
#36519=CARTESIAN_POINT('Ctrl Pts',(95.6857423046466,1.24284435621649,-6.42003323216322));
#36520=CARTESIAN_POINT('Ctrl Pts',(95.7332791656549,1.27124761245924,-6.42303503824684));
#36521=CARTESIAN_POINT('Ctrl Pts',(95.7823041177332,1.2968841254138,-6.42603684433046));
#36522=CARTESIAN_POINT('Ctrl Pts',(95.8312999314135,1.32250540108844,-6.42903686626505));
#36523=CARTESIAN_POINT('Ctrl Pts',(95.8817816160496,1.34536294862071,-6.43203688819965));
#36524=CARTESIAN_POINT('Ctrl Pts',(95.9334048098988,1.36529227383073,-6.43503691013424));
#36525=CARTESIAN_POINT('Ctrl Pts',(95.9850177097712,1.38521762501287,-6.43803633384634));
#36526=CARTESIAN_POINT('Ctrl Pts',(96.0377711744047,1.40221572339034,-6.44103575755843));
#36527=CARTESIAN_POINT('Ctrl Pts',(96.0913015734375,1.4161704834635,-6.44403518127053));
#36528=CARTESIAN_POINT('Ctrl Pts',(96.1448811859189,1.43013807291734,-6.44703736251828));
#36529=CARTESIAN_POINT('Ctrl Pts',(96.1992386477005,1.44105660070103,-6.45003954376604));
#36530=CARTESIAN_POINT('Ctrl Pts',(96.2539973523197,1.44886050883572,-6.4530417250138));
#36531=CARTESIAN_POINT('Ctrl Pts',(96.3087809818858,1.45666796913615,-6.45604527278782));
#36532=CARTESIAN_POINT('Ctrl Pts',(96.3639656912268,1.46135793888933,-6.45904882056184));
#36533=CARTESIAN_POINT('Ctrl Pts',(96.4191702244085,1.46291683768629,-6.46205236833586));
#36534=CARTESIAN_POINT('Ctrl Pts',(96.4744789468561,1.46447867864238,-6.46506158480083));
#36535=CARTESIAN_POINT('Ctrl Pts',(96.5298070386893,1.46289765888103,-6.46807080126579));
#36536=CARTESIAN_POINT('Ctrl Pts',(96.5847748920056,1.45821235280584,-6.47108001773076));
#36537=CARTESIAN_POINT('Ctrl Pts',(96.6268275525529,1.45462790163933,-6.47338219165387));
#36538=CARTESIAN_POINT('Ctrl Pts',(96.6686693881686,1.44922763500379,-6.475684365577));
#36539=CARTESIAN_POINT('Ctrl Pts',(96.7101348032585,1.44204896010572,-6.47798653950011));
#36540=CARTESIAN_POINT('Ctrl Pts',(96.7643514865242,1.43266272962009,-6.48099666816135));
#36541=CARTESIAN_POINT('Ctrl Pts',(96.8181520080073,1.42019495131144,-6.48400679682259));
#36542=CARTESIAN_POINT('Ctrl Pts',(96.8711601430782,1.4046974229439,-6.48701692548383));
#36543=CARTESIAN_POINT('Ctrl Pts',(96.9240740677568,1.38922743805102,-6.49002170429828));
#36544=CARTESIAN_POINT('Ctrl Pts',(96.9761978979951,1.3707385361097,-6.49302648311272));
#36545=CARTESIAN_POINT('Ctrl Pts',(97.027165357044,1.3493335511777,-6.49603126192716));
#36546=CARTESIAN_POINT('Ctrl Pts',(97.0780823922361,1.32794974293203,-6.49903306801079));
#36547=CARTESIAN_POINT('Ctrl Pts',(97.1278448379982,1.30365577019171,-6.50203487409441));
#36548=CARTESIAN_POINT('Ctrl Pts',(97.1761031489141,1.27660374345996,-6.50503668017803));
#36549=CARTESIAN_POINT('Ctrl Pts',(97.2243327770917,1.2495677953308,-6.50803670211263));
#36550=CARTESIAN_POINT('Ctrl Pts',(97.2710595826273,1.21977730007934,-6.51103672404723));
#36551=CARTESIAN_POINT('Ctrl Pts',(97.3159576393139,1.1874307909587,-6.51403674598183));
#36552=CARTESIAN_POINT('Ctrl Pts',(97.3608467430567,1.15509073192744,-6.51703616969392));
#36553=CARTESIAN_POINT('Ctrl Pts',(97.4039073939027,1.12019597977156,-6.52003559340602));
#36554=CARTESIAN_POINT('Ctrl Pts',(97.4448436809194,1.08298765604419,-6.52303501711812));
#36555=CARTESIAN_POINT('Ctrl Pts',(97.4858176029228,1.04574512465248,-6.52603719836588));
#36556=CARTESIAN_POINT('Ctrl Pts',(97.5246628675223,1.00618512821049,-6.52903937961364));
#36557=CARTESIAN_POINT('Ctrl Pts',(97.5611187918536,0.964587264143905,-6.5320415608614));
#36558=CARTESIAN_POINT('Ctrl Pts',(97.5975913101124,0.922970465653054,-6.53504510863541));
#36559=CARTESIAN_POINT('Ctrl Pts',(97.6316719945516,0.879314367459454,-6.53804865640943));
#36560=CARTESIAN_POINT('Ctrl Pts',(97.6631411544674,0.833930861386641,-6.54105220418344));
#36561=CARTESIAN_POINT('Ctrl Pts',(97.6946697071265,0.788461701583791,-6.54406142064841));
#36562=CARTESIAN_POINT('Ctrl Pts',(97.7235766127074,0.741259072640851,-6.54707063711337));
#36563=CARTESIAN_POINT('Ctrl Pts',(97.7496867620436,0.692661983295228,-6.55007985357834));
#36564=CARTESIAN_POINT('Ctrl Pts',(97.769662096364,0.655483218280092,-6.55238202750145));
#36565=CARTESIAN_POINT('Ctrl Pts',(97.7880014424451,0.61748887037511,-6.55468420142456));
#36566=CARTESIAN_POINT('Ctrl Pts',(97.8046456490466,0.578838069497681,-6.55698637534768));
#36567=CARTESIAN_POINT('Ctrl Pts',(97.8286351980216,0.523130080359468,-6.56030453375556));
#36568=CARTESIAN_POINT('Ctrl Pts',(97.8491882128639,0.465858031256992,-6.56362269216345));
#36569=CARTESIAN_POINT('Ctrl Pts',(97.8661211561645,0.40744062098,-6.56694085057134));
#36570=CARTESIAN_POINT('Ctrl Pts',(97.8829986720517,0.349214431207237,-6.57024814749254));
#36571=CARTESIAN_POINT('Ctrl Pts',(97.8962796017182,0.289850665694475,-6.57355544441374));
#36572=CARTESIAN_POINT('Ctrl Pts',(97.9058288493017,0.229786202286622,-6.57686274133495));
#36573=CARTESIAN_POINT('Ctrl Pts',(97.9153293820534,0.170028153621295,-6.58015316630763));
#36574=CARTESIAN_POINT('Ctrl Pts',(97.9211360715741,0.109576858096741,-6.58344359128031));
#36575=CARTESIAN_POINT('Ctrl Pts',(97.9231644409405,0.0488799968574776,
-6.58673401625299));
#36576=CARTESIAN_POINT('Ctrl Pts',(97.9237009416909,0.0328257652465272,
-6.58760432887759));
#36577=CARTESIAN_POINT('Ctrl Pts',(97.9239733837609,0.0167544342987488,
-6.58847464150218));
#36578=CARTESIAN_POINT('Ctrl Pts',(97.9239807941682,0.000674448999165355,
-6.58934495412678));
#36579=CARTESIAN_POINT('Origin',(96.460480949577,-8.32667268468867E-16,
1.18130019239114E-14));
#36580=CARTESIAN_POINT('',(97.9239803863197,-0.00128399919636206,-7.16065504587409));
#36581=CARTESIAN_POINT('',(97.9239803766892,-0.00129492944526685,-7.08934495420499));
#36582=CARTESIAN_POINT('',(97.923980949577,-1.01189432752408E-15,1.19922289829666E-14));
#36583=CARTESIAN_POINT('Ctrl Pts',(97.9239803863202,-0.00128399862218805,
-7.1606550458429));
#36584=CARTESIAN_POINT('Ctrl Pts',(97.9240284084967,0.0534515961901013,
-7.15768174384173));
#36585=CARTESIAN_POINT('Ctrl Pts',(97.9210014401702,0.108255387245641,-7.15470844184055));
#36586=CARTESIAN_POINT('Ctrl Pts',(97.9149031712147,0.162752115827591,-7.15173513983938));
#36587=CARTESIAN_POINT('Ctrl Pts',(97.9088083138335,0.217218357129264,-7.14876350120212));
#36588=CARTESIAN_POINT('Ctrl Pts',(97.8996456193441,0.271377341401932,-7.14579186256485));
#36589=CARTESIAN_POINT('Ctrl Pts',(97.8874707313403,0.324857526837941,-7.14282022392758));
#36590=CARTESIAN_POINT('Ctrl Pts',(97.8752976171332,0.378329920581715,-7.13984901823746));
#36591=CARTESIAN_POINT('Ctrl Pts',(97.8601133014658,0.431123186603639,-7.13687781254734));
#36592=CARTESIAN_POINT('Ctrl Pts',(97.8420242977194,0.482877031140819,-7.13390660685723));
#36593=CARTESIAN_POINT('Ctrl Pts',(97.8239180353275,0.53468025381267,-7.13093256635172));
#36594=CARTESIAN_POINT('Ctrl Pts',(97.8029017321617,0.585441565881671,-7.12795852584622));
#36595=CARTESIAN_POINT('Ctrl Pts',(97.7791309073797,0.6348185085415,-7.12498448534072));
#36596=CARTESIAN_POINT('Ctrl Pts',(97.7553473168163,0.684221968382254,-7.12200884766929));
#36597=CARTESIAN_POINT('Ctrl Pts',(97.7288065230378,0.732239107887783,-7.11903320999787));
#36598=CARTESIAN_POINT('Ctrl Pts',(97.6997094827783,0.778553076225247,-7.11605757232644));
#36599=CARTESIAN_POINT('Ctrl Pts',(97.6705602221932,0.824950164030577,-7.11307659429165));
#36600=CARTESIAN_POINT('Ctrl Pts',(97.6388458752375,0.869637543718845,-7.11009561625686));
#36601=CARTESIAN_POINT('Ctrl Pts',(97.6048091565678,0.912329548291191,-7.10711463822207));
#36602=CARTESIAN_POINT('Ctrl Pts',(97.5891757490176,0.931938415793702,-7.10574544499965));
#36603=CARTESIAN_POINT('Ctrl Pts',(97.5730529323351,0.951126822072045,-7.10437625177722));
#36604=CARTESIAN_POINT('Ctrl Pts',(97.5564667651661,0.969869755187462,-7.1030070585548));
#36605=CARTESIAN_POINT('Ctrl Pts',(97.5200025931577,1.01107550996509,-7.09999692989356));
#36606=CARTESIAN_POINT('Ctrl Pts',(97.4811347572606,1.05030856924528,-7.09698680123233));
#36607=CARTESIAN_POINT('Ctrl Pts',(97.440104944285,1.08727599025841,-7.09397667257109));
#36608=CARTESIAN_POINT('Ctrl Pts',(97.3991480528479,1.12417770974811,-7.09097189375665));
#36609=CARTESIAN_POINT('Ctrl Pts',(97.3560371988642,1.15882143129324,-7.08796711494221));
#36610=CARTESIAN_POINT('Ctrl Pts',(97.311052273536,1.190949483756,-7.08496233612777));
#36611=CARTESIAN_POINT('Ctrl Pts',(97.2661118533386,1.22304575083361,-7.08196053004415));
#36612=CARTESIAN_POINT('Ctrl Pts',(97.2193014622973,1.25263097367006,-7.07895872396053));
#36613=CARTESIAN_POINT('Ctrl Pts',(97.1709341354984,1.27948760080513,-7.07595691787692));
#36614=CARTESIAN_POINT('Ctrl Pts',(97.1225955562323,1.30632826547508,-7.07295689594232));
#36615=CARTESIAN_POINT('Ctrl Pts',(97.0727023361604,1.33044329302545,-7.06995687400772));
#36616=CARTESIAN_POINT('Ctrl Pts',(97.0215946080853,1.3516596140432,-7.06695685207312));
#36617=CARTESIAN_POINT('Ctrl Pts',(96.9704970712002,1.37287170439828,-7.06395742836103));
#36618=CARTESIAN_POINT('Ctrl Pts',(96.9181859947554,1.39118603377388,-7.06095800464894));
#36619=CARTESIAN_POINT('Ctrl Pts',(96.8650219868468,1.40647744353213,-7.05795858093685));
#36620=CARTESIAN_POINT('Ctrl Pts',(96.8118091023332,1.42178291152684,-7.05495639968909));
#36621=CARTESIAN_POINT('Ctrl Pts',(96.7577422283616,1.43405976125443,-7.05195421844133));
#36622=CARTESIAN_POINT('Ctrl Pts',(96.7031962108579,1.44323302066623,-7.04895203719357));
#36623=CARTESIAN_POINT('Ctrl Pts',(96.6486253652178,1.45241045554207,-7.04594848941955));
#36624=CARTESIAN_POINT('Ctrl Pts',(96.5935754671363,1.45848142601986,-7.04294494164554));
#36625=CARTESIAN_POINT('Ctrl Pts',(96.5384273126797,1.46142280483064,-7.03994139387152));
#36626=CARTESIAN_POINT('Ctrl Pts',(96.4831750753627,1.46436973499891,-7.03693217740656));
#36627=CARTESIAN_POINT('Ctrl Pts',(96.4278247406292,1.46417527605419,-7.03392296094159));
#36628=CARTESIAN_POINT('Ctrl Pts',(96.3727567635999,1.46086848045765,-7.03091374447663));
#36629=CARTESIAN_POINT('Ctrl Pts',(96.3306275043085,1.45833864630311,-7.0286115705535));
#36630=CARTESIAN_POINT('Ctrl Pts',(96.2886635144571,1.45398828503214,-7.02630939663037));
#36631=CARTESIAN_POINT('Ctrl Pts',(96.2470312747839,1.44785064365449,-7.02400722270724));
#36632=CARTESIAN_POINT('Ctrl Pts',(96.1925964657486,1.43982558089201,-7.020997094046));
#36633=CARTESIAN_POINT('Ctrl Pts',(96.1385004897705,1.42870951185745,-7.01798696538476));
#36634=CARTESIAN_POINT('Ctrl Pts',(96.0851207510273,1.41454479297927,-7.01497683672353));
#36635=CARTESIAN_POINT('Ctrl Pts',(96.0318358831207,1.4004052487977,-7.01197205790908));
#36636=CARTESIAN_POINT('Ctrl Pts',(95.9792652325821,1.38322794180095,-7.00896727909463));
#36637=CARTESIAN_POINT('Ctrl Pts',(95.9277775373783,1.36310649790536,-7.00596250028019));
#36638=CARTESIAN_POINT('Ctrl Pts',(95.8763407807187,1.34300496084492,-7.00296069419656));
#36639=CARTESIAN_POINT('Ctrl Pts',(95.8259853464624,1.31996524816035,-6.99995888811294));
#36640=CARTESIAN_POINT('Ctrl Pts',(95.7770644809546,1.29413066589723,-6.99695708202932));
#36641=CARTESIAN_POINT('Ctrl Pts',(95.7281726919799,1.26831143863818,-6.99395706009472));
#36642=CARTESIAN_POINT('Ctrl Pts',(95.6807142478144,1.23970088044208,-6.99095703816012));
#36643=CARTESIAN_POINT('Ctrl Pts',(95.6350199459775,1.20848929723705,-6.98795701622552));
#36644=CARTESIAN_POINT('Ctrl Pts',(95.5893347558606,1.1772839378104,-6.98495759251343));
#36645=CARTESIAN_POINT('Ctrl Pts',(95.5454134452998,1.143478881119,-6.98195816880133));
#36646=CARTESIAN_POINT('Ctrl Pts',(95.5035578728706,1.10730775995957,-6.97895874508924));
#36647=CARTESIAN_POINT('Ctrl Pts',(95.4616638203048,1.07110338469324,-6.97595656384148));
#36648=CARTESIAN_POINT('Ctrl Pts',(95.4218397005595,1.03252894514053,-6.97295438259372));
#36649=CARTESIAN_POINT('Ctrl Pts',(95.3843531190853,0.991857420419462,-6.96995220134596));
#36650=CARTESIAN_POINT('Ctrl Pts',(95.3468494745513,0.951167382923188,-6.96694865357194));
#36651=CARTESIAN_POINT('Ctrl Pts',(95.3116858251814,0.908378766162068,-6.96394510579792));
#36652=CARTESIAN_POINT('Ctrl Pts',(95.2790896061615,0.863797860441274,-6.9609415580239));
#36653=CARTESIAN_POINT('Ctrl Pts',(95.246431867264,0.819132815763593,-6.95793234155893));
#36654=CARTESIAN_POINT('Ctrl Pts',(95.2163515262493,0.772669169180109,-6.95492312509396));
#36655=CARTESIAN_POINT('Ctrl Pts',(95.1890321300838,0.724741436244182,-6.951913908629));
#36656=CARTESIAN_POINT('Ctrl Pts',(95.1681316723801,0.688074756314977,-6.94961173470589));
#36657=CARTESIAN_POINT('Ctrl Pts',(95.1488462577054,0.650551765119949,-6.94730956078278));
#36658=CARTESIAN_POINT('Ctrl Pts',(95.131239005216,0.612330060793418,-6.94500738685968));
#36659=CARTESIAN_POINT('Ctrl Pts',(95.1082172452907,0.562354580435533,-6.94199725819844));
#36660=CARTESIAN_POINT('Ctrl Pts',(95.0879694233587,0.510973968189141,-6.93898712953721));
#36661=CARTESIAN_POINT('Ctrl Pts',(95.0706662769323,0.458527453596354,-6.93597700087597));
#36662=CARTESIAN_POINT('Ctrl Pts',(95.0533938830727,0.406174151237822,-6.93297222206153));
#36663=CARTESIAN_POINT('Ctrl Pts',(95.039055942892,0.352759203469606,-6.92996744324708));
#36664=CARTESIAN_POINT('Ctrl Pts',(95.0277755191432,0.298642595095792,-6.92696266443264));
#36665=CARTESIAN_POINT('Ctrl Pts',(95.0165062555048,0.244579526140235,-6.92396085834902));
#36666=CARTESIAN_POINT('Ctrl Pts',(95.0082886233428,0.189816686172077,-6.9209590522654));
#36667=CARTESIAN_POINT('Ctrl Pts',(95.0031956124036,0.134728230373038,-6.91795724618177));
#36668=CARTESIAN_POINT('Ctrl Pts',(94.9981056285388,0.0796725168670466,
-6.91495722424717));
#36669=CARTESIAN_POINT('Ctrl Pts',(94.9961366334338,0.0242920959479925,
-6.91195720231257));
#36670=CARTESIAN_POINT('Ctrl Pts',(94.9973099872178,-0.0310319981469414,
-6.90895718037797));
#36671=CARTESIAN_POINT('Ctrl Pts',(94.9984831070281,-0.0863450602830034,
-6.90595775666589));
#36672=CARTESIAN_POINT('Ctrl Pts',(95.0027973201282,-0.141601290199693,
-6.9029583329538));
#36673=CARTESIAN_POINT('Ctrl Pts',(95.0102218871038,-0.196420217173161,
-6.89995890924171));
#36674=CARTESIAN_POINT('Ctrl Pts',(95.0176532798934,-0.251289542210087,
-6.89695672799395));
#36675=CARTESIAN_POINT('Ctrl Pts',(95.0282006684755,-0.305720236624135,
-6.89395454674619));
#36676=CARTESIAN_POINT('Ctrl Pts',(95.0417816440599,-0.359339018929665,
-6.89095236549844));
#36677=CARTESIAN_POINT('Ctrl Pts',(95.0553688014029,-0.412982207314665,
-6.88794881772442));
#36678=CARTESIAN_POINT('Ctrl Pts',(95.0719921395309,-0.465812242245802,
-6.88494526995039));
#36679=CARTESIAN_POINT('Ctrl Pts',(95.0915194017629,-0.517471284813382,
-6.88194172217638));
#36680=CARTESIAN_POINT('Ctrl Pts',(95.111083518416,-0.569227825129932,-6.87893250571141));
#36681=CARTESIAN_POINT('Ctrl Pts',(95.1335622926563,-0.619808474374922,
-6.87592328924644));
#36682=CARTESIAN_POINT('Ctrl Pts',(95.1587758480468,-0.668876729039158,
-6.87291407278148));
#36683=CARTESIAN_POINT('Ctrl Pts',(95.1780652512535,-0.706415954833038,
-6.87061189885836));
#36684=CARTESIAN_POINT('Ctrl Pts',(95.1989542913622,-0.743070423738718,
-6.86830972493524));
#36685=CARTESIAN_POINT('Ctrl Pts',(95.2213454637532,-0.778701160762088,
-6.86600755101212));
#36686=CARTESIAN_POINT('Ctrl Pts',(95.2506222742913,-0.825288910565812,
-6.86299742235088));
#36687=CARTESIAN_POINT('Ctrl Pts',(95.2825915894323,-0.870321171193206,
-6.85998729368965));
#36688=CARTESIAN_POINT('Ctrl Pts',(95.3170625856117,-0.913469591692483,
-6.85697716502841));
#36689=CARTESIAN_POINT('Ctrl Pts',(95.3514723171179,-0.956541325290622,
-6.85397238621397));
#36690=CARTESIAN_POINT('Ctrl Pts',(95.3883745791975,-0.997735453842079,
-6.85096760739953));
#36691=CARTESIAN_POINT('Ctrl Pts',(95.4275351158937,-1.0367522146956,-6.84796282858509));
#36692=CARTESIAN_POINT('Ctrl Pts',(95.4666569097267,-1.07573037492832,-6.84496102250147));
#36693=CARTESIAN_POINT('Ctrl Pts',(95.5080321800748,-1.11253506380543,-6.84195921641785));
#36694=CARTESIAN_POINT('Ctrl Pts',(95.5513874432147,-1.14690071352749,-6.83895741033423));
#36695=CARTESIAN_POINT('Ctrl Pts',(95.5947169377845,-1.18124593773287,-6.83595738839963));
#36696=CARTESIAN_POINT('Ctrl Pts',(95.6400236795582,-1.21315466871284,-6.83295736646503));
#36697=CARTESIAN_POINT('Ctrl Pts',(95.687000213198,-1.24240082117273,-6.82995734453043));
#36698=CARTESIAN_POINT('Ctrl Pts',(95.7339673794331,-1.27164114177298,-6.82695792081835));
#36699=CARTESIAN_POINT('Ctrl Pts',(95.7826032281977,-1.29821965930536,-6.82395849710626));
#36700=CARTESIAN_POINT('Ctrl Pts',(95.8325723091258,-1.32195423114674,-6.82095907339417));
#36701=CARTESIAN_POINT('Ctrl Pts',(95.8825873293864,-1.34571062348925,-6.81795689214642));
#36702=CARTESIAN_POINT('Ctrl Pts',(95.9339375525643,-1.36661761944449,-6.81495471089866));
#36703=CARTESIAN_POINT('Ctrl Pts',(95.9862653175298,-1.38454027905369,-6.8119525296509));
#36704=CARTESIAN_POINT('Ctrl Pts',(96.0386169009323,-1.40247109665969,-6.80894898187689));
#36705=CARTESIAN_POINT('Ctrl Pts',(96.0919464036947,-1.41741472729072,-6.80594543410287));
#36706=CARTESIAN_POINT('Ctrl Pts',(96.1458818615687,-1.42928641770092,-6.80294188632886));
#36707=CARTESIAN_POINT('Ctrl Pts',(96.1999191135424,-1.44118051392886,-6.7999326698639));
#36708=CARTESIAN_POINT('Ctrl Pts',(96.2545640825608,-1.44999100372019,-6.79692345339893));
#36709=CARTESIAN_POINT('Ctrl Pts',(96.3094366540997,-1.45568467423538,-6.79391423693396));
#36710=CARTESIAN_POINT('Ctrl Pts',(96.3514164201826,-1.46004056552456,-6.79161206301083));
#36711=CARTESIAN_POINT('Ctrl Pts',(96.393529213884,-1.46257329016689,-6.78930988908769));
#36712=CARTESIAN_POINT('Ctrl Pts',(96.4356053637645,-1.46328857551424,-6.78700771516456));
#36713=CARTESIAN_POINT('Ctrl Pts',(96.490620592387,-1.46422382237087,-6.78399758650331));
#36714=CARTESIAN_POINT('Ctrl Pts',(96.5458042309069,-1.46205411097958,-6.78098745784207));
#36715=CARTESIAN_POINT('Ctrl Pts',(96.6007770113185,-1.45675985154034,-6.77797732918083));
#36716=CARTESIAN_POINT('Ctrl Pts',(96.6556520896096,-1.45147500149188,-6.77497255036638));
#36717=CARTESIAN_POINT('Ctrl Pts',(96.7103165320628,-1.44307667398022,-6.77196777155193));
#36718=CARTESIAN_POINT('Ctrl Pts',(96.7643912828551,-1.43159727553765,-6.76896299273748));
#36719=CARTESIAN_POINT('Ctrl Pts',(96.8184125356401,-1.420129234058,-6.76596118665386));
#36720=CARTESIAN_POINT('Ctrl Pts',(96.871844738392,-1.40558626913275,-6.76295938057023));
#36721=CARTESIAN_POINT('Ctrl Pts',(96.9243160404985,-1.38805232553742,-6.75995757448661));
#36722=CARTESIAN_POINT('Ctrl Pts',(96.9767561558396,-1.37052880339086,-6.75695755255201));
#36723=CARTESIAN_POINT('Ctrl Pts',(97.0282360026413,-1.35001799316396,-6.7539575306174));
#36724=CARTESIAN_POINT('Ctrl Pts',(97.0783982359955,-1.32665386485894,-6.7509575086828));
#36725=CARTESIAN_POINT('Ctrl Pts',(97.1285504666972,-1.30329439550231,-6.7479580849707));
#36726=CARTESIAN_POINT('Ctrl Pts',(97.1773851272762,-1.27708296087088,-6.7449586612586));
#36727=CARTESIAN_POINT('Ctrl Pts',(97.2245663796204,-1.24820098765999,-6.7419592375465));
#36728=CARTESIAN_POINT('Ctrl Pts',(97.2717910082924,-1.21929246165803,-6.73895705629874));
#36729=CARTESIAN_POINT('Ctrl Pts',(97.3173587404368,-1.1877087682782,-6.73595487505097));
#36730=CARTESIAN_POINT('Ctrl Pts',(97.3609611355696,-1.15367572767863,-6.73295269380321));
#36731=CARTESIAN_POINT('Ctrl Pts',(97.4045833775446,-1.11962719599447,-6.72994914602919));
#36732=CARTESIAN_POINT('Ctrl Pts',(97.4462381013335,-1.08312744329101,-6.72694559825516));
#36733=CARTESIAN_POINT('Ctrl Pts',(97.4856510840067,-1.04444169079626,-6.72394205048114));
#36734=CARTESIAN_POINT('Ctrl Pts',(97.5251384520517,-1.00568292545424,-6.72093283401617));
#36735=CARTESIAN_POINT('Ctrl Pts',(97.5623752709247,-0.964730310279934,
-6.7179236175512));
#36736=CARTESIAN_POINT('Ctrl Pts',(97.5971260308949,-0.921884054052279,
-6.71491440108623));
#36737=CARTESIAN_POINT('Ctrl Pts',(97.6237117864701,-0.889104912060561,
-6.71261222716315));
#36738=CARTESIAN_POINT('Ctrl Pts',(97.6488432766803,-0.855218184759521,
-6.71031005324007));
#36739=CARTESIAN_POINT('Ctrl Pts',(97.6724325905286,-0.820369105948431,
-6.70800787931698));
#36740=CARTESIAN_POINT('Ctrl Pts',(97.7037292966424,-0.774133705253864,
-6.70495351066697));
#36741=CARTESIAN_POINT('Ctrl Pts',(97.732438933426,-0.726012933133433,-6.70189914201697));
#36742=CARTESIAN_POINT('Ctrl Pts',(97.758333054594,-0.676322529199528,-6.69884477336696));
#36743=CARTESIAN_POINT('Ctrl Pts',(97.7853132466074,-0.624547972702387,
-6.69566229607329));
#36744=CARTESIAN_POINT('Ctrl Pts',(97.8092360930233,-0.571069584415693,
-6.69247981877961));
#36745=CARTESIAN_POINT('Ctrl Pts',(97.8298924651478,-0.516279334297092,
-6.68929734148594));
#36746=CARTESIAN_POINT('Ctrl Pts',(97.8496510794807,-0.463870352953487,
-6.68625317956389));
#36747=CARTESIAN_POINT('Ctrl Pts',(97.8664210779866,-0.41026171723104,-6.68320901764185));
#36748=CARTESIAN_POINT('Ctrl Pts',(97.8800668537132,-0.3558203349695,-6.6801648557198));
#36749=CARTESIAN_POINT('Ctrl Pts',(97.8937003451011,-0.30142796248155,-6.67712343424409));
#36750=CARTESIAN_POINT('Ctrl Pts',(97.9042150716696,-0.246204821887107,
-6.67408201276838));
#36751=CARTESIAN_POINT('Ctrl Pts',(97.9115251914004,-0.190533089701565,
-6.67104059129267));
#36752=CARTESIAN_POINT('Ctrl Pts',(97.9188312553177,-0.134892245404056,
-6.66800085726376));
#36753=CARTESIAN_POINT('Ctrl Pts',(97.9229361774325,-0.0788038064188046,
-6.66496112323484));
#36754=CARTESIAN_POINT('Ctrl Pts',(97.9238055394607,-0.0226582135575034,
-6.66192138920592));
#36755=CARTESIAN_POINT('Ctrl Pts',(97.9239262639303,-0.0148615227717745,
-6.66149927475158));
#36756=CARTESIAN_POINT('Ctrl Pts',(97.9239846768685,-0.00706373686963602,
-6.66107716029724));
#36757=CARTESIAN_POINT('Ctrl Pts',(97.9239807654658,0.000734093566312587,
-6.6606550458429));
#36758=CARTESIAN_POINT('Ctrl Pts',(97.9239807941685,0.000674448439337589,
-6.58934495415708));
#36759=CARTESIAN_POINT('Ctrl Pts',(97.9240067388656,-0.0556234952178808,
-6.59239202230983));
#36760=CARTESIAN_POINT('Ctrl Pts',(97.9207798368809,-0.111913354676098,
-6.59543909046258));
#36761=CARTESIAN_POINT('Ctrl Pts',(97.9143291626584,-0.167802334071808,
-6.59848615861533));
#36762=CARTESIAN_POINT('Ctrl Pts',(97.9077134966479,-0.22512081096258,-6.60161116299699));
#36763=CARTESIAN_POINT('Ctrl Pts',(97.8977069013895,-0.28201705927344,-6.60473616737865));
#36764=CARTESIAN_POINT('Ctrl Pts',(97.8843968830571,-0.338076417961225,
-6.60786117176031));
#36765=CARTESIAN_POINT('Ctrl Pts',(97.8713913919585,-0.392853163732691,
-6.61091467744706));
#36766=CARTESIAN_POINT('Ctrl Pts',(97.8552322800615,-0.446830443496005,
-6.61396818313381));
#36767=CARTESIAN_POINT('Ctrl Pts',(97.8360516456787,-0.499637378531921,
-6.61702168882056));
#36768=CARTESIAN_POINT('Ctrl Pts',(97.8161973313687,-0.554299047433307,
-6.62018244254967));
#36769=CARTESIAN_POINT('Ctrl Pts',(97.7931054900853,-0.607706069216668,
-6.62334319627879));
#36770=CARTESIAN_POINT('Ctrl Pts',(97.7669754134871,-0.659472869625587,
-6.6265039500079));
#36771=CARTESIAN_POINT('Ctrl Pts',(97.740845336889,-0.7112396700345,-6.62966470373701));
#36772=CARTESIAN_POINT('Ctrl Pts',(97.7116773880182,-0.761365777376917,
-6.63282545746612));
#36773=CARTESIAN_POINT('Ctrl Pts',(97.6797197261331,-0.809499262348027,
-6.63598621119524));
#36774=CARTESIAN_POINT('Ctrl Pts',(97.6492850000422,-0.855338956007879,
-6.63899633985647));
#36775=CARTESIAN_POINT('Ctrl Pts',(97.6161975820751,-0.899556196763912,
-6.64200646851771));
#36776=CARTESIAN_POINT('Ctrl Pts',(97.5806564616684,-0.941827517176423,
-6.64501659717895));
#36777=CARTESIAN_POINT('Ctrl Pts',(97.5451785078471,-0.984023709541822,
-6.64802137599339));
#36778=CARTESIAN_POINT('Ctrl Pts',(97.5072558429796,-1.0242804439233,-6.65102615480783));
#36779=CARTESIAN_POINT('Ctrl Pts',(97.4671301590771,-1.06230392026613,-6.65403093362228));
#36780=CARTESIAN_POINT('Ctrl Pts',(97.427044172891,-1.10028977867862,-6.6570327397059));
#36781=CARTESIAN_POINT('Ctrl Pts',(97.3847598666553,-1.13604639437271,-6.66003454578952));
#36782=CARTESIAN_POINT('Ctrl Pts',(97.3405572911961,-1.16931513413723,-6.66303635187314));
#36783=CARTESIAN_POINT('Ctrl Pts',(97.2963809879142,-1.20256410034279,-6.66603637380774));
#36784=CARTESIAN_POINT('Ctrl Pts',(97.250289096355,-1.23332780453114,-6.66903639574234));
#36785=CARTESIAN_POINT('Ctrl Pts',(97.2025946391917,-1.26138793465233,-6.67203641767694));
#36786=CARTESIAN_POINT('Ctrl Pts',(97.1549096925914,-1.289442469414,-6.67503584138903));
#36787=CARTESIAN_POINT('Ctrl Pts',(97.1056232699489,-1.31479423310814,-6.67803526510112));
#36788=CARTESIAN_POINT('Ctrl Pts',(97.05507527934,-1.33726954388924,-6.68103468881322));
#36789=CARTESIAN_POINT('Ctrl Pts',(97.004480817175,-1.35976551746326,-6.68403687006098));
#36790=CARTESIAN_POINT('Ctrl Pts',(96.9526229534576,-1.37937953976783,-6.68703905130873));
#36791=CARTESIAN_POINT('Ctrl Pts',(96.8998626175477,-1.39598567322567,-6.69004123255649));
#36792=CARTESIAN_POINT('Ctrl Pts',(96.847078266304,-1.41259936542684,-6.69304478033051));
#36793=CARTESIAN_POINT('Ctrl Pts',(96.7933911368269,-1.42620230958813,-6.69604832810453));
#36794=CARTESIAN_POINT('Ctrl Pts',(96.7391751998421,-1.43671909741228,-6.69905187587855));
#36795=CARTESIAN_POINT('Ctrl Pts',(96.6848569394005,-1.44725573390355,-6.70206109234352));
#36796=CARTESIAN_POINT('Ctrl Pts',(96.6300084023298,-1.45469450736379,-6.70507030880848));
#36797=CARTESIAN_POINT('Ctrl Pts',(96.5750104158968,-1.45901173790498,-6.70807952527345));
#36798=CARTESIAN_POINT('Ctrl Pts',(96.5329347022804,-1.46231459620304,-6.71038169919656));
#36799=CARTESIAN_POINT('Ctrl Pts',(96.4907716762808,-1.46379152747159,-6.71268387311968));
#36800=CARTESIAN_POINT('Ctrl Pts',(96.4486908126069,-1.46345250782874,-6.7149860470428));
#36801=CARTESIAN_POINT('Ctrl Pts',(96.3936694206248,-1.46300923430651,-6.71799617570403));
#36802=CARTESIAN_POINT('Ctrl Pts',(96.3385574561869,-1.45945775804877,-6.72100630436527));
#36803=CARTESIAN_POINT('Ctrl Pts',(96.2837345590264,-1.4527879967247,-6.72401643302651));
#36804=CARTESIAN_POINT('Ctrl Pts',(96.2290090976017,-1.44613008944583,-6.72702121184096));
#36805=CARTESIAN_POINT('Ctrl Pts',(96.1745722039164,-1.43636495864269,-6.7300259906554));
#36806=CARTESIAN_POINT('Ctrl Pts',(96.1208020029894,-1.42353449668251,-6.73303076946985));
#36807=CARTESIAN_POINT('Ctrl Pts',(96.0670849987679,-1.41071672833879,-6.73603257555347));
#36808=CARTESIAN_POINT('Ctrl Pts',(96.0140338918733,-1.39483975832009,-6.73903438163709));
#36809=CARTESIAN_POINT('Ctrl Pts',(95.9620183132523,-1.37599682055892,-6.74203618772071));
#36810=CARTESIAN_POINT('Ctrl Pts',(95.9100336505337,-1.35716508225835,-6.7450362096553));
#36811=CARTESIAN_POINT('Ctrl Pts',(95.8590837917253,-1.33537104981141,-6.74803623158991));
#36812=CARTESIAN_POINT('Ctrl Pts',(95.8095226134042,-1.31075760328414,-6.75103625352451));
#36813=CARTESIAN_POINT('Ctrl Pts',(95.7599713178817,-1.28614906482688,-6.7540356772366));
#36814=CARTESIAN_POINT('Ctrl Pts',(95.7118086256451,-1.25872246358268,-6.75703510094869));
#36815=CARTESIAN_POINT('Ctrl Pts',(95.6653657243524,-1.22866758263416,-6.76003452466078));
#36816=CARTESIAN_POINT('Ctrl Pts',(95.6188801255389,-1.19858507057577,-6.76303670590854));
#36817=CARTESIAN_POINT('Ctrl Pts',(95.5741179208266,-1.16586973885513,-6.7660388871563));
#36818=CARTESIAN_POINT('Ctrl Pts',(95.5313817967113,-1.13075506372699,-6.76904106840406));
#36819=CARTESIAN_POINT('Ctrl Pts',(95.488626220061,-1.09562440517822,-6.77204461617808));
#36820=CARTESIAN_POINT('Ctrl Pts',(95.4478989514394,-1.05809258465265,-6.7750481639521));
#36821=CARTESIAN_POINT('Ctrl Pts',(95.4094674834614,-1.01843160990004,-6.77805171172612));
#36822=CARTESIAN_POINT('Ctrl Pts',(95.3709634825552,-0.978695781732232,
-6.78106092819108));
#36823=CARTESIAN_POINT('Ctrl Pts',(95.3347642842418,-0.936823172417153,
-6.78407014465605));
#36824=CARTESIAN_POINT('Ctrl Pts',(95.301097803588,-0.893119796442088,-6.78707936112102));
#36825=CARTESIAN_POINT('Ctrl Pts',(95.2753415661268,-0.859684922715582,
-6.78938153504414));
#36826=CARTESIAN_POINT('Ctrl Pts',(95.2510668845504,-0.825179243157309,
-6.79168370896725));
#36827=CARTESIAN_POINT('Ctrl Pts',(95.228358003907,-0.789750148308691,-6.79398588289037));
#36828=CARTESIAN_POINT('Ctrl Pts',(95.1986657848254,-0.743426048823991,
-6.7969960115516));
#36829=CARTESIAN_POINT('Ctrl Pts',(95.1715272807514,-0.695327782696951,
-6.80000614021284));
#36830=CARTESIAN_POINT('Ctrl Pts',(95.1471583695683,-0.645767799475315,
-6.80301626887408));
#36831=CARTESIAN_POINT('Ctrl Pts',(95.1228327688067,-0.596295898308325,
-6.80602104768852));
#36832=CARTESIAN_POINT('Ctrl Pts',(95.1012672236512,-0.545367905653447,
-6.80902582650297));
#36833=CARTESIAN_POINT('Ctrl Pts',(95.0826332541428,-0.493323401215417,
-6.81203060531741));
#36834=CARTESIAN_POINT('Ctrl Pts',(95.0640177198601,-0.441330386192153,
-6.81503241140103));
#36835=CARTESIAN_POINT('Ctrl Pts',(95.0483281929976,-0.388223542315368,
-6.81803421748465));
#36836=CARTESIAN_POINT('Ctrl Pts',(95.0356885525259,-0.334363388105666,
-6.82103602356827));
#36837=CARTESIAN_POINT('Ctrl Pts',(95.0230564245323,-0.280535246137478,
-6.82403604550287));
#36838=CARTESIAN_POINT('Ctrl Pts',(95.0134707104046,-0.225955194401009,
-6.82703606743747));
#36839=CARTESIAN_POINT('Ctrl Pts',(95.0070051010148,-0.170997683160566,
-6.83003608937207));
#36840=CARTESIAN_POINT('Ctrl Pts',(95.0005407809065,-0.116051130780047,
-6.83303551308416));
#36841=CARTESIAN_POINT('Ctrl Pts',(94.997195391609,-0.0607277925787329,
-6.83603493679625));
#36842=CARTESIAN_POINT('Ctrl Pts',(94.9969909443191,-0.00540874386480694,
-6.83903436050834));
#36843=CARTESIAN_POINT('Ctrl Pts',(94.9967863090695,0.0499611627019756,
-6.8420365417561));
#36844=CARTESIAN_POINT('Ctrl Pts',(94.9997283869156,0.10532624265535,-6.84503872300386));
#36845=CARTESIAN_POINT('Ctrl Pts',(95.0057870219234,0.160305417399915,-6.84804090425161));
#36846=CARTESIAN_POINT('Ctrl Pts',(95.0118484146874,0.21530961744437,-6.85104445202563));
#36847=CARTESIAN_POINT('Ctrl Pts',(95.0210291047738,0.269927040405136,-6.85404799979965));
#36848=CARTESIAN_POINT('Ctrl Pts',(95.0332474352863,0.323785030051596,-6.85705154757367));
#36849=CARTESIAN_POINT('Ctrl Pts',(95.0454888258415,0.377744667589589,-6.86006076403863));
#36850=CARTESIAN_POINT('Ctrl Pts',(95.0607791632033,0.430941499757943,-6.8630699805036));
#36851=CARTESIAN_POINT('Ctrl Pts',(95.0789866839011,0.483017436439501,-6.86607919696856));
#36852=CARTESIAN_POINT('Ctrl Pts',(95.0929161834379,0.522857662241198,-6.86838137089169));
#36853=CARTESIAN_POINT('Ctrl Pts',(95.108552027997,0.56204212921919,-6.8706835448148));
#36854=CARTESIAN_POINT('Ctrl Pts',(95.1258168051965,0.600419746265118,-6.87298571873793));
#36855=CARTESIAN_POINT('Ctrl Pts',(95.1483907732866,0.650599084958767,-6.87599584739916));
#36856=CARTESIAN_POINT('Ctrl Pts',(95.1738459935429,0.699609016294267,-6.8790059760604));
#36857=CARTESIAN_POINT('Ctrl Pts',(95.2020387358882,0.747098015528137,-6.88201610472164));
#36858=CARTESIAN_POINT('Ctrl Pts',(95.2301813717866,0.794502613429398,-6.88502088353609));
#36859=CARTESIAN_POINT('Ctrl Pts',(95.261051607042,0.840391193152243,-6.88802566235053));
#36860=CARTESIAN_POINT('Ctrl Pts',(95.2944587523897,0.884434557028695,-6.89103044116498));
#36861=CARTESIAN_POINT('Ctrl Pts',(95.3278328469018,0.928434347293419,-6.8940322472486));
#36862=CARTESIAN_POINT('Ctrl Pts',(95.3637385620232,0.970592119309378,-6.89703405333222));
#36863=CARTESIAN_POINT('Ctrl Pts',(95.4019416407734,1.01060713520026,-6.90003585941584));
#36864=CARTESIAN_POINT('Ctrl Pts',(95.4401220131984,1.05059836782555,-6.90303588135044));
#36865=CARTESIAN_POINT('Ctrl Pts',(95.4805966788677,1.08844898739582,-6.90603590328504));
#36866=CARTESIAN_POINT('Ctrl Pts',(95.5230922900105,1.12389267766819,-6.90903592521964));
#36867=CARTESIAN_POINT('Ctrl Pts',(95.5655794272716,1.15932930025439,-6.91203534893172));
#36868=CARTESIAN_POINT('Ctrl Pts',(95.6100863043492,1.1923596086404,-6.91503477264381));
#36869=CARTESIAN_POINT('Ctrl Pts',(95.6563057872485,1.22275694980396,-6.9180341963559));
#36870=CARTESIAN_POINT('Ctrl Pts',(95.702567762268,1.25318223692004,-6.92103637760366));
#36871=CARTESIAN_POINT('Ctrl Pts',(95.7505450465516,1.28096942988863,-6.92403855885142));
#36872=CARTESIAN_POINT('Ctrl Pts',(95.7999019994357,1.30593556526737,-6.92704074009918));
#36873=CARTESIAN_POINT('Ctrl Pts',(95.8492814185092,1.33091306467673,-6.9300442878732));
#36874=CARTESIAN_POINT('Ctrl Pts',(95.9000412731775,1.35306673514891,-6.93304783564722));
#36875=CARTESIAN_POINT('Ctrl Pts',(95.9518248368109,1.37226134863066,-6.93605138342124));
#36876=CARTESIAN_POINT('Ctrl Pts',(96.0037061332057,1.39149218871501,-6.93906059988621));
#36877=CARTESIAN_POINT('Ctrl Pts',(96.0566144921403,1.4077526599331,-6.94206981635118));
#36878=CARTESIAN_POINT('Ctrl Pts',(96.1101780084611,1.42095745870365,-6.94507903281614));
#36879=CARTESIAN_POINT('Ctrl Pts',(96.1511562936526,1.43105967093846,-6.94738120673926));
#36880=CARTESIAN_POINT('Ctrl Pts',(96.1925177034025,1.43937446924748,-6.94968338066238));
#36881=CARTESIAN_POINT('Ctrl Pts',(96.2340933970198,1.44588413299515,-6.9519855545855));
#36882=CARTESIAN_POINT('Ctrl Pts',(96.2884542711968,1.45439562086543,-6.95499568324673));
#36883=CARTESIAN_POINT('Ctrl Pts',(96.3434100401121,1.45985502291366,-6.95800581190796));
#36884=CARTESIAN_POINT('Ctrl Pts',(96.3985877587826,1.46219064520783,-6.9610159405692));
#36885=CARTESIAN_POINT('Ctrl Pts',(96.4536674110997,1.46452211644307,-6.96402071938364));
#36886=CARTESIAN_POINT('Ctrl Pts',(96.508967706973,1.46374080342766,-6.96702549819809));
#36887=CARTESIAN_POINT('Ctrl Pts',(96.5641087426303,1.45982654123937,-6.97003027701254));
#36888=CARTESIAN_POINT('Ctrl Pts',(96.6191952253683,1.45591615156502,-6.97303208309616));
#36889=CARTESIAN_POINT('Ctrl Pts',(96.6741222358115,1.448878989957,-6.97603388917977));
#36890=CARTESIAN_POINT('Ctrl Pts',(96.7285099008003,1.43874693094586,-6.97903569526339));
#36891=CARTESIAN_POINT('Ctrl Pts',(96.7828652400171,1.42862089401031,-6.98203571719799));
#36892=CARTESIAN_POINT('Ctrl Pts',(96.8366813510123,1.41540370216642,-6.98503573913259));
#36893=CARTESIAN_POINT('Ctrl Pts',(96.8895858306163,1.39917877737916,-6.98803576106719));
#36894=CARTESIAN_POINT('Ctrl Pts',(96.9424797607473,1.38295708793995,-6.99103518477928));
#36895=CARTESIAN_POINT('Ctrl Pts',(96.9944619158818,1.36372901141448,-6.99403460849137));
#36896=CARTESIAN_POINT('Ctrl Pts',(97.0451746512045,1.34162793846771,-6.99703403220346));
#36897=CARTESIAN_POINT('Ctrl Pts',(97.0959340095421,1.31950654678549,-7.00003621345122));
#36898=CARTESIAN_POINT('Ctrl Pts',(97.1454211312806,1.29450709314458,-7.00303839469898));
#36899=CARTESIAN_POINT('Ctrl Pts',(97.1932993868719,1.26681071512705,-7.00604057594674));
#36900=CARTESIAN_POINT('Ctrl Pts',(97.2411994355822,1.23910173033309,-7.00904412372076));
#36901=CARTESIAN_POINT('Ctrl Pts',(97.2874887161502,1.20869366453079,-7.01204767149478));
#36902=CARTESIAN_POINT('Ctrl Pts',(97.3318590574115,1.17581139779589,-7.01505121926879));
#36903=CARTESIAN_POINT('Ctrl Pts',(97.3763131402248,1.14286707131635,-7.01806043573376));
#36904=CARTESIAN_POINT('Ctrl Pts',(97.4188406421111,1.10743955443045,-7.02106965219873));
#36905=CARTESIAN_POINT('Ctrl Pts',(97.4591669115095,1.06979371817143,-7.0240788686637));
#36906=CARTESIAN_POINT('Ctrl Pts',(97.4900181603,1.04099311058523,-7.02638104258681));
#36907=CARTESIAN_POINT('Ctrl Pts',(97.5195817395779,1.01089498991801,-7.02868321650993));
#36908=CARTESIAN_POINT('Ctrl Pts',(97.5477505539431,0.97963108230674,-7.03098539043305));
#36909=CARTESIAN_POINT('Ctrl Pts',(97.584188794614,0.939189132032247,-7.03396340599271));
#36910=CARTESIAN_POINT('Ctrl Pts',(97.6184523334827,0.896617035648177,-7.03694142155236));
#36911=CARTESIAN_POINT('Ctrl Pts',(97.6502795702539,0.852180434083894,-7.03991943711201));
#36912=CARTESIAN_POINT('Ctrl Pts',(97.6820603240518,0.80780873119042,-7.04289310334601));
#36913=CARTESIAN_POINT('Ctrl Pts',(97.7114115077978,0.761578348566087,-7.04586676958));
#36914=CARTESIAN_POINT('Ctrl Pts',(97.7381102812762,0.713789563374084,-7.04884043581399));
#36915=CARTESIAN_POINT('Ctrl Pts',(97.7647811609684,0.666050705949744,-7.05181099528316));
#36916=CARTESIAN_POINT('Ctrl Pts',(97.7888048572825,0.616757140291628,-7.05478155475234));
#36917=CARTESIAN_POINT('Ctrl Pts',(97.8100019850866,0.566237781075439,-7.05775211422151));
#36918=CARTESIAN_POINT('Ctrl Pts',(97.8311912990912,0.51573704457758,-7.06072157866704));
#36919=CARTESIAN_POINT('Ctrl Pts',(97.8495558883255,0.4640119020712,-7.06369104311258));
#36920=CARTESIAN_POINT('Ctrl Pts',(97.8649634682578,0.411413544648343,-7.06666050755811));
#36921=CARTESIAN_POINT('Ctrl Pts',(97.880367471045,0.358827398874208,-7.06962928258941));
#36922=CARTESIAN_POINT('Ctrl Pts',(97.892815681147,0.305368960812963,-7.0725980576207));
#36923=CARTESIAN_POINT('Ctrl Pts',(97.9022257719699,0.251404290144893,-7.075566832652));
#36924=CARTESIAN_POINT('Ctrl Pts',(97.9116425082685,0.197401509227816,-7.07853770425415));
#36925=CARTESIAN_POINT('Ctrl Pts',(97.9180167573192,0.142892316245049,-7.08150857585629));
#36926=CARTESIAN_POINT('Ctrl Pts',(97.9213177137636,0.088250769973256,-7.08447944745844));
#36927=CARTESIAN_POINT('Ctrl Pts',(97.9231197467293,0.0584212737836033,
-7.08610128302465));
#36928=CARTESIAN_POINT('Ctrl Pts',(97.924006786112,0.0285524121465811,-7.08772311859086));
#36929=CARTESIAN_POINT('Ctrl Pts',(97.92398037669,-0.00129492856329451,
-7.08934495415707));
#36930=CARTESIAN_POINT('Origin',(96.460480949577,-8.32667268468867E-16,
1.18130019239114E-14));
#36931=CARTESIAN_POINT('',(97.9239808632502,0.000502671547986457,-7.66065504587107));
#36932=CARTESIAN_POINT('',(97.9239808370566,0.000573887927501785,-7.58934495418715));
#36933=CARTESIAN_POINT('',(97.923980949577,-1.01189432752408E-15,1.19922289829666E-14));
#36934=CARTESIAN_POINT('Ctrl Pts',(97.92398086325,0.000502672062914034,
-7.66065504584291));
#36935=CARTESIAN_POINT('Ctrl Pts',(97.9239711281533,0.0288458290411993,
-7.65910533372452));
#36936=CARTESIAN_POINT('Ctrl Pts',(97.9231380787271,0.0571737031003787,
-7.65755562160613));
#36937=CARTESIAN_POINT('Ctrl Pts',(97.9214840360923,0.0854530935234917,
-7.65600590948774));
#36938=CARTESIAN_POINT('Ctrl Pts',(97.918271258001,0.140382394666001,-7.65299578082649));
#36939=CARTESIAN_POINT('Ctrl Pts',(97.9119496588756,0.195245670108786,-7.64998565216525));
#36940=CARTESIAN_POINT('Ctrl Pts',(97.9025282822349,0.249663253952477,-7.646975523504));
#36941=CARTESIAN_POINT('Ctrl Pts',(97.8931236500352,0.303984122416502,-7.64397074468955));
#36942=CARTESIAN_POINT('Ctrl Pts',(97.8806302626854,0.357860355082166,-7.6409659658751));
#36943=CARTESIAN_POINT('Ctrl Pts',(97.8651089962332,0.410916415523629,-7.63796118706064));
#36944=CARTESIAN_POINT('Ctrl Pts',(97.8496030855027,0.463919985783276,-7.63495938097702));
#36945=CARTESIAN_POINT('Ctrl Pts',(97.8310753773326,0.51610448683195,-7.63195757489339));
#36946=CARTESIAN_POINT('Ctrl Pts',(97.8096375965919,0.567105450349019,-7.62895576880977));
#36947=CARTESIAN_POINT('Ctrl Pts',(97.7882125575788,0.618076101008883,-7.62595574687516));
#36948=CARTESIAN_POINT('Ctrl Pts',(97.7638810784644,0.667864122530152,-7.62295572494056));
#36949=CARTESIAN_POINT('Ctrl Pts',(97.7368036741354,0.716123280431402,-7.61995570300596));
#36950=CARTESIAN_POINT('Ctrl Pts',(97.7097316692045,0.764372815164853,-7.61695627929387));
#36951=CARTESIAN_POINT('Ctrl Pts',(97.6799150847523,0.811093631412987,-7.61395685558177));
#36952=CARTESIAN_POINT('Ctrl Pts',(97.6475601369233,0.855964516185827,-7.61095743186968));
#36953=CARTESIAN_POINT('Ctrl Pts',(97.6151754434061,0.900876653238153,-7.60795525062192));
#36954=CARTESIAN_POINT('Ctrl Pts',(97.5802480337135,0.943935031661751,-7.60495306937416));
#36955=CARTESIAN_POINT('Ctrl Pts',(97.5430263268552,0.984849103230332,-7.6019508881264));
#36956=CARTESIAN_POINT('Ctrl Pts',(97.5057876775023,1.02578179797606,-7.59894734035238));
#36957=CARTESIAN_POINT('Ctrl Pts',(97.4662530268612,1.06456786970337,-7.59594379257836));
#36958=CARTESIAN_POINT('Ctrl Pts',(97.4247075047286,1.10095385931496,-7.59294024480434));
#36959=CARTESIAN_POINT('Ctrl Pts',(97.3830835724148,1.13740852135842,-7.58993102833937));
#36960=CARTESIAN_POINT('Ctrl Pts',(97.3394416045668,1.17145372677336,-7.5869218118744));
#36961=CARTESIAN_POINT('Ctrl Pts',(97.2940987020515,1.20287725589913,-7.58391259540943));
#36962=CARTESIAN_POINT('Ctrl Pts',(97.2594095233291,1.22691754351777,-7.58161042148635));
#36963=CARTESIAN_POINT('Ctrl Pts',(97.2237254860201,1.24942424404664,-7.57930824756327));
#36964=CARTESIAN_POINT('Ctrl Pts',(97.1871980350955,1.27032063968725,-7.57700607364019));
#36965=CARTESIAN_POINT('Ctrl Pts',(97.139437817743,1.29764300608345,-7.57399594497896));
#36966=CARTESIAN_POINT('Ctrl Pts',(97.0900342510819,1.32232557501299,-7.57098581631772));
#36967=CARTESIAN_POINT('Ctrl Pts',(97.0393102568641,1.34416847270924,-7.56797568765649));
#36968=CARTESIAN_POINT('Ctrl Pts',(96.9886764134766,1.36597254942163,-7.56497090884205));
#36969=CARTESIAN_POINT('Ctrl Pts',(96.9367272808478,1.38494676331364,-7.56196613002761));
#36970=CARTESIAN_POINT('Ctrl Pts',(96.8838106432748,1.40093690808463,-7.55896135121318));
#36971=CARTESIAN_POINT('Ctrl Pts',(96.8309463579478,1.41691123325652,-7.55595954512956));
#36972=CARTESIAN_POINT('Ctrl Pts',(96.7771169668699,1.42990718554583,-7.55295773904595));
#36973=CARTESIAN_POINT('Ctrl Pts',(96.7226887680985,1.4398191934775,-7.54995593296233));
#36974=CARTESIAN_POINT('Ctrl Pts',(96.6682929191908,1.44972531012279,-7.54695591102774));
#36975=CARTESIAN_POINT('Ctrl Pts',(96.6132994865528,1.45655102104358,-7.54395588909314));
#36976=CARTESIAN_POINT('Ctrl Pts',(96.558086155585,1.46024158061607,-7.54095586715855));
#36977=CARTESIAN_POINT('Ctrl Pts',(96.5028838344892,1.46393140426868,-7.53795644344646));
#36978=CARTESIAN_POINT('Ctrl Pts',(96.4474622287907,1.46448728292819,-7.53495701973437));
#36979=CARTESIAN_POINT('Ctrl Pts',(96.3922030387056,1.46190641864896,-7.53195759602229));
#36980=CARTESIAN_POINT('Ctrl Pts',(96.3368930457988,1.45932318163884,-7.52895541477453));
#36981=CARTESIAN_POINT('Ctrl Pts',(96.2817462954972,1.45359746496226,-7.52595323352677));
#36982=CARTESIAN_POINT('Ctrl Pts',(96.2271418649315,1.44477857181534,-7.52295105227902));
#36983=CARTESIAN_POINT('Ctrl Pts',(96.1725125796411,1.43595566450402,-7.519947504505));
#36984=CARTESIAN_POINT('Ctrl Pts',(96.1184266228099,1.42403688793133,-7.51694395673099));
#36985=CARTESIAN_POINT('Ctrl Pts',(96.0652520670549,1.40912255691983,-7.51394040895697));
#36986=CARTESIAN_POINT('Ctrl Pts',(96.0119771532747,1.39418007761852,-7.51093119249201));
#36987=CARTESIAN_POINT('Ctrl Pts',(95.9596175775726,1.37623092160277,-7.50792197602704));
#36988=CARTESIAN_POINT('Ctrl Pts',(95.9085243422947,1.35542471339334,-7.50491275956208));
#36989=CARTESIAN_POINT('Ctrl Pts',(95.8694359233405,1.3395071114072,-7.50261058563893));
#36990=CARTESIAN_POINT('Ctrl Pts',(95.8310883380211,1.32191834261455,-7.50030841171577));
#36991=CARTESIAN_POINT('Ctrl Pts',(95.7936285884951,1.30274332795046,-7.49800623779262));
#36992=CARTESIAN_POINT('Ctrl Pts',(95.7446493760397,1.2776716942917,-7.49499610913138));
#36993=CARTESIAN_POINT('Ctrl Pts',(95.6969831453964,1.24978133638675,-7.49198598047014));
#36994=CARTESIAN_POINT('Ctrl Pts',(95.6509737394014,1.21923349965204,-7.48897585180891));
#36995=CARTESIAN_POINT('Ctrl Pts',(95.6050461050849,1.18873995503065,-7.48597107299446));
#36996=CARTESIAN_POINT('Ctrl Pts',(95.5607698881623,1.15559859433539,-7.48296629418001));
#36997=CARTESIAN_POINT('Ctrl Pts',(95.5184642685352,1.12001643855746,-7.47996151536557));
#36998=CARTESIAN_POINT('Ctrl Pts',(95.4762005033097,1.08446948542766,-7.47695970928195));
#36999=CARTESIAN_POINT('Ctrl Pts',(95.4359038755366,1.04648685900662,-7.47395790319833));
#37000=CARTESIAN_POINT('Ctrl Pts',(95.3978629479879,1.00631765993588,-7.47095609711471));
#37001=CARTESIAN_POINT('Ctrl Pts',(95.3598446303887,0.966172335770845,-7.46795607518011));
#37002=CARTESIAN_POINT('Ctrl Pts',(95.3240797180821,0.923843397553606,-7.46495605324551));
#37003=CARTESIAN_POINT('Ctrl Pts',(95.2908204278217,0.879617254177741,-7.46195603131091));
#37004=CARTESIAN_POINT('Ctrl Pts',(95.2575677696649,0.835399929762189,-7.45895660759881));
#37005=CARTESIAN_POINT('Ctrl Pts',(95.2268200585374,0.789286573348786,-7.45595718388672));
#37006=CARTESIAN_POINT('Ctrl Pts',(95.1987881972936,0.741595340354497,-7.45295776017463));
#37007=CARTESIAN_POINT('Ctrl Pts',(95.1707305648135,0.693860262179053,-7.44995557892687));
#37008=CARTESIAN_POINT('Ctrl Pts',(95.145394038746,0.644544865525138,-7.44695339767911));
#37009=CARTESIAN_POINT('Ctrl Pts',(95.1229444525937,0.593993576764662,-7.44395121643135));
#37010=CARTESIAN_POINT('Ctrl Pts',(95.1004846478881,0.543419278179704,-7.44094766865733));
#37011=CARTESIAN_POINT('Ctrl Pts',(95.0809145895451,0.491608460990693,-7.43794412088331));
#37012=CARTESIAN_POINT('Ctrl Pts',(95.064351374634,0.438924207545438,-7.43494057310929));
#37013=CARTESIAN_POINT('Ctrl Pts',(95.0477568994422,0.386140521438198,-7.43193135664432));
#37014=CARTESIAN_POINT('Ctrl Pts',(95.0341807340498,0.332480619252014,-7.42892214017936));
#37015=CARTESIAN_POINT('Ctrl Pts',(95.0236893501979,0.278320229149122,-7.42591292371439));
#37016=CARTESIAN_POINT('Ctrl Pts',(95.0156630115804,0.236885311052697,-7.42361074979128));
#37017=CARTESIAN_POINT('Ctrl Pts',(95.0094411087291,0.195157742080686,-7.42130857586817));
#37018=CARTESIAN_POINT('Ctrl Pts',(95.0050328394778,0.153307040962721,-7.41900640194506));
#37019=CARTESIAN_POINT('Ctrl Pts',(94.9992689580063,0.0985865901473129,
-7.41599627328382));
#37020=CARTESIAN_POINT('Ctrl Pts',(94.9965832420588,0.0434256570727678,
-7.41298614462259));
#37021=CARTESIAN_POINT('Ctrl Pts',(94.9970285186357,-0.0117996767691671,
-7.40997601596135));
#37022=CARTESIAN_POINT('Ctrl Pts',(94.9974730038305,-0.0669268596320551,
-7.4069712371469));
#37023=CARTESIAN_POINT('Ctrl Pts',(95.001037434229,-0.122117692291472,-7.40396645833246));
#37024=CARTESIAN_POINT('Ctrl Pts',(95.0077228228246,-0.176991737532955,
-7.40096167951802));
#37025=CARTESIAN_POINT('Ctrl Pts',(95.0144015973358,-0.231811493997847,
-7.3979598734344));
#37026=CARTESIAN_POINT('Ctrl Pts',(95.0241951499612,-0.286314562229797,
-7.39495806735078));
#37027=CARTESIAN_POINT('Ctrl Pts',(95.0370525217755,-0.340123155528405,
-7.39195626126716));
#37028=CARTESIAN_POINT('Ctrl Pts',(95.0499022517013,-0.393899767231153,
-7.38895623933256));
#37029=CARTESIAN_POINT('Ctrl Pts',(95.0658120689693,-0.446982209501575,
-7.38595621739796));
#37030=CARTESIAN_POINT('Ctrl Pts',(95.0846799086669,-0.499002751325654,
-7.38295619546336));
#37031=CARTESIAN_POINT('Ctrl Pts',(95.1035439860032,-0.55101291993925,-7.37995677175127));
#37032=CARTESIAN_POINT('Ctrl Pts',(95.1253647343889,-0.601961112440803,
-7.37695734803918));
#37033=CARTESIAN_POINT('Ctrl Pts',(95.1499909265914,-0.65149685314294,-7.37395792432708));
#37034=CARTESIAN_POINT('Ctrl Pts',(95.1746397590108,-0.701078134783912,
-7.37095574307932));
#37035=CARTESIAN_POINT('Ctrl Pts',(95.2020989525488,-0.749243896384251,
-7.36795356183157));
#37036=CARTESIAN_POINT('Ctrl Pts',(95.2321706516241,-0.795667054705019,
-7.36495138058381));
#37037=CARTESIAN_POINT('Ctrl Pts',(95.2622560386694,-0.842111343816925,
-7.36194783280979));
#37038=CARTESIAN_POINT('Ctrl Pts',(95.2949559893923,-0.886811021489771,
-7.35894428503577));
#37039=CARTESIAN_POINT('Ctrl Pts',(95.3300303939341,-0.929469629007074,
-7.35594073726175));
#37040=CARTESIAN_POINT('Ctrl Pts',(95.3651709955116,-0.972208747466919,
-7.35293152079679));
#37041=CARTESIAN_POINT('Ctrl Pts',(95.4026946442625,-1.01289871126401,-7.34992230433182));
#37042=CARTESIAN_POINT('Ctrl Pts',(95.4423229776373,-1.05127855213337,-7.34691308786686));
#37043=CARTESIAN_POINT('Ctrl Pts',(95.4726402767663,-1.0806407033284,-7.34461091394374));
#37044=CARTESIAN_POINT('Ctrl Pts',(95.5041886154988,-1.10865149429615,-7.34230874002061));
#37045=CARTESIAN_POINT('Ctrl Pts',(95.5368310429968,-1.13521059723487,-7.34000656609749));
#37046=CARTESIAN_POINT('Ctrl Pts',(95.5795115310335,-1.16993704260449,-7.33699643743626));
#37047=CARTESIAN_POINT('Ctrl Pts',(95.6242428323756,-1.20232611928237,-7.33398630877502));
#37048=CARTESIAN_POINT('Ctrl Pts',(95.6707388331178,-1.23212809378348,-7.33097618011378));
#37049=CARTESIAN_POINT('Ctrl Pts',(95.7171521973655,-1.26187710177862,-7.32797140129934));
#37050=CARTESIAN_POINT('Ctrl Pts',(95.7653235958424,-1.2890478496978,-7.32496662248489));
#37051=CARTESIAN_POINT('Ctrl Pts',(95.8149349556383,-1.31343161973118,-7.32196184367045));
#37052=CARTESIAN_POINT('Ctrl Pts',(95.864497233213,-1.33779126606386,-7.31896003758683));
#37053=CARTESIAN_POINT('Ctrl Pts',(95.9154961784037,-1.35936916469073,-7.31595823150321));
#37054=CARTESIAN_POINT('Ctrl Pts',(95.9675875409249,-1.37800157391323,-7.31295642541959));
#37055=CARTESIAN_POINT('Ctrl Pts',(96.019647942501,-1.39662290880455,-7.30995640348499));
#37056=CARTESIAN_POINT('Ctrl Pts',(96.0727989782063,-1.41230204673811,-7.30695638155039));
#37057=CARTESIAN_POINT('Ctrl Pts',(96.1266768955525,-1.42492354304251,-7.30395635961579));
#37058=CARTESIAN_POINT('Ctrl Pts',(96.1805440693163,-1.43754252254425,-7.3009569359037));
#37059=CARTESIAN_POINT('Ctrl Pts',(96.23513732296,-1.44710495089071,-7.29795751219161));
#37060=CARTESIAN_POINT('Ctrl Pts',(96.2900804936969,-1.45354598641937,-7.29495808847952));
#37061=CARTESIAN_POINT('Ctrl Pts',(96.3450741767213,-1.45999294354728,-7.29195590723176));
#37062=CARTESIAN_POINT('Ctrl Pts',(96.4004178938987,-1.46331271300988,-7.288953725984));
#37063=CARTESIAN_POINT('Ctrl Pts',(96.4557295967009,-1.46349228718359,-7.28595154473624));
#37064=CARTESIAN_POINT('Ctrl Pts',(96.5110664761623,-1.46367194309547,-7.28294799696222));
#37065=CARTESIAN_POINT('Ctrl Pts',(96.5663707839206,-1.46070858272003,-7.2799444491882));
#37066=CARTESIAN_POINT('Ctrl Pts',(96.6212630327378,-1.45464132064728,-7.27694090141418));
#37067=CARTESIAN_POINT('Ctrl Pts',(96.6762588814367,-1.44856260763845,-7.27393168494921));
#37068=CARTESIAN_POINT('Ctrl Pts',(96.7308405955774,-1.43936837842359,-7.27092246848425));
#37069=CARTESIAN_POINT('Ctrl Pts',(96.7846375110102,-1.4271491770939,-7.26791325201928));
#37070=CARTESIAN_POINT('Ctrl Pts',(96.8257943560879,-1.41780098729431,-7.26561107809616));
#37071=CARTESIAN_POINT('Ctrl Pts',(96.8664920358128,-1.40668339077259,-7.26330890417304));
#37072=CARTESIAN_POINT('Ctrl Pts',(96.9065716935508,-1.39385626882433,-7.26100673024993));
#37073=CARTESIAN_POINT('Ctrl Pts',(96.9589764772547,-1.37708460486363,-7.25799660158869));
#37074=CARTESIAN_POINT('Ctrl Pts',(97.0105442081131,-1.35731820048866,-7.25498647292745));
#37075=CARTESIAN_POINT('Ctrl Pts',(97.0609093960967,-1.33466023039945,-7.25197634426622));
#37076=CARTESIAN_POINT('Ctrl Pts',(97.1111850709499,-1.31204252990742,-7.24897156545177));
#37077=CARTESIAN_POINT('Ctrl Pts',(97.1602619666023,-1.28654367725036,-7.24596678663733));
#37078=CARTESIAN_POINT('Ctrl Pts',(97.2077914824816,-1.25831602445883,-7.24296200782288));
#37079=CARTESIAN_POINT('Ctrl Pts',(97.2552739757793,-1.23011629825316,-7.23996020173926));
#37080=CARTESIAN_POINT('Ctrl Pts',(97.301211670054,-1.19919338822766,-7.23695839565564));
#37081=CARTESIAN_POINT('Ctrl Pts',(97.3452793302217,-1.16574614544011,-7.23395658957202));
#37082=CARTESIAN_POINT('Ctrl Pts',(97.3893207984002,-1.13231878230627,-7.23095656763743));
#37083=CARTESIAN_POINT('Ctrl Pts',(97.4314940156502,-1.09637037886917,-7.22795654570282));
#37084=CARTESIAN_POINT('Ctrl Pts',(97.4715035410207,-1.0581425091123,-7.22495652376823));
#37085=CARTESIAN_POINT('Ctrl Pts',(97.51150508825,-1.01992226222374,-7.22195710005614));
#37086=CARTESIAN_POINT('Ctrl Pts',(97.5493434188221,-0.979423816342423,
-7.21895767634405));
#37087=CARTESIAN_POINT('Ctrl Pts',(97.5847586922295,-0.936926788695987,
-7.21595825263196));
#37088=CARTESIAN_POINT('Ctrl Pts',(97.6202065248513,-0.894390691187875,
-7.2129560713842));
#37089=CARTESIAN_POINT('Ctrl Pts',(97.6532265109286,-0.849852747592014,
-7.20995389013644));
#37090=CARTESIAN_POINT('Ctrl Pts',(97.6835990064107,-0.8036258265184,-7.20695170888868));
#37091=CARTESIAN_POINT('Ctrl Pts',(97.7139853267784,-0.757377863976492,
-7.20394816111467));
#37092=CARTESIAN_POINT('Ctrl Pts',(97.7417214893671,-0.709439849351401,
-7.20094461334065));
#37093=CARTESIAN_POINT('Ctrl Pts',(97.7666329033613,-0.660150985476467,
-7.19794106556663));
#37094=CARTESIAN_POINT('Ctrl Pts',(97.791591333457,-0.610769097165929,-7.19493184910166));
#37095=CARTESIAN_POINT('Ctrl Pts',(97.8137141533856,-0.560031751868831,
-7.1919226326367));
#37096=CARTESIAN_POINT('Ctrl Pts',(97.8328746668239,-0.508298863722117,
-7.18891341617173));
#37097=CARTESIAN_POINT('Ctrl Pts',(97.8475332448641,-0.468721084108819,
-7.18661124224861));
#37098=CARTESIAN_POINT('Ctrl Pts',(97.8604590110083,-0.428561070948875,
-7.18430906832549));
#37099=CARTESIAN_POINT('Ctrl Pts',(97.8716153188119,-0.387984589853705,
-7.18200689440237));
#37100=CARTESIAN_POINT('Ctrl Pts',(97.8898814412655,-0.321549082204936,
-7.17823756573832));
#37101=CARTESIAN_POINT('Ctrl Pts',(97.9034650875488,-0.253774761264491,
-7.17446823707427));
#37102=CARTESIAN_POINT('Ctrl Pts',(97.9122095811533,-0.185246404179905,
-7.17069890841022));
#37103=CARTESIAN_POINT('Ctrl Pts',(97.919976524955,-0.124378854568375,-7.16735095423151));
#37104=CARTESIAN_POINT('Ctrl Pts',(97.9239263130642,-0.0629165758066123,
-7.1640030000528));
#37105=CARTESIAN_POINT('Ctrl Pts',(97.9239803863197,-0.00128399919637083,
-7.16065504587409));
#37106=CARTESIAN_POINT('Ctrl Pts',(97.9239803766892,-0.00129492944525746,
-7.08934495420499));
#37107=CARTESIAN_POINT('Ctrl Pts',(97.923918208247,-0.0715562706037072,
-7.0931627932256));
#37108=CARTESIAN_POINT('Ctrl Pts',(97.9187924004044,-0.141595414215573,
-7.0969806322462));
#37109=CARTESIAN_POINT('Ctrl Pts',(97.9087212224606,-0.210789852692321,
-7.1007984712668));
#37110=CARTESIAN_POINT('Ctrl Pts',(97.900643228254,-0.266290041077624,-7.10386072293807));
#37111=CARTESIAN_POINT('Ctrl Pts',(97.8893846145948,-0.321247370882346,
-7.10692297460935));
#37112=CARTESIAN_POINT('Ctrl Pts',(97.8750281893846,-0.375350977556835,
-7.10998522628062));
#37113=CARTESIAN_POINT('Ctrl Pts',(97.8609161268772,-0.428533679244946,
-7.11299535494185));
#37114=CARTESIAN_POINT('Ctrl Pts',(97.8437709800176,-0.48103116058418,-7.11600548360309));
#37115=CARTESIAN_POINT('Ctrl Pts',(97.8236773919737,-0.532473200674981,
-7.11901561226433));
#37116=CARTESIAN_POINT('Ctrl Pts',(97.8036195158975,-0.583823813765773,
-7.12202039107877));
#37117=CARTESIAN_POINT('Ctrl Pts',(97.7806237884638,-0.634122220236565,
-7.12502516989322));
#37118=CARTESIAN_POINT('Ctrl Pts',(97.7548248181123,-0.683012591381024,
-7.12802994870766));
#37119=CARTESIAN_POINT('Ctrl Pts',(97.7290513715678,-0.731854593603062,
-7.13103175479128));
#37120=CARTESIAN_POINT('Ctrl Pts',(97.7004804212265,-0.779290855221356,
-7.1340335608749));
#37121=CARTESIAN_POINT('Ctrl Pts',(97.6692941919306,-0.824986542381567,
-7.13703536695852));
#37122=CARTESIAN_POINT('Ctrl Pts',(97.6381264984357,-0.870655069920795,
-7.14003538889312));
#37123=CARTESIAN_POINT('Ctrl Pts',(97.6043469040442,-0.914584638159508,
-7.14303541082771));
#37124=CARTESIAN_POINT('Ctrl Pts',(97.5681818023395,-0.956468018696541,
-7.14603543276231));
#37125=CARTESIAN_POINT('Ctrl Pts',(97.5320239121746,-0.998343047434352,
-7.1490348564744));
#37126=CARTESIAN_POINT('Ctrl Pts',(97.4934818043415,-1.03817229928613,-7.15203428018649));
#37127=CARTESIAN_POINT('Ctrl Pts',(97.4528216597379,-1.07568218585111,-7.15503370389859));
#37128=CARTESIAN_POINT('Ctrl Pts',(97.4121241340205,-1.11322655732384,-7.15803588514634));
#37129=CARTESIAN_POINT('Ctrl Pts',(97.3693050702268,-1.14844694454677,-7.1610380663941));
#37130=CARTESIAN_POINT('Ctrl Pts',(97.3246658821713,-1.1811082305517,-7.16404024764186));
#37131=CARTESIAN_POINT('Ctrl Pts',(97.2800063753483,-1.21378438324898,-7.16704379541587));
#37132=CARTESIAN_POINT('Ctrl Pts',(97.2335255367407,-1.24389882502807,-7.17004734318989));
#37133=CARTESIAN_POINT('Ctrl Pts',(97.1855533492081,-1.27126010921966,-7.17305089096391));
#37134=CARTESIAN_POINT('Ctrl Pts',(97.137490622245,-1.29867303323045,-7.17606010742887));
#37135=CARTESIAN_POINT('Ctrl Pts',(97.0879313976346,-1.32332218383262,-7.17906932389384));
#37136=CARTESIAN_POINT('Ctrl Pts',(97.0372287545369,-1.34506290539661,-7.1820785403588));
#37137=CARTESIAN_POINT('Ctrl Pts',(96.9984391546088,-1.36169544839816,-7.18438071428192));
#37138=CARTESIAN_POINT('Ctrl Pts',(96.9589808206018,-1.3766266896331,-7.18668288820505));
#37139=CARTESIAN_POINT('Ctrl Pts',(96.9190174629403,-1.38981168361495,-7.18898506212817));
#37140=CARTESIAN_POINT('Ctrl Pts',(96.8667647434183,-1.40705127089564,-7.19199519078941));
#37141=CARTESIAN_POINT('Ctrl Pts',(96.8134286489963,-1.42137616669333,-7.19500531945064));
#37142=CARTESIAN_POINT('Ctrl Pts',(96.7593654983363,-1.43265497469313,-7.19801544811188));
#37143=CARTESIAN_POINT('Ctrl Pts',(96.7053984331283,-1.44391373707309,-7.20102022692632));
#37144=CARTESIAN_POINT('Ctrl Pts',(96.6507073888337,-1.4521370483083,-7.20402500574077));
#37145=CARTESIAN_POINT('Ctrl Pts',(96.5956639310935,-1.45724322318147,-7.20702978455521));
#37146=CARTESIAN_POINT('Ctrl Pts',(96.5406749297354,-1.46234434634056,-7.21003159063883));
#37147=CARTESIAN_POINT('Ctrl Pts',(96.485334728873,-1.46433439363332,-7.21303339672245));
#37148=CARTESIAN_POINT('Ctrl Pts',(96.4300233278089,-1.4631830313656,-7.21603520280607));
#37149=CARTESIAN_POINT('Ctrl Pts',(96.3747448015473,-1.46203235341986,-7.21903522474067));
#37150=CARTESIAN_POINT('Ctrl Pts',(96.3194955681037,-1.457743977644,-7.22203524667527));
#37151=CARTESIAN_POINT('Ctrl Pts',(96.2646566400979,-1.45033964636461,-7.22503526860987));
#37152=CARTESIAN_POINT('Ctrl Pts',(96.2098286473058,-1.44293679155364,-7.22803469232196));
#37153=CARTESIAN_POINT('Ctrl Pts',(96.1554113205392,-1.43241928581964,-7.23103411603405));
#37154=CARTESIAN_POINT('Ctrl Pts',(96.1017792376444,-1.41886057519992,-7.23403353974614));
#37155=CARTESIAN_POINT('Ctrl Pts',(96.0480978478174,-1.40528939930961,-7.2370357209939));
#37156=CARTESIAN_POINT('Ctrl Pts',(95.9952036572684,-1.3886715623126,-7.24003790224166));
#37157=CARTESIAN_POINT('Ctrl Pts',(95.9434582741108,-1.3691310394019,-7.24304008348942));
#37158=CARTESIAN_POINT('Ctrl Pts',(95.8916893376034,-1.34958162207895,-7.24604363126344));
#37159=CARTESIAN_POINT('Ctrl Pts',(95.8410707343959,-1.32710708157954,-7.24904717903746));
#37160=CARTESIAN_POINT('Ctrl Pts',(95.7919431075654,-1.30187918172096,-7.25205072681147));
#37161=CARTESIAN_POINT('Ctrl Pts',(95.7427227606071,-1.27660366844707,-7.25505994327644));
#37162=CARTESIAN_POINT('Ctrl Pts',(95.6949994678199,-1.24856468317754,-7.25806915974141));
#37163=CARTESIAN_POINT('Ctrl Pts',(95.6490873032538,-1.21797889994298,-7.26107837620637));
#37164=CARTESIAN_POINT('Ctrl Pts',(95.6139626157317,-1.19457952226423,-7.26338055012949));
#37165=CARTESIAN_POINT('Ctrl Pts',(95.5798974205506,-1.16969047719016,-7.26568272405262));
#37166=CARTESIAN_POINT('Ctrl Pts',(95.5470188114984,-1.14342431856985,-7.26798489797574));
#37167=CARTESIAN_POINT('Ctrl Pts',(95.5040295123601,-1.10908090251014,-7.27099502663698));
#37168=CARTESIAN_POINT('Ctrl Pts',(95.4628893939892,-1.0722375548306,-7.27400515529821));
#37169=CARTESIAN_POINT('Ctrl Pts',(95.4239031954539,-1.03312090756948,-7.27701528395945));
#37170=CARTESIAN_POINT('Ctrl Pts',(95.3849862863786,-0.994073781612414,
-7.2800200627739));
#37171=CARTESIAN_POINT('Ctrl Pts',(95.348216069999,-0.95276174509638,-7.28302484158834));
#37172=CARTESIAN_POINT('Ctrl Pts',(95.3138639818906,-0.909451361763583,
-7.28602962040278));
#37173=CARTESIAN_POINT('Ctrl Pts',(95.2795458794822,-0.866183826879712,
-7.2890314264864));
#37174=CARTESIAN_POINT('Ctrl Pts',(95.2476414928095,-0.820922273318624,
-7.29203323257002));
#37175=CARTESIAN_POINT('Ctrl Pts',(95.218383857285,-0.773968386511854,-7.29503503865364));
#37176=CARTESIAN_POINT('Ctrl Pts',(95.1891436112855,-0.727042407147746,
-7.29803506058824));
#37177=CARTESIAN_POINT('Ctrl Pts',(95.1625472771441,-0.678426535530184,
-7.30103508252284));
#37178=CARTESIAN_POINT('Ctrl Pts',(95.138784828877,-0.628451759904116,-7.30403510445744));
#37179=CARTESIAN_POINT('Ctrl Pts',(95.1150271189857,-0.578486949550379,
-7.30703452816953));
#37180=CARTESIAN_POINT('Ctrl Pts',(95.094102399371,-0.527164250007825,-7.31003395188162));
#37181=CARTESIAN_POINT('Ctrl Pts',(95.0761538248649,-0.474837510930137,
-7.31303337559372));
#37182=CARTESIAN_POINT('Ctrl Pts',(95.0581887492442,-0.422462664994863,
-7.31603555684147));
#37183=CARTESIAN_POINT('Ctrl Pts',(95.0432054568902,-0.369082435972016,
-7.31903773808924));
#37184=CARTESIAN_POINT('Ctrl Pts',(95.0312976964958,-0.315067419947357,
-7.322039919337));
#37185=CARTESIAN_POINT('Ctrl Pts',(95.0193845159533,-0.261027817486447,
-7.32504346711101));
#37186=CARTESIAN_POINT('Ctrl Pts',(95.0105497423939,-0.206353374302305,
-7.32804701488503));
#37187=CARTESIAN_POINT('Ctrl Pts',(95.0048356450383,-0.15142323921522,-7.33105056265905));
#37188=CARTESIAN_POINT('Ctrl Pts',(94.9991107632855,-0.0963894327425316,
-7.33405977912402));
#37189=CARTESIAN_POINT('Ctrl Pts',(94.9965183482246,-0.0410994991782647,
-7.33706899558898));
#37190=CARTESIAN_POINT('Ctrl Pts',(94.9970485383513,0.0140651261685238,
-7.34007821205395));
#37191=CARTESIAN_POINT('Ctrl Pts',(94.9974541555272,0.0562683253835064,
-7.34238038597707));
#37192=CARTESIAN_POINT('Ctrl Pts',(94.9996863116939,0.0983981196657594,
-7.34468255990019));
#37193=CARTESIAN_POINT('Ctrl Pts',(95.0037201835205,0.140286565566228,-7.34698473382331));
#37194=CARTESIAN_POINT('Ctrl Pts',(95.0089945344629,0.195056368279004,-7.34999486248454));
#37195=CARTESIAN_POINT('Ctrl Pts',(95.0173730305296,0.249643385155405,-7.35300499114578));
#37196=CARTESIAN_POINT('Ctrl Pts',(95.0288323695198,0.303668558168467,-7.35601511980702));
#37197=CARTESIAN_POINT('Ctrl Pts',(95.0402713420357,0.35759771322645,-7.35901989862146));
#37198=CARTESIAN_POINT('Ctrl Pts',(95.054780182562,0.410966493616192,-7.3620246774359));
#37199=CARTESIAN_POINT('Ctrl Pts',(95.0722839481235,0.463401915355771,-7.36502945625035));
#37200=CARTESIAN_POINT('Ctrl Pts',(95.0897703966089,0.515785460932704,-7.36803126233397));
#37201=CARTESIAN_POINT('Ctrl Pts',(95.110245734204,0.567236978598275,-7.37103306841759));
#37202=CARTESIAN_POINT('Ctrl Pts',(95.1335846208753,0.617396455187357,-7.37403487450121));
#37203=CARTESIAN_POINT('Ctrl Pts',(95.1569096358805,0.667526119064179,-7.37703489643581));
#37204=CARTESIAN_POINT('Ctrl Pts',(95.1830946041882,0.716364786097731,-7.38003491837041));
#37205=CARTESIAN_POINT('Ctrl Pts',(95.2119661152921,0.763572497259179,-7.38303494030501));
#37206=CARTESIAN_POINT('Ctrl Pts',(95.2408318692422,0.81077079491767,-7.3860343640171));
#37207=CARTESIAN_POINT('Ctrl Pts',(95.2723828266986,0.85633833229758,-7.38903378772919));
#37208=CARTESIAN_POINT('Ctrl Pts',(95.3064008482915,0.899961871312809,-7.39203321144128));
#37209=CARTESIAN_POINT('Ctrl Pts',(95.3404501445281,0.943625515853741,-7.39503539268904));
#37210=CARTESIAN_POINT('Ctrl Pts',(95.3769707108299,0.985341174032579,-7.3980375739368));
#37211=CARTESIAN_POINT('Ctrl Pts',(95.4157033869191,1.02482783654945,-7.40103975518456));
#37212=CARTESIAN_POINT('Ctrl Pts',(95.4544536932627,1.06433247251854,-7.40404330295858));
#37213=CARTESIAN_POINT('Ctrl Pts',(95.4954177252884,1.10160573426926,-7.4070468507326));
#37214=CARTESIAN_POINT('Ctrl Pts',(95.5383010313913,1.13640505476484,-7.41005039850662));
#37215=CARTESIAN_POINT('Ctrl Pts',(95.5812652725176,1.17127005312137,-7.41305961497158));
#37216=CARTESIAN_POINT('Ctrl Pts',(95.6261555944798,1.20365147315702,-7.41606883143655));
#37217=CARTESIAN_POINT('Ctrl Pts',(95.6726471466537,1.2333491593914,-7.41907804790152));
#37218=CARTESIAN_POINT('Ctrl Pts',(95.7082150894409,1.25606910646787,-7.42138022182463));
#37219=CARTESIAN_POINT('Ctrl Pts',(95.7447195673557,1.27721916981486,-7.42368239574775));
#37220=CARTESIAN_POINT('Ctrl Pts',(95.7820063598691,1.29672837599889,-7.42598456967087));
#37221=CARTESIAN_POINT('Ctrl Pts',(95.8307594283072,1.32223697033352,-7.4289946983321));
#37222=CARTESIAN_POINT('Ctrl Pts',(95.8810555013984,1.34504588612142,-7.43200482699334));
#37223=CARTESIAN_POINT('Ctrl Pts',(95.9325643756122,1.36496752376505,-7.43501495565458));
#37224=CARTESIAN_POINT('Ctrl Pts',(95.983981704043,1.38485375504527,-7.43801973446902));
#37225=CARTESIAN_POINT('Ctrl Pts',(96.0366070674375,1.4018627027287,-7.44102451328347));
#37226=CARTESIAN_POINT('Ctrl Pts',(96.0900871331254,1.41585333659049,-7.44402929209791));
#37227=CARTESIAN_POINT('Ctrl Pts',(96.1435142891485,1.42983012903794,-7.44703109818153));
#37228=CARTESIAN_POINT('Ctrl Pts',(96.1977939639886,1.44079439002421,-7.45003290426515));
#37229=CARTESIAN_POINT('Ctrl Pts',(96.2525561516286,1.44865438542052,-7.45303471034876));
#37230=CARTESIAN_POINT('Ctrl Pts',(96.3072857908958,1.45650970916161,-7.45603473228336));
#37231=CARTESIAN_POINT('Ctrl Pts',(96.3624968528197,1.46126434943482,-7.45903475421796));
#37232=CARTESIAN_POINT('Ctrl Pts',(96.4178098617443,1.4628777899275,-7.46203477615256));
#37233=CARTESIAN_POINT('Ctrl Pts',(96.4731118409207,1.4644909086904,-7.46503419986465));
#37234=CARTESIAN_POINT('Ctrl Pts',(96.5285151991299,1.46296405623551,-7.46803362357674));
#37235=CARTESIAN_POINT('Ctrl Pts',(96.5836384005495,1.45830877809535,-7.47103304728883));
#37236=CARTESIAN_POINT('Ctrl Pts',(96.6388122797687,1.45364922010121,-7.47403522853659));
#37237=CARTESIAN_POINT('Ctrl Pts',(96.6937049602461,1.44585553481708,-7.47703740978434));
#37238=CARTESIAN_POINT('Ctrl Pts',(96.7479394849717,1.43499123357209,-7.4800395910321));
#37239=CARTESIAN_POINT('Ctrl Pts',(96.802198696049,1.42412198713835,-7.48304313880612));
#37240=CARTESIAN_POINT('Ctrl Pts',(96.8557986421881,1.41017947175455,-7.48604668658014));
#37241=CARTESIAN_POINT('Ctrl Pts',(96.9083752797664,1.39327776088768,-7.48905023435416));
#37242=CARTESIAN_POINT('Ctrl Pts',(96.9610511468999,1.37634415088598,-7.49205945081912));
#37243=CARTESIAN_POINT('Ctrl Pts',(97.012699353357,1.35644037890279,-7.49506866728409));
#37244=CARTESIAN_POINT('Ctrl Pts',(97.0629747664302,1.33372915190965,-7.49807788374906));
#37245=CARTESIAN_POINT('Ctrl Pts',(97.1014375178803,1.31635413248035,-7.50038005767218));
#37246=CARTESIAN_POINT('Ctrl Pts',(97.1390971685741,1.29733696136971,-7.5026822315953));
#37247=CARTESIAN_POINT('Ctrl Pts',(97.1758100108592,1.27676802281589,-7.50498440551843));
#37248=CARTESIAN_POINT('Ctrl Pts',(97.2238126303345,1.24987381171822,-7.50799453417966));
#37249=CARTESIAN_POINT('Ctrl Pts',(97.2703972880558,1.22021219893684,-7.5110046628409));
#37250=CARTESIAN_POINT('Ctrl Pts',(97.3152264423986,1.18795723513143,-7.51401479150214));
#37251=CARTESIAN_POINT('Ctrl Pts',(97.3599759227027,1.15575959748515,-7.51701957031658));
#37252=CARTESIAN_POINT('Ctrl Pts',(97.4029756661203,1.12097806158275,-7.52002434913103));
#37253=CARTESIAN_POINT('Ctrl Pts',(97.4439144964584,1.08383149468368,-7.52302912794547));
#37254=CARTESIAN_POINT('Ctrl Pts',(97.4848128246064,1.04672167815837,-7.52603093402909));
#37255=CARTESIAN_POINT('Ctrl Pts',(97.5236538895144,1.0072518188157,-7.52903274011271));
#37256=CARTESIAN_POINT('Ctrl Pts',(97.5601586915457,0.965681683485103,-7.53203454619633));
#37257=CARTESIAN_POINT('Ctrl Pts',(97.5966417966368,0.924136255718623,-7.53503456813093));
#37258=CARTESIAN_POINT('Ctrl Pts',(97.6307910433249,0.880493422245896,-7.53803459006553));
#37259=CARTESIAN_POINT('Ctrl Pts',(97.6623651540989,0.835048866187381,-7.54103461200013));
#37260=CARTESIAN_POINT('Ctrl Pts',(97.6939329688043,0.789613372048033,-7.54403403571222));
#37261=CARTESIAN_POINT('Ctrl Pts',(97.7229263662146,0.742377302293105,-7.54703345942431));
#37262=CARTESIAN_POINT('Ctrl Pts',(97.7491465463483,0.693666511875963,-7.5500328831364));
#37263=CARTESIAN_POINT('Ctrl Pts',(97.7753908321398,0.644910938942282,-7.55303506438416));
#37264=CARTESIAN_POINT('Ctrl Pts',(97.7988565560888,0.594678402674946,-7.55603724563191));
#37265=CARTESIAN_POINT('Ctrl Pts',(97.8193909428121,0.543319317055657,-7.55903942687967));
#37266=CARTESIAN_POINT('Ctrl Pts',(97.8399346763324,0.491936853920694,-7.56204297465369));
#37267=CARTESIAN_POINT('Ctrl Pts',(97.8575442446221,0.439427320824427,-7.56504652242771));
#37268=CARTESIAN_POINT('Ctrl Pts',(97.8721162752737,0.386157943392706,-7.56805007020172));
#37269=CARTESIAN_POINT('Ctrl Pts',(97.8867158081807,0.332788028975941,-7.57105928666669));
#37270=CARTESIAN_POINT('Ctrl Pts',(97.898266240733,0.278655923186091,-7.57406850313166));
#37271=CARTESIAN_POINT('Ctrl Pts',(97.9067152652418,0.224139586404613,-7.57707771959663));
#37272=CARTESIAN_POINT('Ctrl Pts',(97.9131791152594,0.182432354510986,-7.57937989351975));
#37273=CARTESIAN_POINT('Ctrl Pts',(97.9178288079481,0.140500475882384,-7.58168206744287));
#37274=CARTESIAN_POINT('Ctrl Pts',(97.9206615212428,0.0985136951381394,
-7.58398424136599));
#37275=CARTESIAN_POINT('Ctrl Pts',(97.9228602202261,0.065924342623426,-7.58577114562968));
#37276=CARTESIAN_POINT('Ctrl Pts',(97.9239680194875,0.0332605710567664,
-7.58755804989338));
#37277=CARTESIAN_POINT('Ctrl Pts',(97.9239808370563,0.000573888477526073,
-7.58934495415708));
#37278=CARTESIAN_POINT('Origin',(96.460480949577,-8.32667268468867E-16,
1.18130019239114E-14));
#37279=CARTESIAN_POINT('',(97.9239807231656,0.000814067757715891,-8.16065504580903));
#37280=CARTESIAN_POINT('',(97.9239807535762,0.000757426072927294,-8.08934495412446));
#37281=CARTESIAN_POINT('',(97.923980949577,-1.01189432752408E-15,1.19922289829666E-14));
#37282=CARTESIAN_POINT('Ctrl Pts',(97.9239807231655,0.000814067757716574,
-8.16065504580903));
#37283=CARTESIAN_POINT('Ctrl Pts',(97.9239464028604,0.0625137952283417,
-8.15731430388859));
#37284=CARTESIAN_POINT('Ctrl Pts',(97.9200061480074,0.124074536863195,-8.15397356196815));
#37285=CARTESIAN_POINT('Ctrl Pts',(97.9122370551678,0.185030970056225,-8.1506328200477));
#37286=CARTESIAN_POINT('Ctrl Pts',(97.9042418234276,0.24776169286938,-8.14719483746861));
#37287=CARTESIAN_POINT('Ctrl Pts',(97.8921915595825,0.30985203107941,-8.14375685488951));
#37288=CARTESIAN_POINT('Ctrl Pts',(97.8762243240005,0.370813899113717,-8.14031887231041));
#37289=CARTESIAN_POINT('Ctrl Pts',(97.8602570884185,0.43177576714803,-8.13688088973131));
#37290=CARTESIAN_POINT('Ctrl Pts',(97.840373094531,0.491608884166954,-8.13344290715221));
#37291=CARTESIAN_POINT('Ctrl Pts',(97.8167620668367,0.549848871022543,-8.13000492457311));
#37292=CARTESIAN_POINT('Ctrl Pts',(97.7960894108393,0.600840942572633,-8.12699479591192));
#37293=CARTESIAN_POINT('Ctrl Pts',(97.7724935993597,0.650772688870189,-8.12398466725073));
#37294=CARTESIAN_POINT('Ctrl Pts',(97.746105053258,0.699287433059187,-8.12097453858954));
#37295=CARTESIAN_POINT('Ctrl Pts',(97.7197634070382,0.747715952877777,-8.11796975977514));
#37296=CARTESIAN_POINT('Ctrl Pts',(97.6906391265511,0.794732008217593,-8.11496498096075));
#37297=CARTESIAN_POINT('Ctrl Pts',(97.6589103975745,0.839999469150084,-8.11196020214635));
#37298=CARTESIAN_POINT('Ctrl Pts',(97.6272130589186,0.885222145429594,-8.10895839606278));
#37299=CARTESIAN_POINT('Ctrl Pts',(97.5929166776638,0.928699223901486,-8.10595658997921));
#37300=CARTESIAN_POINT('Ctrl Pts',(97.5562440458509,0.970121377377232,-8.10295478389564));
#37301=CARTESIAN_POINT('Ctrl Pts',(97.5195932107292,1.01151891124313,-8.09995476196109));
#37302=CARTESIAN_POINT('Ctrl Pts',(97.4805692737868,1.05086354630713,-8.09695474002655));
#37303=CARTESIAN_POINT('Ctrl Pts',(97.4394353835665,1.08787888396288,-8.093954718092));
#37304=CARTESIAN_POINT('Ctrl Pts',(97.3983096956925,1.12488684053655,-8.09095529437996));
#37305=CARTESIAN_POINT('Ctrl Pts',(97.355075282457,1.15956606906559,-8.08795587066792));
#37306=CARTESIAN_POINT('Ctrl Pts',(97.3100305450237,1.1916785367188,-8.08495644695589));
#37307=CARTESIAN_POINT('Ctrl Pts',(97.2649443954787,1.22382052713489,-8.08195426570818));
#37308=CARTESIAN_POINT('Ctrl Pts',(97.2180450275701,1.25339073494585,-8.07895208446047));
#37309=CARTESIAN_POINT('Ctrl Pts',(97.1696609705368,1.28019371497892,-8.07594990321276));
#37310=CARTESIAN_POINT('Ctrl Pts',(97.1212548901547,1.30700889513351,-8.07294635543879));
#37311=CARTESIAN_POINT('Ctrl Pts',(97.0713632500681,1.33105410693777,-8.06994280766482));
#37312=CARTESIAN_POINT('Ctrl Pts',(97.02033744414,1.35218081464558,-8.06693925989085));
#37313=CARTESIAN_POINT('Ctrl Pts',(96.9692153355905,1.37334739545873,-8.06393004342593));
#37314=CARTESIAN_POINT('Ctrl Pts',(96.9169552849752,1.39158429428975,-8.06092082696102));
#37315=CARTESIAN_POINT('Ctrl Pts',(96.8639257297596,1.40679229431478,-8.0579116104961));
#37316=CARTESIAN_POINT('Ctrl Pts',(96.8233559466894,1.41842703760911,-8.05560943657258));
#37317=CARTESIAN_POINT('Ctrl Pts',(96.7823361516432,1.42829002409365,-8.05330726264907));
#37318=CARTESIAN_POINT('Ctrl Pts',(96.7410344002811,1.43635720184709,-8.05100508872556));
#37319=CARTESIAN_POINT('Ctrl Pts',(96.6870317099268,1.44690516380721,-8.04799496006434));
#37320=CARTESIAN_POINT('Ctrl Pts',(96.6323198698276,1.45442554682468,-8.04498483140311));
#37321=CARTESIAN_POINT('Ctrl Pts',(96.5772688678957,1.45883269504587,-8.04197470274189));
#37322=CARTESIAN_POINT('Ctrl Pts',(96.5223157071059,1.46323201052287,-8.03896992392746));
#37323=CARTESIAN_POINT('Ctrl Pts',(96.4670251028906,1.46452902986565,-8.03596514511304));
#37324=CARTESIAN_POINT('Ctrl Pts',(96.4117759331206,1.46268932838521,-8.03296036629861));
#37325=CARTESIAN_POINT('Ctrl Pts',(96.3565814232508,1.4608514469846,-8.02995856021501));
#37326=CARTESIAN_POINT('Ctrl Pts',(96.3014287918509,1.45588300966986,-8.0269567541314));
#37327=CARTESIAN_POINT('Ctrl Pts',(96.2466988414626,1.44780159560975,-8.0239549480478));
#37328=CARTESIAN_POINT('Ctrl Pts',(96.1920014202866,1.43972498480695,-8.02095492611322));
#37329=CARTESIAN_POINT('Ctrl Pts',(96.1377267035879,1.42853914151573,-8.01795490417863));
#37330=CARTESIAN_POINT('Ctrl Pts',(96.0842499659686,1.41431343660911,-8.01495488224405));
#37331=CARTESIAN_POINT('Ctrl Pts',(96.030783891934,1.40009056839403,-8.01195545853197));
#37332=CARTESIAN_POINT('Ctrl Pts',(95.9781159910503,1.38282917807471,-8.0089560348199));
#37333=CARTESIAN_POINT('Ctrl Pts',(95.9266086674442,1.36264912445217,-8.00595661110783));
#37334=CARTESIAN_POINT('Ctrl Pts',(95.8750539903143,1.34245051819319,-8.00295442986008));
#37335=CARTESIAN_POINT('Ctrl Pts',(95.8246625149347,1.3193280808361,-7.99995224861234));
#37336=CARTESIAN_POINT('Ctrl Pts',(95.7757774389838,1.29345017398482,-7.9969500673646));
#37337=CARTESIAN_POINT('Ctrl Pts',(95.7268701116316,1.26756048808478,-7.9939465195906));
#37338=CARTESIAN_POINT('Ctrl Pts',(95.6794710033299,1.23891310611856,-7.9909429718166));
#37339=CARTESIAN_POINT('Ctrl Pts',(95.6338965169911,1.20772117055498,-7.98793942404259));
#37340=CARTESIAN_POINT('Ctrl Pts',(95.5882360164793,1.17647036546241,-7.98493020757765));
#37341=CARTESIAN_POINT('Ctrl Pts',(95.5444074363961,1.14266573653001,-7.9819209911127));
#37342=CARTESIAN_POINT('Ctrl Pts',(95.5026951862869,1.10656164836794,-7.97891177464775));
#37343=CARTESIAN_POINT('Ctrl Pts',(95.4707836054484,1.07894054125991,-7.9766096007245));
#37344=CARTESIAN_POINT('Ctrl Pts',(95.4401100338438,1.04997445604544,-7.97430742680124));
#37345=CARTESIAN_POINT('Ctrl Pts',(95.4107864405577,1.01979100198748,-7.97200525287799));
#37346=CARTESIAN_POINT('Ctrl Pts',(95.372445380523,0.980325660451858,-7.96899512421673));
#37347=CARTESIAN_POINT('Ctrl Pts',(95.3362525226972,0.938612129670457,-7.96598499555547));
#37348=CARTESIAN_POINT('Ctrl Pts',(95.3024817661057,0.894913482454971,-7.96297486689421));
#37349=CARTESIAN_POINT('Ctrl Pts',(95.2687710296642,0.851292500048519,-7.95997008807975));
#37350=CARTESIAN_POINT('Ctrl Pts',(95.237474171964,0.805693817262215,-7.95696530926528));
#37351=CARTESIAN_POINT('Ctrl Pts',(95.20882704199,0.758415944994775,-7.95396053045082));
#37352=CARTESIAN_POINT('Ctrl Pts',(95.1802082536051,0.711184846349246,-7.95095872436717));
#37353=CARTESIAN_POINT('Ctrl Pts',(95.1542342722823,0.662278298587115,-7.94795691828353));
#37354=CARTESIAN_POINT('Ctrl Pts',(95.1310984440087,0.612024839274533,-7.94495511219989));
#37355=CARTESIAN_POINT('Ctrl Pts',(95.1079763667118,0.561801248533632,-7.94195509026527));
#37356=CARTESIAN_POINT('Ctrl Pts',(95.0876893193695,0.510232811742635,-7.93895506833065));
#37357=CARTESIAN_POINT('Ctrl Pts',(95.0703842505783,0.457671735453273,-7.93595504639603));
#37358=CARTESIAN_POINT('Ctrl Pts',(95.0530826325224,0.40512114016024,-7.93295562268392));
#37359=CARTESIAN_POINT('Ctrl Pts',(95.0387619771807,0.351578799812521,-7.92995619897181));
#37360=CARTESIAN_POINT('Ctrl Pts',(95.0275199157738,0.297413727998022,-7.92695677525969));
#37361=CARTESIAN_POINT('Ctrl Pts',(95.0162675189198,0.243198859245237,-7.92395459401191));
#37362=CARTESIAN_POINT('Ctrl Pts',(95.0080994781695,0.188360633429305,-7.92095241276413));
#37363=CARTESIAN_POINT('Ctrl Pts',(95.0030623080127,0.133278479961912,-7.91795023151635));
#37364=CARTESIAN_POINT('Ctrl Pts',(94.998022845048,0.0781712543209931,-7.91494668374231));
#37365=CARTESIAN_POINT('Ctrl Pts',(94.9961171117249,0.0228204084206592,
-7.91194313596827));
#37366=CARTESIAN_POINT('Ctrl Pts',(94.997339476799,-0.0323926015764528,
-7.90893958819422));
#37367=CARTESIAN_POINT('Ctrl Pts',(94.9985641488813,-0.0877098168379549,
-7.90593037172924));
#37368=CARTESIAN_POINT('Ctrl Pts',(95.0029286712914,-0.142888148758757,
-7.90292115526425));
#37369=CARTESIAN_POINT('Ctrl Pts',(95.0103754070814,-0.197550412866063,
-7.89991193879926));
#37370=CARTESIAN_POINT('Ctrl Pts',(95.0160724651516,-0.239369285140981,
-7.89760976487632));
#37371=CARTESIAN_POINT('Ctrl Pts',(95.0235724219682,-0.280886182121544,
-7.89530759095337));
#37372=CARTESIAN_POINT('Ctrl Pts',(95.0328295808075,-0.32193760148588,-7.89300541703043));
#37373=CARTESIAN_POINT('Ctrl Pts',(95.0449334617809,-0.375612978824334,
-7.8899952883692));
#37374=CARTESIAN_POINT('Ctrl Pts',(95.060094031007,-0.428717580776824,-7.88698515970797));
#37375=CARTESIAN_POINT('Ctrl Pts',(95.078240615278,-0.480878267586556,-7.88397503104674));
#37376=CARTESIAN_POINT('Ctrl Pts',(95.0963549479557,-0.532946250158535,
-7.8809702522323));
#37377=CARTESIAN_POINT('Ctrl Pts',(95.1174445917954,-0.584073152043974,
-7.87796547341787));
#37378=CARTESIAN_POINT('Ctrl Pts',(95.1413884028453,-0.633898338187454,
-7.87496069460343));
#37379=CARTESIAN_POINT('Ctrl Pts',(95.165308525461,-0.683674230563958,-7.87195888851982));
#37380=CARTESIAN_POINT('Ctrl Pts',(95.1920769939993,-0.73215048466659,-7.8689570824362));
#37381=CARTESIAN_POINT('Ctrl Pts',(95.221524292895,-0.778985656391256,-7.86595527635259));
#37382=CARTESIAN_POINT('Ctrl Pts',(95.2509540895377,-0.825792991232581,
-7.862955254418));
#37383=CARTESIAN_POINT('Ctrl Pts',(95.2830592801791,-0.870960730790322,
-7.85995523248341));
#37384=CARTESIAN_POINT('Ctrl Pts',(95.3176251744894,-0.914173357383019,
-7.85695521054882));
#37385=CARTESIAN_POINT('Ctrl Pts',(95.3521841761514,-0.957377367116765,
-7.85395578683673));
#37386=CARTESIAN_POINT('Ctrl Pts',(95.3892025773124,-0.998626625955611,
-7.85095636312465));
#37387=CARTESIAN_POINT('Ctrl Pts',(95.428424664477,-1.03763773754891,-7.84795693941257));
#37388=CARTESIAN_POINT('Ctrl Pts',(95.4676828106698,-1.07668471420897,-7.84495475816482));
#37389=CARTESIAN_POINT('Ctrl Pts',(95.5091483152464,-1.11348905947541,-7.84195257691706));
#37390=CARTESIAN_POINT('Ctrl Pts',(95.5525288111977,-1.14780449747004,-7.83895039566931));
#37391=CARTESIAN_POINT('Ctrl Pts',(95.5959290529877,-1.18213555509029,-7.8359468478953));
#37392=CARTESIAN_POINT('Ctrl Pts',(95.641245590876,-1.21397514295113,-7.83294330012129));
#37393=CARTESIAN_POINT('Ctrl Pts',(95.6881558681701,-1.24311955122177,-7.82993975234728));
#37394=CARTESIAN_POINT('Ctrl Pts',(95.735154680718,-1.27231896465823,-7.82693053588232));
#37395=CARTESIAN_POINT('Ctrl Pts',(95.7837527766234,-1.29881278363055,-7.82392131941736));
#37396=CARTESIAN_POINT('Ctrl Pts',(95.8336027611374,-1.3224431885184,-7.8209121029524));
#37397=CARTESIAN_POINT('Ctrl Pts',(95.8717400423052,-1.3405214167085,-7.81860992902922));
#37398=CARTESIAN_POINT('Ctrl Pts',(95.9106095078347,-1.3569246705614,-7.81630775510604));
#37399=CARTESIAN_POINT('Ctrl Pts',(95.9500492516203,-1.37160188528635,-7.81400558118287));
#37400=CARTESIAN_POINT('Ctrl Pts',(96.0016173377522,-1.39079257468904,-7.81099545252163));
#37401=CARTESIAN_POINT('Ctrl Pts',(96.0543775465989,-1.40711133598547,-7.8079853238604));
#37402=CARTESIAN_POINT('Ctrl Pts',(96.1079787480087,-1.42041347779071,-7.80497519519916));
#37403=CARTESIAN_POINT('Ctrl Pts',(96.1614846849804,-1.43369197794184,-7.80197041638472));
#37404=CARTESIAN_POINT('Ctrl Pts',(96.215828139889,-1.44396437212751,-7.79896563757028));
#37405=CARTESIAN_POINT('Ctrl Pts',(96.2706408785899,-1.45113507208929,-7.79596085875583));
#37406=CARTESIAN_POINT('Ctrl Pts',(96.3253993891668,-1.45829867783146,-7.79295905267221));
#37407=CARTESIAN_POINT('Ctrl Pts',(96.380625742743,-1.4623665999551,-7.78995724658859));
#37408=CARTESIAN_POINT('Ctrl Pts',(96.4359413480525,-1.46329424859015,-7.78695544050498));
#37409=CARTESIAN_POINT('Ctrl Pts',(96.4912240760606,-1.46422134586934,-7.78395541857038));
#37410=CARTESIAN_POINT('Ctrl Pts',(96.5465954236708,-1.46201186024535,-7.78095539663578));
#37411=CARTESIAN_POINT('Ctrl Pts',(96.6016738303798,-1.45667320302483,-7.77795537470119));
#37412=CARTESIAN_POINT('Ctrl Pts',(96.6567412541216,-1.45133561036482,-7.7749559509891));
#37413=CARTESIAN_POINT('Ctrl Pts',(96.7115153276124,-1.44287013621937,-7.77195652727701));
#37414=CARTESIAN_POINT('Ctrl Pts',(96.7656189779315,-1.43133610086938,-7.76895710356492));
#37415=CARTESIAN_POINT('Ctrl Pts',(96.8197723687206,-1.41979146164447,-7.76595492231716));
#37416=CARTESIAN_POINT('Ctrl Pts',(96.8732535873175,-1.40517273537686,-7.7629527410694));
#37417=CARTESIAN_POINT('Ctrl Pts',(96.92569662286,-1.38759022313211,-7.75995055982164));
#37418=CARTESIAN_POINT('Ctrl Pts',(96.9781635293082,-1.36999970771809,-7.75694701204763));
#37419=CARTESIAN_POINT('Ctrl Pts',(97.0295908194455,-1.34944291345266,-7.75394346427361));
#37420=CARTESIAN_POINT('Ctrl Pts',(97.0796316370957,-1.3260786839947,-7.75093991649959));
#37421=CARTESIAN_POINT('Ctrl Pts',(97.1297668983678,-1.30267035848568,-7.74793070003463));
#37422=CARTESIAN_POINT('Ctrl Pts',(97.178509993609,-1.27644426392918,-7.74492148356967));
#37423=CARTESIAN_POINT('Ctrl Pts',(97.2255389295129,-1.24760512075593,-7.74191226710471));
#37424=CARTESIAN_POINT('Ctrl Pts',(97.2615179928775,-1.22554199430688,-7.73961009318157));
#37425=CARTESIAN_POINT('Ctrl Pts',(97.2964942828172,-1.20195044434721,-7.73730791925843));
#37426=CARTESIAN_POINT('Ctrl Pts',(97.330336566335,-1.17693816999641,-7.7350057453353));
#37427=CARTESIAN_POINT('Ctrl Pts',(97.3758768095831,-1.14328012627949,-7.73190779952429));
#37428=CARTESIAN_POINT('Ctrl Pts',(97.4195684264721,-1.10689512752576,-7.72880985371328));
#37429=CARTESIAN_POINT('Ctrl Pts',(97.4610650931287,-1.06801854931123,-7.72571190790227));
#37430=CARTESIAN_POINT('Ctrl Pts',(97.5009660260385,-1.03063695064124,-7.7227330920618));
#37431=CARTESIAN_POINT('Ctrl Pts',(97.5388373000252,-0.990952309552827,
-7.71975427622134));
#37432=CARTESIAN_POINT('Ctrl Pts',(97.5744015893822,-0.949217076445578,
-7.71677546038087));
#37433=CARTESIAN_POINT('Ctrl Pts',(97.6099317286148,-0.907521919027523,
-7.71379950490775));
#37434=CARTESIAN_POINT('Ctrl Pts',(97.6431589216179,-0.863780475734517,
-7.71082354943462));
#37435=CARTESIAN_POINT('Ctrl Pts',(97.6738429280665,-0.818281711365913,
-7.7078475939615));
#37436=CARTESIAN_POINT('Ctrl Pts',(97.704510123906,-0.77280787405331,-7.70487326890207));
#37437=CARTESIAN_POINT('Ctrl Pts',(97.7326365934287,-0.725579068743478,
-7.70189894384265));
#37438=CARTESIAN_POINT('Ctrl Pts',(97.7580241324221,-0.676915015827166,
-7.69892461878322));
#37439=CARTESIAN_POINT('Ctrl Pts',(97.7834082307919,-0.628257558063158,
-7.69595069681655));
#37440=CARTESIAN_POINT('Ctrl Pts',(97.8060538882951,-0.578165716678501,
-7.69297677484987));
#37441=CARTESIAN_POINT('Ctrl Pts',(97.8258089713965,-0.526983531843833,
-7.69000285288319));
#37442=CARTESIAN_POINT('Ctrl Pts',(97.8455819994866,-0.475754854482134,
-7.68702622948538));
#37443=CARTESIAN_POINT('Ctrl Pts',(97.8624590207538,-0.42343436066911,-7.68404960608758));
#37444=CARTESIAN_POINT('Ctrl Pts',(97.8763368191506,-0.37038413383133,-7.68107298268977));
#37445=CARTESIAN_POINT('Ctrl Pts',(97.8902221992464,-0.31730492466961,-7.67809473310733));
#37446=CARTESIAN_POINT('Ctrl Pts',(97.9011049906649,-0.263495717065944,
-7.67511648352489));
#37447=CARTESIAN_POINT('Ctrl Pts',(97.9089331718106,-0.209328473711563,
-7.67213823394245));
#37448=CARTESIAN_POINT('Ctrl Pts',(97.9167743489373,-0.155071304427995,
-7.66915504000906));
#37449=CARTESIAN_POINT('Ctrl Pts',(97.9215507579237,-0.100455449451422,
-7.66617184607568));
#37450=CARTESIAN_POINT('Ctrl Pts',(97.9232623684937,-0.0458559753144874,
-7.66318865214229));
#37451=CARTESIAN_POINT('Ctrl Pts',(97.9237469215567,-0.0303989882543154,
-7.66234411671855));
#37452=CARTESIAN_POINT('Ctrl Pts',(97.9239861685101,-0.0149432940640844,
-7.66149958129481));
#37453=CARTESIAN_POINT('Ctrl Pts',(97.9239808632502,0.000502671547976529,
-7.66065504587106));
#37454=CARTESIAN_POINT('Ctrl Pts',(97.9239808370565,0.00057388792750276,
-7.58934495418714));
#37455=CARTESIAN_POINT('Ctrl Pts',(97.9240028461078,-0.0555524784163405,
-7.59241325097991));
#37456=CARTESIAN_POINT('Ctrl Pts',(97.9207913233707,-0.111807974811069,
-7.59548154777268));
#37457=CARTESIAN_POINT('Ctrl Pts',(97.9143311632191,-0.167785000202359,
-7.59854984456545));
#37458=CARTESIAN_POINT('Ctrl Pts',(97.9080666489641,-0.222066761843438,
-7.60152521801527));
#37459=CARTESIAN_POINT('Ctrl Pts',(97.8987475302933,-0.276086097553949,
-7.60450059146509));
#37460=CARTESIAN_POINT('Ctrl Pts',(97.8864127316492,-0.329470488627234,
-7.6074759649149));
#37461=CARTESIAN_POINT('Ctrl Pts',(97.874088928565,-0.382807291468012,-7.61044868603956));
#37462=CARTESIAN_POINT('Ctrl Pts',(97.8587548885398,-0.435509746893538,
-7.61342140716422));
#37463=CARTESIAN_POINT('Ctrl Pts',(97.8405009258672,-0.487213623619121,
-7.61639412828888));
#37464=CARTESIAN_POINT('Ctrl Pts',(97.8222556758174,-0.538892822066113,
-7.6193654305327));
#37465=CARTESIAN_POINT('Ctrl Pts',(97.8010934439899,-0.589573878319355,
-7.62233673277652));
#37466=CARTESIAN_POINT('Ctrl Pts',(97.7771542131249,-0.638908261848428,
-7.62530803502034));
#37467=CARTESIAN_POINT('Ctrl Pts',(97.7532164953648,-0.688239527144512,
-7.62827914945979));
#37468=CARTESIAN_POINT('Ctrl Pts',(97.7265023650285,-0.736223804873542,
-7.63125026389924));
#37469=CARTESIAN_POINT('Ctrl Pts',(97.6971986597833,-0.782535338027751,
-7.63422137833869));
#37470=CARTESIAN_POINT('Ctrl Pts',(97.6678656785182,-0.828893138961163,
-7.63719546108555));
#37471=CARTESIAN_POINT('Ctrl Pts',(97.6359382520737,-0.873574406303675,
-7.64016954383241));
#37472=CARTESIAN_POINT('Ctrl Pts',(97.6016466922879,-0.916282160506793,
-7.64314362657927));
#37473=CARTESIAN_POINT('Ctrl Pts',(97.5673341391361,-0.959016060488219,
-7.64611953006593));
#37474=CARTESIAN_POINT('Ctrl Pts',(97.5306549364374,-0.99977364518832,-7.64909543355259));
#37475=CARTESIAN_POINT('Ctrl Pts',(97.4918776007987,-1.03829340643611,-7.65207133703926));
#37476=CARTESIAN_POINT('Ctrl Pts',(97.4530340547581,-1.07687893829012,-7.65505232173541));
#37477=CARTESIAN_POINT('Ctrl Pts',(97.4120856380219,-1.11321867435527,-7.65803330643157));
#37478=CARTESIAN_POINT('Ctrl Pts',(97.3693340381951,-1.14709124018506,-7.66101429112772));
#37479=CARTESIAN_POINT('Ctrl Pts',(97.3599175181445,-1.15455205326792,-7.66167088648966));
#37480=CARTESIAN_POINT('Ctrl Pts',(97.3504136240353,-1.16189334111058,-7.6623274818516));
#37481=CARTESIAN_POINT('Ctrl Pts',(97.3408257528014,-1.16911303022237,-7.66298407721354));
#37482=CARTESIAN_POINT('Ctrl Pts',(97.296870635732,-1.20221133456666,-7.66599420587478));
#37483=CARTESIAN_POINT('Ctrl Pts',(97.2509539746627,-1.23289686607644,-7.66900433453601));
#37484=CARTESIAN_POINT('Ctrl Pts',(97.2033710646308,-1.26093081767217,-7.67201446319725));
#37485=CARTESIAN_POINT('Ctrl Pts',(97.1558727228374,-1.28891494503684,-7.67501924201169));
#37486=CARTESIAN_POINT('Ctrl Pts',(97.1067144603246,-1.31425657877322,-7.67802402082613));
#37487=CARTESIAN_POINT('Ctrl Pts',(97.0562219674992,-1.33675909930136,-7.68102879964058));
#37488=CARTESIAN_POINT('Ctrl Pts',(97.0057794286303,-1.35923935731351,-7.6840306057242));
#37489=CARTESIAN_POINT('Ctrl Pts',(96.954005754314,-1.37888585235764,-7.68703241180782));
#37490=CARTESIAN_POINT('Ctrl Pts',(96.9012511039757,-1.39554789276162,-7.69003421789144));
#37491=CARTESIAN_POINT('Ctrl Pts',(96.8485278088132,-1.41220002993994,-7.69303423982604));
#37492=CARTESIAN_POINT('Ctrl Pts',(96.7948251958644,-1.42587106959957,-7.69603426176064));
#37493=CARTESIAN_POINT('Ctrl Pts',(96.7405110983378,-1.43645931574306,-7.69903428369524));
#37494=CARTESIAN_POINT('Ctrl Pts',(96.6862078313705,-1.44704545052625,-7.70203370740733));
#37495=CARTESIAN_POINT('Ctrl Pts',(96.6312938400482,-1.45454991162153,-7.70503313111942));
#37496=CARTESIAN_POINT('Ctrl Pts',(96.5761474578232,-1.45892203659761,-7.70803255483151));
#37497=CARTESIAN_POINT('Ctrl Pts',(96.5209503764872,-1.46329818110936,-7.71103473607927));
#37498=CARTESIAN_POINT('Ctrl Pts',(96.4655210049996,-1.46453619434792,-7.71403691732703));
#37499=CARTESIAN_POINT('Ctrl Pts',(96.4102416108544,-1.46263743246395,-7.71703909857478));
#37500=CARTESIAN_POINT('Ctrl Pts',(96.3549370547562,-1.46073780630571,-7.7200426463488));
#37501=CARTESIAN_POINT('Ctrl Pts',(96.2997831389271,-1.45569860695874,-7.72304619412282));
#37502=CARTESIAN_POINT('Ctrl Pts',(96.2451576130081,-1.44757317974907,-7.72604974189684));
#37503=CARTESIAN_POINT('Ctrl Pts',(96.190428990602,-1.439432417163,-7.7290589583618));
#37504=CARTESIAN_POINT('Ctrl Pts',(96.1362312686457,-1.42819389839307,-7.73206817482677));
#37505=CARTESIAN_POINT('Ctrl Pts',(96.0829314475773,-1.41396203044488,-7.73507739129173));
#37506=CARTESIAN_POINT('Ctrl Pts',(96.0421549000608,-1.4030740681965,-7.73737956521486));
#37507=CARTESIAN_POINT('Ctrl Pts',(96.0019036750428,-1.39043520068455,-7.73968173913799));
#37508=CARTESIAN_POINT('Ctrl Pts',(95.9623342670875,-1.37611123559279,-7.74198391306112));
#37509=CARTESIAN_POINT('Ctrl Pts',(95.9105966430106,-1.35738242564838,-7.74499404172235));
#37510=CARTESIAN_POINT('Ctrl Pts',(95.8598080011761,-1.33569244020792,-7.74800417038358));
#37511=CARTESIAN_POINT('Ctrl Pts',(95.8103296969894,-1.31115811356174,-7.75101429904482));
#37512=CARTESIAN_POINT('Ctrl Pts',(95.7609393296906,-1.28666739132701,-7.75401907785926));
#37513=CARTESIAN_POINT('Ctrl Pts',(95.712855147758,-1.25934259267138,-7.7570238566737));
#37514=CARTESIAN_POINT('Ctrl Pts',(95.666419781341,-1.22934905990919,-7.76002863548815));
#37515=CARTESIAN_POINT('Ctrl Pts',(95.6200303550259,-1.19938520077853,-7.76303044157177));
#37516=CARTESIAN_POINT('Ctrl Pts',(95.5752869542786,-1.16675812292454,-7.76603224765539));
#37517=CARTESIAN_POINT('Ctrl Pts',(95.5325071131653,-1.13167875695152,-7.76903405373901));
#37518=CARTESIAN_POINT('Ctrl Pts',(95.4897526986151,-1.0966202406986,-7.7720340756736));
#37519=CARTESIAN_POINT('Ctrl Pts',(95.4489599380729,-1.05911265946183,-7.7750340976082));
#37520=CARTESIAN_POINT('Ctrl Pts',(95.4104149872946,-1.01940851715886,-7.77803411954279));
#37521=CARTESIAN_POINT('Ctrl Pts',(95.3718777226125,-0.979712292101841,
-7.78103354325488));
#37522=CARTESIAN_POINT('Ctrl Pts',(95.3355877451907,-0.937820754555388,
-7.78403296696697));
#37523=CARTESIAN_POINT('Ctrl Pts',(95.3017942060922,-0.894023087214553,
-7.78703239067905));
#37524=CARTESIAN_POINT('Ctrl Pts',(95.2679695987292,-0.850185154262212,
-7.79003457192681));
#37525=CARTESIAN_POINT('Ctrl Pts',(95.2366463383367,-0.804438009447662,
-7.79303675317457));
#37526=CARTESIAN_POINT('Ctrl Pts',(95.2080321585604,-0.757102553080574,
-7.79603893442233));
#37527=CARTESIAN_POINT('Ctrl Pts',(95.1794049542447,-0.709745550664493,
-7.79904248219635));
#37528=CARTESIAN_POINT('Ctrl Pts',(95.1534895362214,-0.660799263062481,
-7.80204602997037));
#37529=CARTESIAN_POINT('Ctrl Pts',(95.1304476272651,-0.610609213441792,
-7.80504957774439));
#37530=CARTESIAN_POINT('Ctrl Pts',(95.1073622305835,-0.560324438549092,
-7.80805879420935));
#37531=CARTESIAN_POINT('Ctrl Pts',(95.0871613699973,-0.508791705252998,
-7.81106801067432));
#37532=CARTESIAN_POINT('Ctrl Pts',(95.069958129428,-0.45637543387533,-7.81407722713928));
#37533=CARTESIAN_POINT('Ctrl Pts',(95.056796945348,-0.41627483808297,-7.81637940106241));
#37534=CARTESIAN_POINT('Ctrl Pts',(95.0453892256993,-0.375657526258463,
-7.81868157498554));
#37535=CARTESIAN_POINT('Ctrl Pts',(95.035765362791,-0.334690523871059,-7.82098374890867));
#37536=CARTESIAN_POINT('Ctrl Pts',(95.0231820104731,-0.281125523063627,
-7.82399387756991));
#37537=CARTESIAN_POINT('Ctrl Pts',(95.0135972424989,-0.226737345757492,
-7.82700400623114));
#37538=CARTESIAN_POINT('Ctrl Pts',(95.007110650181,-0.171892474627354,-7.83001413489238));
#37539=CARTESIAN_POINT('Ctrl Pts',(95.0006355863653,-0.117145078286787,
-7.83301891370682));
#37540=CARTESIAN_POINT('Ctrl Pts',(94.9972478323819,-0.0619431191127279,
-7.83602369252127));
#37541=CARTESIAN_POINT('Ctrl Pts',(94.9969961213614,-0.00666390146810231,
-7.83902847133572));
#37542=CARTESIAN_POINT('Ctrl Pts',(94.9967446593672,0.0485606265489857,
-7.84203027741934));
#37543=CARTESIAN_POINT('Ctrl Pts',(94.9996230966375,0.103861736109363,-7.84503208350295));
#37544=CARTESIAN_POINT('Ctrl Pts',(95.0056282724815,0.158858232232584,-7.84803388958658));
#37545=CARTESIAN_POINT('Ctrl Pts',(95.0116298790981,0.213822040719754,-7.85103391152118));
#37546=CARTESIAN_POINT('Ctrl Pts',(95.0207544835995,0.268481070674426,-7.85403393345578));
#37547=CARTESIAN_POINT('Ctrl Pts',(95.0329469615407,0.32245769180041,-7.85703395539038));
#37548=CARTESIAN_POINT('Ctrl Pts',(95.0451370082282,0.376423549661888,-7.86003337910247));
#37549=CARTESIAN_POINT('Ctrl Pts',(95.0603935971449,0.429706754088005,-7.86303280281456));
#37550=CARTESIAN_POINT('Ctrl Pts',(95.0786106651637,0.481940626068776,-7.86603222652665));
#37551=CARTESIAN_POINT('Ctrl Pts',(95.0968444811381,0.534222519529316,-7.86903440777442));
#37552=CARTESIAN_POINT('Ctrl Pts',(95.118044039595,0.585452653450035,-7.87203658902218));
#37553=CARTESIAN_POINT('Ctrl Pts',(95.1420540827371,0.635281706642631,-7.87503877026994));
#37554=CARTESIAN_POINT('Ctrl Pts',(95.1660750547179,0.685133440914093,-7.87804231804396));
#37555=CARTESIAN_POINT('Ctrl Pts',(95.192908805199,0.733582360370158,-7.88104586581798));
#37556=CARTESIAN_POINT('Ctrl Pts',(95.222354313918,0.780304225332474,-7.884049413592));
#37557=CARTESIAN_POINT('Ctrl Pts',(95.2518553960792,0.827114269951953,-7.88705863005697));
#37558=CARTESIAN_POINT('Ctrl Pts',(95.2839777761885,0.872190317532797,-7.89006784652194));
#37559=CARTESIAN_POINT('Ctrl Pts',(95.3184780310294,0.915238539414054,-7.89307706298691));
#37560=CARTESIAN_POINT('Ctrl Pts',(95.3448721399146,0.948172193408378,-7.89537923691002));
#37561=CARTESIAN_POINT('Ctrl Pts',(95.3726570984648,0.979919605362234,-7.89768141083313));
#37562=CARTESIAN_POINT('Ctrl Pts',(95.4017096245929,1.01036405883792,-7.89998358475624));
#37563=CARTESIAN_POINT('Ctrl Pts',(95.4396962600516,1.0501706612249,-7.90299371341748));
#37564=CARTESIAN_POINT('Ctrl Pts',(95.4800107426962,1.08791564893066,-7.90600384207871));
#37565=CARTESIAN_POINT('Ctrl Pts',(95.5224005497256,1.12331536685595,-7.90901397073995));
#37566=CARTESIAN_POINT('Ctrl Pts',(95.5647150181239,1.15865216950793,-7.9120187495544));
#37567=CARTESIAN_POINT('Ctrl Pts',(95.6090970891016,1.19165163843458,-7.91502352836885));
#37568=CARTESIAN_POINT('Ctrl Pts',(95.6552573876917,1.22206680070472,-7.91802830718329));
#37569=CARTESIAN_POINT('Ctrl Pts',(95.7013720183138,1.2524518722108,-7.92103011326692));
#37570=CARTESIAN_POINT('Ctrl Pts',(95.7492609527108,1.28025741270279,-7.92403191935054));
#37571=CARTESIAN_POINT('Ctrl Pts',(95.7986032028385,1.30527778590322,-7.92703372543416));
#37572=CARTESIAN_POINT('Ctrl Pts',(95.8479161259795,1.33028328803166,-7.93003374736876));
#37573=CARTESIAN_POINT('Ctrl Pts',(95.8986801826815,1.35250666558881,-7.93303376930337));
#37574=CARTESIAN_POINT('Ctrl Pts',(95.9505489776281,1.37178775106951,-7.93603379123797));
#37575=CARTESIAN_POINT('Ctrl Pts',(96.0024074296236,1.39106499178524,-7.93903321495007));
#37576=CARTESIAN_POINT('Ctrl Pts',(96.0553696876308,1.40740092169702,-7.94203263866216));
#37577=CARTESIAN_POINT('Ctrl Pts',(96.109070695634,1.42068401955668,-7.94503206237426));
#37578=CARTESIAN_POINT('Ctrl Pts',(96.1628210739361,1.43397932930088,-7.94803424362202));
#37579=CARTESIAN_POINT('Ctrl Pts',(96.2173110453676,1.44421607261537,-7.95103642486978));
#37580=CARTESIAN_POINT('Ctrl Pts',(96.2721632117813,1.45133341435782,-7.95403860611754));
#37581=CARTESIAN_POINT('Ctrl Pts',(96.3270403456836,1.45845399575624,-7.95704215389157));
#37582=CARTESIAN_POINT('Ctrl Pts',(96.3822794755548,1.46245230695228,-7.96004570166559));
#37583=CARTESIAN_POINT('Ctrl Pts',(96.4374992052558,1.46331954453836,-7.96304924943961));
#37584=CARTESIAN_POINT('Ctrl Pts',(96.4928231529035,1.46418841888944,-7.96605846590458));
#37585=CARTESIAN_POINT('Ctrl Pts',(96.5481270982729,1.46191443648731,-7.96906768236955));
#37586=CARTESIAN_POINT('Ctrl Pts',(96.603031946463,1.45654092400001,-7.97207689883452));
#37587=CARTESIAN_POINT('Ctrl Pts',(96.6450364055061,1.45242996672336,-7.97437907275761));
#37588=CARTESIAN_POINT('Ctrl Pts',(96.6868073097122,1.44650597742622,-7.97668124668071));
#37589=CARTESIAN_POINT('Ctrl Pts',(96.728179545075,1.43880843477108,-7.97898342060381));
#37590=CARTESIAN_POINT('Ctrl Pts',(96.7822743943803,1.42874377652141,-7.98199354926504));
#37591=CARTESIAN_POINT('Ctrl Pts',(96.8359145124702,1.41560302543563,-7.98500367792627));
#37592=CARTESIAN_POINT('Ctrl Pts',(96.8887243530978,1.39944268812301,-7.9880138065875));
#37593=CARTESIAN_POINT('Ctrl Pts',(96.9414403357584,1.38331107228327,-7.99101858540194));
#37594=CARTESIAN_POINT('Ctrl Pts',(96.9933284684523,1.36417067366595,-7.99402336421638));
#37595=CARTESIAN_POINT('Ctrl Pts',(97.0440237913569,1.34212890655383,-7.99702814303082));
#37596=CARTESIAN_POINT('Ctrl Pts',(97.0946689596385,1.32010894611851,-8.00002994911443));
#37597=CARTESIAN_POINT('Ctrl Pts',(97.1441231738903,1.2951935129002,-8.00303175519805));
#37598=CARTESIAN_POINT('Ctrl Pts',(97.1920388215885,1.26753908416982,-8.00603356128167));
#37599=CARTESIAN_POINT('Ctrl Pts',(97.2399259902132,1.23990109208476,-8.00903358321626));
#37600=CARTESIAN_POINT('Ctrl Pts',(97.2862759483156,1.2095275946438,-8.01203360515086));
#37601=CARTESIAN_POINT('Ctrl Pts',(97.3307652822583,1.17662119235098,-8.01503362708546));
#37602=CARTESIAN_POINT('Ctrl Pts',(97.3752457447589,1.14372135179367,-8.01803305079755));
#37603=CARTESIAN_POINT('Ctrl Pts',(97.4178658955736,1.10828992331808,-8.02103247450964));
#37604=CARTESIAN_POINT('Ctrl Pts',(97.4583328674818,1.07057171638976,-8.02403189822173));
#37605=CARTESIAN_POINT('Ctrl Pts',(97.4988370429094,1.03281883303333,-8.02703407946948));
#37606=CARTESIAN_POINT('Ctrl Pts',(97.5371836974197,0.992775331835817,-8.03003626071724));
#37607=CARTESIAN_POINT('Ctrl Pts',(97.5731156710776,0.950724053819656,-8.03303844196499));
#37608=CARTESIAN_POINT('Ctrl Pts',(97.6090640001723,0.908653634995189,-8.036041989739));
#37609=CARTESIAN_POINT('Ctrl Pts',(97.6425951371194,0.864574038622622,-8.03904553751302));
#37610=CARTESIAN_POINT('Ctrl Pts',(97.673493315475,0.818799884085621,-8.04204908528704));
#37611=CARTESIAN_POINT('Ctrl Pts',(97.7044498089422,0.77293933853546,-8.045058301752));
#37612=CARTESIAN_POINT('Ctrl Pts',(97.7327631461288,0.725378300839316,-8.04806751821696));
#37613=CARTESIAN_POINT('Ctrl Pts',(97.7582624783195,0.676457946700814,-8.05107673468192));
#37614=CARTESIAN_POINT('Ctrl Pts',(97.7777705124909,0.63903187086994,-8.05337890860507));
#37615=CARTESIAN_POINT('Ctrl Pts',(97.7956324701048,0.600810769922016,-8.05568108252822));
#37616=CARTESIAN_POINT('Ctrl Pts',(97.8117911979588,0.561954502267177,-8.05798325645138));
#37617=CARTESIAN_POINT('Ctrl Pts',(97.8352823864444,0.505466150240102,-8.06133010417628));
#37618=CARTESIAN_POINT('Ctrl Pts',(97.8552563046488,0.447434047055465,-8.06467695190118));
#37619=CARTESIAN_POINT('Ctrl Pts',(97.8715321197142,0.388287065525512,-8.06802379962608));
#37620=CARTESIAN_POINT('Ctrl Pts',(97.8877496688976,0.329351824607984,-8.07135866595195));
#37621=CARTESIAN_POINT('Ctrl Pts',(97.9002953787761,0.26930995292303,-8.07469353227782));
#37622=CARTESIAN_POINT('Ctrl Pts',(97.9090371646527,0.208607626336123,-8.0780283986037));
#37623=CARTESIAN_POINT('Ctrl Pts',(97.9177299795459,0.148245350703205,-8.08134458319957));
#37624=CARTESIAN_POINT('Ctrl Pts',(97.9226612352516,0.0872302985620028,
-8.08466076779545));
#37625=CARTESIAN_POINT('Ctrl Pts',(97.923749648434,0.0260185500224431,-8.08797695239133));
#37626=CARTESIAN_POINT('Ctrl Pts',(97.9238993135162,0.0176014695223185,
-8.08843295296904));
#37627=CARTESIAN_POINT('Ctrl Pts',(97.9239763941621,0.00918069264905495,
-8.08888895354675));
#37628=CARTESIAN_POINT('Ctrl Pts',(97.9239807535762,0.000757426072930723,
-8.08934495412446));
#37629=CARTESIAN_POINT('Origin',(96.460480949577,-8.32667268468867E-16,
1.18130019239114E-14));
#37630=CARTESIAN_POINT('',(97.9239804054011,-0.00126206278290129,-8.66065504588342));
#37631=CARTESIAN_POINT('',(97.9239803911303,-0.00127850425146132,-8.58934495419103));
#37632=CARTESIAN_POINT('',(97.923980949577,-1.01189432752408E-15,1.19922289829666E-14));
#37633=CARTESIAN_POINT('Ctrl Pts',(97.9239804054018,-0.0012620620365945,
-8.6606550458429));
#37634=CARTESIAN_POINT('Ctrl Pts',(97.9240276872323,0.053566410110067,-8.65767794005104));
#37635=CARTESIAN_POINT('Ctrl Pts',(97.9209895412013,0.1084571276113,-8.65470083425919));
#37636=CARTESIAN_POINT('Ctrl Pts',(97.914871620017,0.163033823904847,-8.65172372846733));
#37637=CARTESIAN_POINT('Ctrl Pts',(97.9087566825499,0.217583903081169,-8.64874807461337));
#37638=CARTESIAN_POINT('Ctrl Pts',(97.8995650059973,0.271819731168011,-8.64577242075942));
#37639=CARTESIAN_POINT('Ctrl Pts',(97.8873541773523,0.325369085590568,-8.64279676690547));
#37640=CARTESIAN_POINT('Ctrl Pts',(97.8751442845461,0.378914335987086,-8.63982134110582));
#37641=CARTESIAN_POINT('Ctrl Pts',(97.8599158208427,0.431772693885009,-8.63684591530617));
#37642=CARTESIAN_POINT('Ctrl Pts',(97.8417771765689,0.483583481208858,-8.63387048950652));
#37643=CARTESIAN_POINT('Ctrl Pts',(97.8236202153823,0.535446588521609,-8.63089205903829));
#37644=CARTESIAN_POINT('Ctrl Pts',(97.8025473891416,0.586259506865642,-8.62791362857006));
#37645=CARTESIAN_POINT('Ctrl Pts',(97.7787159875234,0.635679663612517,-8.62493519810183));
#37646=CARTESIAN_POINT('Ctrl Pts',(97.7548704339337,0.685129167884049,-8.62195499893096));
#37647=CARTESIAN_POINT('Ctrl Pts',(97.7282633079905,0.733183795884246,-8.61897479976009));
#37648=CARTESIAN_POINT('Ctrl Pts',(97.6990971959579,0.779526807878603,-8.61599460058922));
#37649=CARTESIAN_POINT('Ctrl Pts',(97.6698794337128,0.825951888624783,-8.61300912378931));
#37650=CARTESIAN_POINT('Ctrl Pts',(97.6380939598203,0.870658871980485,-8.6100236469894));
#37651=CARTESIAN_POINT('Ctrl Pts',(97.6039849017055,0.913362448027296,-8.60703817018948));
#37652=CARTESIAN_POINT('Ctrl Pts',(97.592429545286,0.927829427442212,-8.60602676001248));
#37653=CARTESIAN_POINT('Ctrl Pts',(97.5806078299067,0.94206678369978,-8.60501534983548));
#37654=CARTESIAN_POINT('Ctrl Pts',(97.568530182405,0.956064405586448,-8.60400393965848));
#37655=CARTESIAN_POINT('Ctrl Pts',(97.5325850498447,0.997723708374557,-8.60099381099893));
#37656=CARTESIAN_POINT('Ctrl Pts',(97.4942117303392,1.03744058079032,-8.59798368233938));
#37657=CARTESIAN_POINT('Ctrl Pts',(97.4536482220841,1.07491907547536,-8.59497355367983));
#37658=CARTESIAN_POINT('Ctrl Pts',(97.4131568066128,1.11233096031496,-8.59196877486707));
#37659=CARTESIAN_POINT('Ctrl Pts',(97.3704833120042,1.14751200675001,-8.58896399605431));
#37660=CARTESIAN_POINT('Ctrl Pts',(97.3259043796911,1.18020105770567,-8.58595921724156));
#37661=CARTESIAN_POINT('Ctrl Pts',(97.2813695508459,1.2128577682611,-8.58295741115963));
#37662=CARTESIAN_POINT('Ctrl Pts',(97.2349334424098,1.24302705644912,-8.57995560507771));
#37663=CARTESIAN_POINT('Ctrl Pts',(97.1869063396721,1.27048746653605,-8.57695379899578));
#37664=CARTESIAN_POINT('Ctrl Pts',(97.138907782252,1.2979315552943,-8.57395377706286));
#37665=CARTESIAN_POINT('Ctrl Pts',(97.089320562364,1.32266969555262,-8.57095375512995));
#37666=CARTESIAN_POINT('Ctrl Pts',(97.0384826181072,1.34452457068523,-8.56795373319704));
#37667=CARTESIAN_POINT('Ctrl Pts',(96.9876548112437,1.36637508782369,-8.56495430948662));
#37668=CARTESIAN_POINT('Ctrl Pts',(96.935577260224,1.38534327318383,-8.56195488577621));
#37669=CARTESIAN_POINT('Ctrl Pts',(96.8826089770052,1.40129946066485,-8.5589554620658));
#37670=CARTESIAN_POINT('Ctrl Pts',(96.8295919971214,1.41727031754929,-8.5559532808197));
#37671=CARTESIAN_POINT('Ctrl Pts',(96.7756831557414,1.43022349160527,-8.5529510995736));
#37672=CARTESIAN_POINT('Ctrl Pts',(96.721256330215,1.44007932102821,-8.5499489183275));
#37673=CARTESIAN_POINT('Ctrl Pts',(96.6668047308057,1.44993963660596,-8.54694537055513));
#37674=CARTESIAN_POINT('Ctrl Pts',(96.6118352023302,1.45669973255281,-8.54394182278276));
#37675=CARTESIAN_POINT('Ctrl Pts',(96.5567282212643,1.46033171323941,-8.54093827501039));
#37676=CARTESIAN_POINT('Ctrl Pts',(96.5015172350449,1.46397054867837,-8.53792905854703));
#37677=CARTESIAN_POINT('Ctrl Pts',(96.4461688073963,1.46446947034548,-8.53491984208368));
#37678=CARTESIAN_POINT('Ctrl Pts',(96.3910637275223,1.46185276251824,-8.53191062562032));
#37679=CARTESIAN_POINT('Ctrl Pts',(96.3489060827673,1.45985087377657,-8.52960845168386));
#37680=CARTESIAN_POINT('Ctrl Pts',(96.3068908890163,1.45602653043792,-8.52730627774739));
#37681=CARTESIAN_POINT('Ctrl Pts',(96.2651850304279,1.45041089142481,-8.52500410381093));
#37682=CARTESIAN_POINT('Ctrl Pts',(96.2106539638432,1.44306835502095,-8.52199397515112));
#37683=CARTESIAN_POINT('Ctrl Pts',(96.1564229831566,1.43263081037034,-8.51898384649131));
#37684=CARTESIAN_POINT('Ctrl Pts',(96.1028699935255,1.4191358828921,-8.5159737178315));
#37685=CARTESIAN_POINT('Ctrl Pts',(96.0494121826475,1.40566493970267,-8.51296893901853));
#37686=CARTESIAN_POINT('Ctrl Pts',(95.9966304794966,1.38914752516248,-8.50996416020556));
#37687=CARTESIAN_POINT('Ctrl Pts',(95.9448947659446,1.36967263871603,-8.50695938139259));
#37688=CARTESIAN_POINT('Ctrl Pts',(95.8932102363104,1.35021701944346,-8.50395757531048));
#37689=CARTESIAN_POINT('Ctrl Pts',(95.8425701381476,1.32780990952714,-8.50095576922837));
#37690=CARTESIAN_POINT('Ctrl Pts',(95.7933294852573,1.30259017870396,-8.49795396314626));
#37691=CARTESIAN_POINT('Ctrl Pts',(95.7441180989689,1.27738543744288,-8.49495394121319));
#37692=CARTESIAN_POINT('Ctrl Pts',(95.696304978438,1.24937162897091,-8.49195391928012));
#37693=CARTESIAN_POINT('Ctrl Pts',(95.6502232791616,1.21873490043279,-8.48895389734706));
#37694=CARTESIAN_POINT('Ctrl Pts',(95.6041507688549,1.18810428104376,-8.48595447363652));
#37695=CARTESIAN_POINT('Ctrl Pts',(95.5598094336834,1.15485207252031,-8.48295504992598));
#37696=CARTESIAN_POINT('Ctrl Pts',(95.5175040352204,1.11920810798997,-8.47995562621545));
#37697=CARTESIAN_POINT('Ctrl Pts',(95.4751597430713,1.08353137399718,-8.47695344496927));
#37698=CARTESIAN_POINT('Ctrl Pts',(95.4348555318852,1.04545883194678,-8.47395126372309));
#37699=CARTESIAN_POINT('Ctrl Pts',(95.3968624056838,1.00526008728411,-8.47094908247691));
#37700=CARTESIAN_POINT('Ctrl Pts',(95.3588519858549,0.965043045045409,-8.46794553470448));
#37701=CARTESIAN_POINT('Ctrl Pts',(95.3231550889943,0.92269827543808,-8.46494198693206));
#37702=CARTESIAN_POINT('Ctrl Pts',(95.2900029692953,0.878529195687755,-8.46193843915963));
#37703=CARTESIAN_POINT('Ctrl Pts',(95.2567882805497,0.83427675423281,-8.45892922269626));
#37704=CARTESIAN_POINT('Ctrl Pts',(95.2261282566351,0.788193565322302,-8.4559200062329));
#37705=CARTESIAN_POINT('Ctrl Pts',(95.1982106205418,0.740611818996549,-8.45291078976953));
#37706=CARTESIAN_POINT('Ctrl Pts',(95.1768524846503,0.704209832790175,-8.45060861583415));
#37707=CARTESIAN_POINT('Ctrl Pts',(95.1570985381993,0.666931371096175,-8.44830644189875));
#37708=CARTESIAN_POINT('Ctrl Pts',(95.139013869602,0.628933229001528,-8.44600426796337));
#37709=CARTESIAN_POINT('Ctrl Pts',(95.1153678807133,0.579250060027472,-8.4429941393009));
#37710=CARTESIAN_POINT('Ctrl Pts',(95.0944780102903,0.528127120712406,-8.43998401063843));
#37711=CARTESIAN_POINT('Ctrl Pts',(95.0765192319262,0.475901475178343,-8.43697388197596));
#37712=CARTESIAN_POINT('Ctrl Pts',(95.0585923713712,0.423768649331462,-8.43396910316026));
#37713=CARTESIAN_POINT('Ctrl Pts',(95.0435864351764,0.370537501915542,-8.43096432434456));
#37714=CARTESIAN_POINT('Ctrl Pts',(95.031628985914,0.316566447900545,-8.42795954552886));
#37715=CARTESIAN_POINT('Ctrl Pts',(95.0196833665665,0.262648789301595,-8.42495773944396));
#37716=CARTESIAN_POINT('Ctrl Pts',(95.0107803733285,0.207993187268241,-8.42195593335907));
#37717=CARTESIAN_POINT('Ctrl Pts',(95.0049976772048,0.152972853293195,-8.41895412727417));
#37718=CARTESIAN_POINT('Ctrl Pts',(94.9992184180757,0.0979852211221702,
-8.41595410533829));
#37719=CARTESIAN_POINT('Ctrl Pts',(94.9965558352626,0.042633810859308,-8.4129540834024));
#37720=CARTESIAN_POINT('Ctrl Pts',(94.9970360603772,-0.012700640730549,
-8.40995406146651));
#37721=CARTESIAN_POINT('Ctrl Pts',(94.997516189732,-0.0680240582965324,
-8.40695463775312));
#37722=CARTESIAN_POINT('Ctrl Pts',(95.0011378778449,-0.123329996105209,
-8.40395521403973));
#37723=CARTESIAN_POINT('Ctrl Pts',(95.0078751538129,-0.178237628217731,
-8.40095579032634));
#37724=CARTESIAN_POINT('Ctrl Pts',(95.0146186237304,-0.233195739945271,
-8.39795360907727));
#37725=CARTESIAN_POINT('Ctrl Pts',(95.0244833396089,-0.287754289076616,
-8.39495142782821));
#37726=CARTESIAN_POINT('Ctrl Pts',(95.0373915751653,-0.341538991092539,
-8.39194924657914));
#37727=CARTESIAN_POINT('Ctrl Pts',(95.050305686264,-0.395348174711013,-8.38894569880381));
#37728=CARTESIAN_POINT('Ctrl Pts',(95.0662659261699,-0.44838230245804,-8.38594215102847));
#37729=CARTESIAN_POINT('Ctrl Pts',(95.0851445311735,-0.500281906741627,
-8.38293860325314));
#37730=CARTESIAN_POINT('Ctrl Pts',(95.1040587663669,-0.552279462793791,
-8.37992938678686));
#37731=CARTESIAN_POINT('Ctrl Pts',(95.1259021606642,-0.603137731515617,
-8.37692017032059));
#37732=CARTESIAN_POINT('Ctrl Pts',(95.1504990670713,-0.652517982516026,
-8.37391095385432));
#37733=CARTESIAN_POINT('Ctrl Pts',(95.1693167084412,-0.690295898108604,
-8.37160877994148));
#37734=CARTESIAN_POINT('Ctrl Pts',(95.1897449444011,-0.727209164653124,
-8.36930660602864));
#37735=CARTESIAN_POINT('Ctrl Pts',(95.2116880189019,-0.763117596636237,
-8.3670044321158));
#37736=CARTESIAN_POINT('Ctrl Pts',(95.2403789345166,-0.810068437177948,
-8.36399430345488));
#37737=CARTESIAN_POINT('Ctrl Pts',(95.2717816288482,-0.855497639194487,
-8.36098417479396));
#37738=CARTESIAN_POINT('Ctrl Pts',(95.3057094065078,-0.899074487079725,
-8.35797404613304));
#37739=CARTESIAN_POINT('Ctrl Pts',(95.3395768849468,-0.942573886627629,
-8.35496926731891));
#37740=CARTESIAN_POINT('Ctrl Pts',(95.3759602188609,-0.984227052009934,
-8.35196448850478));
#37741=CARTESIAN_POINT('Ctrl Pts',(95.4146289257559,-1.02373130960683,-8.34895970969066));
#37742=CARTESIAN_POINT('Ctrl Pts',(95.4532593763718,-1.06319648428564,-8.34595790360735));
#37743=CARTESIAN_POINT('Ctrl Pts',(95.4941703534348,-1.10051658711055,-8.34295609752405));
#37744=CARTESIAN_POINT('Ctrl Pts',(95.537091721408,-1.13542264523016,-8.33995429144075));
#37745=CARTESIAN_POINT('Ctrl Pts',(95.5799875787004,-1.17030795663668,-8.33695426950647));
#37746=CARTESIAN_POINT('Ctrl Pts',(95.6248910496381,-1.20278173467422,-8.3339542475722));
#37747=CARTESIAN_POINT('Ctrl Pts',(95.6714975351442,-1.23261406034087,-8.33095422563792));
#37748=CARTESIAN_POINT('Ctrl Pts',(95.7180947270356,-1.26244043726151,-8.32795480192614));
#37749=CARTESIAN_POINT('Ctrl Pts',(95.7663938145319,-1.28962612330611,-8.32495537821437));
#37750=CARTESIAN_POINT('Ctrl Pts',(95.8160616552611,-1.31398478800686,-8.32195595450259));
#37751=CARTESIAN_POINT('Ctrl Pts',(95.865775158376,-1.33836584697168,-8.31895377325515));
#37752=CARTESIAN_POINT('Ctrl Pts',(95.9168594536031,-1.3599144590114,-8.31595159200771));
#37753=CARTESIAN_POINT('Ctrl Pts',(95.9689585982489,-1.378491214388,-8.31294941076028));
#37754=CARTESIAN_POINT('Ctrl Pts',(96.0210814572689,-1.39707642549129,-8.30994586298657));
#37755=CARTESIAN_POINT('Ctrl Pts',(96.0742195789598,-1.41268693425598,-8.30694231521287));
#37756=CARTESIAN_POINT('Ctrl Pts',(96.12800208995,-1.42523333454601,-8.30393876743917));
#37757=CARTESIAN_POINT('Ctrl Pts',(96.1818861063786,-1.43780341405514,-8.30092955097451));
#37758=CARTESIAN_POINT('Ctrl Pts',(96.2364164200425,-1.4472977418607,-8.29792033450986));
#37759=CARTESIAN_POINT('Ctrl Pts',(96.2912133622951,-1.45367834609166,-8.2949111180452));
#37760=CARTESIAN_POINT('Ctrl Pts',(96.3331352689248,-1.45855976983201,-8.29260894411955));
#37761=CARTESIAN_POINT('Ctrl Pts',(96.37521303127,-1.46161983639158,-8.29030677019389));
#37762=CARTESIAN_POINT('Ctrl Pts',(96.4172769194585,-1.46286214722424,-8.28800459626824));
#37763=CARTESIAN_POINT('Ctrl Pts',(96.4722761156628,-1.46448648820115,-8.28499446760714));
#37764=CARTESIAN_POINT('Ctrl Pts',(96.5274826038959,-1.46300822420361,-8.28198433894605));
#37765=CARTESIAN_POINT('Ctrl Pts',(96.5825173913096,-1.45840301593532,-8.27897421028495));
#37766=CARTESIAN_POINT('Ctrl Pts',(96.6374543663989,-1.45380599241975,-8.27596943147066));
#37767=CARTESIAN_POINT('Ctrl Pts',(96.6922197242421,-1.44609309713388,-8.27296465265636));
#37768=CARTESIAN_POINT('Ctrl Pts',(96.7464340328068,-1.43529198569189,-8.26995987384207));
#37769=CARTESIAN_POINT('Ctrl Pts',(96.800594705295,-1.42450156016022,-8.2669580677586));
#37770=CARTESIAN_POINT('Ctrl Pts',(96.8542048930735,-1.41062907351296,-8.26395626167513));
#37771=CARTESIAN_POINT('Ctrl Pts',(96.9068917231434,-1.39375380582219,-8.26095445559167));
#37772=CARTESIAN_POINT('Ctrl Pts',(96.959547238347,-1.37688856809057,-8.25795443365723));
#37773=CARTESIAN_POINT('Ctrl Pts',(97.011279981667,-1.3570242475339,-8.25495441172278));
#37774=CARTESIAN_POINT('Ctrl Pts',(97.0617309580119,-1.33429032723655,-8.25195438978834));
#37775=CARTESIAN_POINT('Ctrl Pts',(97.112171874127,-1.31156094022041,-8.24895496607641));
#37776=CARTESIAN_POINT('Ctrl Pts',(97.161331049642,-1.28596330670351,-8.24595554236449));
#37777=CARTESIAN_POINT('Ctrl Pts',(97.2088704000913,-1.25767463215211,-8.24295611865257));
#37778=CARTESIAN_POINT('Ctrl Pts',(97.2564534560878,-1.22935995026172,-8.23995393740497));
#37779=CARTESIAN_POINT('Ctrl Pts',(97.3024132569838,-1.19834955520426,-8.23695175615737));
#37780=CARTESIAN_POINT('Ctrl Pts',(97.3464385576812,-1.16486538563146,-8.23394957490977));
#37781=CARTESIAN_POINT('Ctrl Pts',(97.3904838977182,-1.13136597480799,-8.23094602713592));
#37782=CARTESIAN_POINT('Ctrl Pts',(97.4325925800262,-1.0953908884934,-8.22794247936206));
#37783=CARTESIAN_POINT('Ctrl Pts',(97.4724870808059,-1.0572018919559,-8.2249389315882));
#37784=CARTESIAN_POINT('Ctrl Pts',(97.5124568757418,-1.0189408201144,-8.2219297151234));
#37785=CARTESIAN_POINT('Ctrl Pts',(97.5502037801204,-0.978457878287744,
-8.2189204986586));
#37786=CARTESIAN_POINT('Ctrl Pts',(97.5854885420198,-0.936050301504208,
-8.2159112821938));
#37787=CARTESIAN_POINT('Ctrl Pts',(97.6124828309726,-0.903606767245738,
-8.21360910826943));
#37788=CARTESIAN_POINT('Ctrl Pts',(97.6380368432212,-0.870037517218503,
-8.21130693434505));
#37789=CARTESIAN_POINT('Ctrl Pts',(97.6620608553443,-0.835486672578546,
-8.20900476042068));
#37790=CARTESIAN_POINT('Ctrl Pts',(97.6938285605627,-0.789799006340861,
-8.20596052358728));
#37791=CARTESIAN_POINT('Ctrl Pts',(97.7230514378139,-0.742204285146314,
-8.20291628675389));
#37792=CARTESIAN_POINT('Ctrl Pts',(97.7494980213216,-0.693013159147089,
-8.19987204992049));
#37793=CARTESIAN_POINT('Ctrl Pts',(97.7759001255963,-0.643904765329677,
-8.19683293304217));
#37794=CARTESIAN_POINT('Ctrl Pts',(97.7995349562016,-0.593205739149372,
-8.19379381616385));
#37795=CARTESIAN_POINT('Ctrl Pts',(97.8202141814697,-0.541255751088821,
-8.19075469928553));
#37796=CARTESIAN_POINT('Ctrl Pts',(97.8408626648377,-0.489382992291977,
-8.18772010038243));
#37797=CARTESIAN_POINT('Ctrl Pts',(97.8585640806866,-0.436263438544642,
-8.18468550147933));
#37798=CARTESIAN_POINT('Ctrl Pts',(97.8731769705423,-0.382259339125534,
-8.18165090257623));
#37799=CARTESIAN_POINT('Ctrl Pts',(97.8877772492243,-0.328301846167547,
-8.17861892258387));
#37800=CARTESIAN_POINT('Ctrl Pts',(97.8992941568264,-0.27346181511333,-8.1755869425915));
#37801=CARTESIAN_POINT('Ctrl Pts',(97.9076357256374,-0.218117638272708,
-8.17255496259914));
#37802=CARTESIAN_POINT('Ctrl Pts',(97.9159735880353,-0.162798052535111,
-8.16952432980781));
#37803=CARTESIAN_POINT('Ctrl Pts',(97.9211388342734,-0.106975271404341,
-8.16649369701649));
#37804=CARTESIAN_POINT('Ctrl Pts',(97.9230907703806,-0.0510368698973246,
-8.16346306422516));
#37805=CARTESIAN_POINT('Ctrl Pts',(97.9236936227492,-0.0337603833765289,
-8.16252705809774));
#37806=CARTESIAN_POINT('Ctrl Pts',(97.9239903389913,-0.016472908141087,
-8.16159105197031));
#37807=CARTESIAN_POINT('Ctrl Pts',(97.9239807231659,0.000814067132374142,
-8.16065504584289));
#37808=CARTESIAN_POINT('Ctrl Pts',(97.9239807535765,0.000757425470412684,
-8.08934495415708));
#37809=CARTESIAN_POINT('Ctrl Pts',(97.9240097899909,-0.0553468229746924,
-8.09238220454818));
#37810=CARTESIAN_POINT('Ctrl Pts',(97.9208082948967,-0.111450673046662,
-8.09541945493928));
#37811=CARTESIAN_POINT('Ctrl Pts',(97.9144027461864,-0.167163570625104,
-8.09845670533038));
#37812=CARTESIAN_POINT('Ctrl Pts',(97.9079948428155,-0.222896948098714,
-8.10149507220567));
#37813=CARTESIAN_POINT('Ctrl Pts',(97.8983806086794,-0.278238582411924,
-8.10453343908097));
#37814=CARTESIAN_POINT('Ctrl Pts',(97.8856381128755,-0.332805213148775,
-8.10757180595627));
#37815=CARTESIAN_POINT('Ctrl Pts',(97.8728767166415,-0.387452780368249,
-8.11061467951861));
#37816=CARTESIAN_POINT('Ctrl Pts',(97.8569779203156,-0.441322554640103,
-8.11365755308095));
#37817=CARTESIAN_POINT('Ctrl Pts',(97.8380701510059,-0.494044777430771,
-8.11670042664329));
#37818=CARTESIAN_POINT('Ctrl Pts',(97.8191457289805,-0.546813434476251,
-8.11974598016787));
#37819=CARTESIAN_POINT('Ctrl Pts',(97.7972072600667,-0.598432060855823,
-8.12279153369245));
#37820=CARTESIAN_POINT('Ctrl Pts',(97.7724307275929,-0.648552256926193,
-8.12583708721703));
#37821=CARTESIAN_POINT('Ctrl Pts',(97.7476053007107,-0.698771360999091,
-8.12888865088602));
#37822=CARTESIAN_POINT('Ctrl Pts',(97.7199308884093,-0.747485693921532,
-8.131940214555));
#37823=CARTESIAN_POINT('Ctrl Pts',(97.6896280054007,-0.794373819533371,
-8.13499177822398));
#37824=CARTESIAN_POINT('Ctrl Pts',(97.6830365696656,-0.804572851309346,
-8.1356555495823));
#37825=CARTESIAN_POINT('Ctrl Pts',(97.6763209229621,-0.814685599609082,
-8.13631932094062));
#37826=CARTESIAN_POINT('Ctrl Pts',(97.6694835840665,-0.824708966725532,
-8.13698309229894));
#37827=CARTESIAN_POINT('Ctrl Pts',(97.6384770190523,-0.870163812375409,
-8.13999322096016));
#37828=CARTESIAN_POINT('Ctrl Pts',(97.6048382945268,-0.913963102553137,
-8.14300334962138));
#37829=CARTESIAN_POINT('Ctrl Pts',(97.5687704363409,-0.955785887910356,
-8.1460134782826));
#37830=CARTESIAN_POINT('Ctrl Pts',(97.5327666809018,-0.997534342393602,
-8.14901825709703));
#37831=CARTESIAN_POINT('Ctrl Pts',(97.4943427015374,-1.03731286654272,-8.15202303591145));
#37832=CARTESIAN_POINT('Ctrl Pts',(97.4537438516837,-1.07483071099524,-8.15502781472588));
#37833=CARTESIAN_POINT('Ctrl Pts',(97.4131851676658,-1.11231143775637,-8.15802962080948));
#37834=CARTESIAN_POINT('Ctrl Pts',(97.370456261476,-1.14753555868958,-8.16103142689308));
#37835=CARTESIAN_POINT('Ctrl Pts',(97.3258404018259,-1.18024796903173,-8.16403323297668));
#37836=CARTESIAN_POINT('Ctrl Pts',(97.2812510599921,-1.21294093647409,-8.16703325491126));
#37837=CARTESIAN_POINT('Ctrl Pts',(97.2347774126897,-1.24312484061645,-8.17003327684584));
#37838=CARTESIAN_POINT('Ctrl Pts',(97.1867351927932,-1.27058530772654,-8.17303329878042));
#37839=CARTESIAN_POINT('Ctrl Pts',(97.1387025528057,-1.2980402990535,-8.1760327224925));
#37840=CARTESIAN_POINT('Ctrl Pts',(97.0891024196415,-1.3227726699336,-8.17903214620457));
#37841=CARTESIAN_POINT('Ctrl Pts',(97.038276850392,-1.34461301012647,-8.18203156991665));
#37842=CARTESIAN_POINT('Ctrl Pts',(96.9874045543932,-1.36647342934882,-8.18503375116439));
#37843=CARTESIAN_POINT('Ctrl Pts',(96.935305057744,-1.38543629698991,-8.18803593241213));
#37844=CARTESIAN_POINT('Ctrl Pts',(96.8823408390857,-1.4013802066619,-8.19103811365987));
#37845=CARTESIAN_POINT('Ctrl Pts',(96.8293525122906,-1.41733137364766,-8.19404166143388));
#37846=CARTESIAN_POINT('Ctrl Pts',(96.7754991932863,-1.4302607198618,-8.19704520920788));
#37847=CARTESIAN_POINT('Ctrl Pts',(96.7211557680833,-1.44009752759898,-8.20004875698189));
#37848=CARTESIAN_POINT('Ctrl Pts',(96.666709778811,-1.4499529006553,-8.20305797344684));
#37849=CARTESIAN_POINT('Ctrl Pts',(96.6117723609819,-1.45670401105588,-8.20606718991179));
#37850=CARTESIAN_POINT('Ctrl Pts',(96.5567246086163,-1.46033195133666,-8.20907640637675));
#37851=CARTESIAN_POINT('Ctrl Pts',(96.5146108220191,-1.46310747433635,-8.21137858029999));
#37852=CARTESIAN_POINT('Ctrl Pts',(96.4724326030032,-1.46405611982685,-8.21368075422325));
#37853=CARTESIAN_POINT('Ctrl Pts',(96.4303592880104,-1.46318998612773,-8.2159829281465));
#37854=CARTESIAN_POINT('Ctrl Pts',(96.3753477660521,-1.46205750267555,-8.21899305680768));
#37855=CARTESIAN_POINT('Ctrl Pts',(96.3202846147334,-1.45781592578264,-8.22200318546886));
#37856=CARTESIAN_POINT('Ctrl Pts',(96.2655495702991,-1.45045992959917,-8.22501331413004));
#37857=CARTESIAN_POINT('Ctrl Pts',(96.2109118054615,-1.44311700709362,-8.22801809294442));
#37858=CARTESIAN_POINT('Ctrl Pts',(96.1566015094434,-1.432670719714,-8.23102287175881));
#37859=CARTESIAN_POINT('Ctrl Pts',(96.102996252815,-1.4191676932558,-8.2340276505732));
#37860=CARTESIAN_POINT('Ctrl Pts',(96.049444029707,-1.40567802580518,-8.23702945665676));
#37861=CARTESIAN_POINT('Ctrl Pts',(95.9965959738366,-1.38913773831285,-8.24003126274032));
#37862=CARTESIAN_POINT('Ctrl Pts',(95.9448205192203,-1.36964468770713,-8.24303306882389));
#37863=CARTESIAN_POINT('Ctrl Pts',(95.8930758377866,-1.35016322296212,-8.24603309075843));
#37864=CARTESIAN_POINT('Ctrl Pts',(95.842402987282,-1.32773265933758,-8.24903311269297));
#37865=CARTESIAN_POINT('Ctrl Pts',(95.7931540266796,-1.30250029864732,-8.25203313462751));
#37866=CARTESIAN_POINT('Ctrl Pts',(95.7439148866177,-1.27727296944229,-8.25503255833954));
#37867=CARTESIAN_POINT('Ctrl Pts',(95.6960995423354,-1.24924519339181,-8.25803198205157));
#37868=CARTESIAN_POINT('Ctrl Pts',(95.6500367781202,-1.21861088742537,-8.2610314057636));
#37869=CARTESIAN_POINT('Ctrl Pts',(95.6039316658649,-1.18794841765161,-8.26403358701131));
#37870=CARTESIAN_POINT('Ctrl Pts',(95.5595827934227,-1.15467492349639,-8.26703576825901));
#37871=CARTESIAN_POINT('Ctrl Pts',(95.5172898988173,-1.1190276546032,-8.27003794950671));
#37872=CARTESIAN_POINT('Ctrl Pts',(95.4749777534251,-1.08336415986454,-8.27304149728068));
#37873=CARTESIAN_POINT('Ctrl Pts',(95.4347238359076,-1.04532509986401,-8.27604504505464));
#37874=CARTESIAN_POINT('Ctrl Pts',(95.3967922104908,-1.00518581184832,-8.2790485928286));
#37875=CARTESIAN_POINT('Ctrl Pts',(95.3587889955147,-0.964970767681657,
-8.28205780929351));
#37876=CARTESIAN_POINT('Ctrl Pts',(95.3231171694233,-0.922647981944113,
-8.28506702575842));
#37877=CARTESIAN_POINT('Ctrl Pts',(95.2900007960032,-0.878526300169629,
-8.28807624222333));
#37878=CARTESIAN_POINT('Ctrl Pts',(95.2646654131152,-0.844771405355678,
-8.2903784161469));
#37879=CARTESIAN_POINT('Ctrl Pts',(95.2408248836876,-0.809964347957286,
-8.29268059007048));
#37880=CARTESIAN_POINT('Ctrl Pts',(95.2185615998193,-0.774253562276169,
-8.29498276399405));
#37881=CARTESIAN_POINT('Ctrl Pts',(95.1894520055427,-0.727561147598254,
-8.29799289265546));
#37882=CARTESIAN_POINT('Ctrl Pts',(95.1629181506182,-0.679126695490427,
-8.30100302131687));
#37883=CARTESIAN_POINT('Ctrl Pts',(95.1391719819818,-0.629265335254224,
-8.30401314997828));
#37884=CARTESIAN_POINT('Ctrl Pts',(95.1154680169781,-0.57949259270458,-8.3070179287929));
#37885=CARTESIAN_POINT('Ctrl Pts',(95.0945421312549,-0.528298447719727,
-8.31002270760752));
#37886=CARTESIAN_POINT('Ctrl Pts',(95.0765615775312,-0.476024601965427,
-8.31302748642213));
#37887=CARTESIAN_POINT('Ctrl Pts',(95.0585988125865,-0.423802472521088,
-8.31602929250593));
#37888=CARTESIAN_POINT('Ctrl Pts',(95.0435757782425,-0.370503255274074,
-8.31903109858972));
#37889=CARTESIAN_POINT('Ctrl Pts',(95.0316118275887,-0.316488992270534,
-8.32203290467351));
#37890=CARTESIAN_POINT('Ctrl Pts',(95.0196549878109,-0.262506833104415,
-8.32503292660828));
#37891=CARTESIAN_POINT('Ctrl Pts',(95.0107537419261,-0.207810985136718,
-8.32803294854305));
#37892=CARTESIAN_POINT('Ctrl Pts',(95.0049770843418,-0.152776792365372,
-8.33103297047782));
#37893=CARTESIAN_POINT('Ctrl Pts',(94.999201578658,-0.0977535737447509,
-8.33403239419009));
#37894=CARTESIAN_POINT('Ctrl Pts',(94.9965494790006,-0.0423926692451935,
-8.33703181790235));
#37895=CARTESIAN_POINT('Ctrl Pts',(94.9970380211664,0.0129245999948381,
-8.34003124161461));
#37896=CARTESIAN_POINT('Ctrl Pts',(94.9975270124759,0.0682927254517481,
-8.34303342286254));
#37897=CARTESIAN_POINT('Ctrl Pts',(95.0011624095153,0.123616606271708,-8.34603560411046));
#37898=CARTESIAN_POINT('Ctrl Pts',(95.0079092850023,0.178515571519108,-8.34903778535839));
#37899=CARTESIAN_POINT('Ctrl Pts',(95.0146592315174,0.233439525556841,-8.35204133313258));
#37900=CARTESIAN_POINT('Ctrl Pts',(95.024523385504,0.287937657889964,-8.35504488090677));
#37901=CARTESIAN_POINT('Ctrl Pts',(95.0374154282645,0.341638364431615,-8.35804842868096));
#37902=CARTESIAN_POINT('Ctrl Pts',(95.050331802586,0.395440422019282,-8.36105764514609));
#37903=CARTESIAN_POINT('Ctrl Pts',(95.0662873289335,0.448441540391401,-8.36406686161122));
#37904=CARTESIAN_POINT('Ctrl Pts',(95.0851457684338,0.500285308109187,-8.36707607807635));
#37905=CARTESIAN_POINT('Ctrl Pts',(95.0995732475221,0.539947915112886,-8.3693782519981));
#37906=CARTESIAN_POINT('Ctrl Pts',(95.1156987231514,0.578933439619426,-8.37168042591986));
#37907=CARTESIAN_POINT('Ctrl Pts',(95.1334428963189,0.617091772109208,-8.37398259984161));
#37908=CARTESIAN_POINT('Ctrl Pts',(95.1566436821995,0.666984392819094,-8.37699272850269));
#37909=CARTESIAN_POINT('Ctrl Pts',(95.182710845181,0.715671604914427,-8.38000285716377));
#37910=CARTESIAN_POINT('Ctrl Pts',(95.2114962629664,0.762803711718899,-8.38301298582484));
#37911=CARTESIAN_POINT('Ctrl Pts',(95.2402305209534,0.809852051489189,-8.38601776463913));
#37912=CARTESIAN_POINT('Ctrl Pts',(95.2716731733469,0.855350323806835,-8.38902254345341));
#37913=CARTESIAN_POINT('Ctrl Pts',(95.3056294220346,0.898971745569833,-8.39202732226769));
#37914=CARTESIAN_POINT('Ctrl Pts',(95.3395520766398,0.942550011162923,-8.39502912835115));
#37915=CARTESIAN_POINT('Ctrl Pts',(95.3759830785269,0.984254689808661,-8.39803093443462));
#37916=CARTESIAN_POINT('Ctrl Pts',(95.4146844217983,1.02378800172987,-8.40103274051808));
#37917=CARTESIAN_POINT('Ctrl Pts',(95.4533627625966,1.06329781669037,-8.40403276245252));
#37918=CARTESIAN_POINT('Ctrl Pts',(95.4943084014814,1.1006384462905,-8.40703278438696));
#37919=CARTESIAN_POINT('Ctrl Pts',(95.5372446760263,1.13554701937008,-8.4100328063214));
#37920=CARTESIAN_POINT('Ctrl Pts',(95.5801723888186,1.17044863146918,-8.41303223003334));
#37921=CARTESIAN_POINT('Ctrl Pts',(95.6250895394138,1.20291881720026,-8.41603165374527));
#37922=CARTESIAN_POINT('Ctrl Pts',(95.6716861786677,1.23273478874661,-8.4190310774572));
#37923=CARTESIAN_POINT('Ctrl Pts',(95.7183256567825,1.26257817176033,-8.42203325870481));
#37924=CARTESIAN_POINT('Ctrl Pts',(95.7666472625621,1.28976218020096,-8.42503543995242));
#37925=CARTESIAN_POINT('Ctrl Pts',(95.8163130897231,1.31410806950236,-8.42803762120003));
#37926=CARTESIAN_POINT('Ctrl Pts',(95.8660015236662,1.33846504051217,-8.4310411689739));
#37927=CARTESIAN_POINT('Ctrl Pts',(95.9170349112087,1.35998111164486,-8.43404471674778));
#37928=CARTESIAN_POINT('Ctrl Pts',(95.9690548597294,1.37852553411864,-8.43704826452165));
#37929=CARTESIAN_POINT('Ctrl Pts',(96.0211729871483,1.39710495606895,-8.44005748098647));
#37930=CARTESIAN_POINT('Ctrl Pts',(96.074280887155,1.41270137636238,-8.4430666974513));
#37931=CARTESIAN_POINT('Ctrl Pts',(96.1280056151919,1.42523415691089,-8.44607591391612));
#37932=CARTESIAN_POINT('Ctrl Pts',(96.1691072339771,1.43482224766995,-8.44837808784047));
#37933=CARTESIAN_POINT('Ctrl Pts',(96.2105695565938,1.44261826540528,-8.45068026176483));
#37934=CARTESIAN_POINT('Ctrl Pts',(96.2522235336151,1.44860660591372,-8.45298243568918));
#37935=CARTESIAN_POINT('Ctrl Pts',(96.3066867645409,1.45643645543342,-8.4559925643501));
#37936=CARTESIAN_POINT('Ctrl Pts',(96.3617066105067,1.46120700645383,-8.45900269301103));
#37937=CARTESIAN_POINT('Ctrl Pts',(96.4169092576931,1.46285124249404,-8.46201282167196));
#37938=CARTESIAN_POINT('Ctrl Pts',(96.4720137942209,1.46449255626352,-8.46501760048609));
#37939=CARTESIAN_POINT('Ctrl Pts',(96.5272999636119,1.46301856605602,-8.46802237930021));
#37940=CARTESIAN_POINT('Ctrl Pts',(96.5823876392997,1.45841386752898,-8.47102715811434));
#37941=CARTESIAN_POINT('Ctrl Pts',(96.6374208148589,1.45381372458827,-8.47402896419764));
#37942=CARTESIAN_POINT('Ctrl Pts',(96.6922553620343,1.44608905273922,-8.47703077028094));
#37943=CARTESIAN_POINT('Ctrl Pts',(96.74651183676,1.43527648262532,-8.48003257636424));
#37944=CARTESIAN_POINT('Ctrl Pts',(96.8007360636878,1.42447033905457,-8.48303259829852));
#37945=CARTESIAN_POINT('Ctrl Pts',(96.8543823822712,1.41058003795155,-8.4860326202328));
#37946=CARTESIAN_POINT('Ctrl Pts',(96.9070794635753,1.39369365977409,-8.48903264216708));
#37947=CARTESIAN_POINT('Ctrl Pts',(96.9597660367627,1.37681064884258,-8.49203206587885));
#37948=CARTESIAN_POINT('Ctrl Pts',(97.0115032459361,1.3569329083871,-8.49503148959061));
#37949=CARTESIAN_POINT('Ctrl Pts',(97.0619351453074,1.33419829876907,-8.49803091330237));
#37950=CARTESIAN_POINT('Ctrl Pts',(97.1124134095059,1.31144278797029,-8.50103309454981));
#37951=CARTESIAN_POINT('Ctrl Pts',(97.1615834838807,1.28582537815449,-8.50403527579725));
#37952=CARTESIAN_POINT('Ctrl Pts',(97.2091110343805,1.25753140959865,-8.50703745704469));
#37953=CARTESIAN_POINT('Ctrl Pts',(97.2566602183662,1.2292245622564,-8.51004100481839));
#37954=CARTESIAN_POINT('Ctrl Pts',(97.3025649496152,1.19823902353762,-8.51304455259209));
#37955=CARTESIAN_POINT('Ctrl Pts',(97.3465198981824,1.16480351628688,-8.51604810036579));
#37956=CARTESIAN_POINT('Ctrl Pts',(97.3905578043177,1.13130490514315,-8.51905731683044));
#37957=CARTESIAN_POINT('Ctrl Pts',(97.4326381741408,1.09534743242449,-8.52206653329509));
#37958=CARTESIAN_POINT('Ctrl Pts',(97.4724896956406,1.05719938890008,-8.52507574975974));
#37959=CARTESIAN_POINT('Ctrl Pts',(97.5029777428691,1.02801457213837,-8.52737792368541));
#37960=CARTESIAN_POINT('Ctrl Pts',(97.5321619678664,0.997548474543418,-8.52968009761107));
#37961=CARTESIAN_POINT('Ctrl Pts',(97.5599369337489,0.965934153484868,-8.53198227153674));
#37962=CARTESIAN_POINT('Ctrl Pts',(97.5959137013808,0.924984289230303,-8.53496426534808));
#37963=CARTESIAN_POINT('Ctrl Pts',(97.6296825206123,0.881927048582567,-8.53794625915942));
#37964=CARTESIAN_POINT('Ctrl Pts',(97.6609847719527,0.83703215139049,-8.54092825297077));
#37965=CARTESIAN_POINT('Ctrl Pts',(97.692240926784,0.792203367591167,-8.5439058554205));
#37966=CARTESIAN_POINT('Ctrl Pts',(97.7210373999692,0.745542722705404,-8.54688345787024));
#37967=CARTESIAN_POINT('Ctrl Pts',(97.7471547911784,0.697354053073913,-8.54986106031997));
#37968=CARTESIAN_POINT('Ctrl Pts',(97.7732445159323,0.649216430258924,-8.5528355085609));
#37969=CARTESIAN_POINT('Ctrl Pts',(97.7966605255636,0.599554460627301,-8.55580995680183));
#37970=CARTESIAN_POINT('Ctrl Pts',(97.8172272417484,0.548700053470984,-8.55878440504276));
#37971=CARTESIAN_POINT('Ctrl Pts',(97.8377852922579,0.497867073545964,-8.56175760001591));
#37972=CARTESIAN_POINT('Ctrl Pts',(97.8554962169165,0.445843146258828,-8.56473079498905));
#37973=CARTESIAN_POINT('Ctrl Pts',(97.8702318258466,0.392981827642424,-8.56770398996219));
#37974=CARTESIAN_POINT('Ctrl Pts',(97.8849638022446,0.340133540074315,-8.57067645200153));
#37975=CARTESIAN_POINT('Ctrl Pts',(97.8967217797702,0.286448791372774,-8.57364891404087));
#37976=CARTESIAN_POINT('Ctrl Pts',(97.9054276944835,0.232295403278304,-8.57662137608021));
#37977=CARTESIAN_POINT('Ctrl Pts',(97.9141388930535,0.178109148017274,-8.57959564218774));
#37978=CARTESIAN_POINT('Ctrl Pts',(97.919794254375,0.123454219241105,-8.58256990829528));
#37979=CARTESIAN_POINT('Ctrl Pts',(97.9223673234851,0.068705747808685,-8.58554417440281));
#37980=CARTESIAN_POINT('Ctrl Pts',(97.9234633550916,0.0453849380947507,
-8.58681110098756));
#37981=CARTESIAN_POINT('Ctrl Pts',(97.9240007683061,0.0220471905637543,
-8.58807802757232));
#37982=CARTESIAN_POINT('Ctrl Pts',(97.9239803911309,-0.00127850362627049,
-8.58934495415707));
#37983=CARTESIAN_POINT('Origin',(96.460480949577,-8.32667268468867E-16,
1.18130019239114E-14));
#37984=CARTESIAN_POINT('',(97.9239808950412,0.000399532766094337,-9.16065504589061));
#37985=CARTESIAN_POINT('',(97.9239808729693,0.000473530088810134,-9.08934495421004));
#37986=CARTESIAN_POINT('',(97.923980949577,-1.01189432752408E-15,1.19922289829666E-14));
#37987=CARTESIAN_POINT('Ctrl Pts',(97.9239808950409,0.000399533638512916,
-9.1606550458429));
#37988=CARTESIAN_POINT('Ctrl Pts',(97.9239748177392,0.0226608147838017,
-9.15943762742574));
#37989=CARTESIAN_POINT('Ctrl Pts',(97.9234608417589,0.0449144548143451,
-9.15822020900858));
#37990=CARTESIAN_POINT('Ctrl Pts',(97.9224398574859,0.0671446318459906,
-9.15700279059142));
#37991=CARTESIAN_POINT('Ctrl Pts',(97.9199154218029,0.122109878251946,-9.15399266146905));
#37992=CARTESIAN_POINT('Ctrl Pts',(97.9142815808914,0.177048047496928,-9.15098253234669));
#37993=CARTESIAN_POINT('Ctrl Pts',(97.9055426216486,0.231579390079305,-9.14797240322433));
#37994=CARTESIAN_POINT('Ctrl Pts',(97.8968191939719,0.286013815269212,-9.14496762394028));
#37995=CARTESIAN_POINT('Ctrl Pts',(97.8850016826745,0.340042331438279,-9.14196284465623));
#37996=CARTESIAN_POINT('Ctrl Pts',(97.8701462548443,0.393288668951429,-9.13895806537219));
#37997=CARTESIAN_POINT('Ctrl Pts',(97.8553055239727,0.446482328128939,-9.13595625881414));
#37998=CARTESIAN_POINT('Ctrl Pts',(97.8374329715623,0.498894835391729,-9.1329544522561));
#37999=CARTESIAN_POINT('Ctrl Pts',(97.8166357481785,0.550160351379524,-9.12995264569806));
#38000=CARTESIAN_POINT('Ctrl Pts',(97.7958508857723,0.601395397343536,-9.12695262328508));
#38001=CARTESIAN_POINT('Ctrl Pts',(97.7721449959489,0.651484314848645,-9.12395260087211));
#38002=CARTESIAN_POINT('Ctrl Pts',(97.7456742438721,0.700078885768492,-9.12095257845913));
#38003=CARTESIAN_POINT('Ctrl Pts',(97.7192087701952,0.748663766688898,-9.11795315426557));
#38004=CARTESIAN_POINT('Ctrl Pts',(97.6899797816649,0.795754429287383,-9.114953730072));
#38005=CARTESIAN_POINT('Ctrl Pts',(97.6581894545535,0.841027102480651,-9.11195430587844));
#38006=CARTESIAN_POINT('Ctrl Pts',(97.6263699008356,0.886341397347103,-9.10895212414827));
#38007=CARTESIAN_POINT('Ctrl Pts',(97.5919846081353,0.929833930480223,-9.10594994241811));
#38008=CARTESIAN_POINT('Ctrl Pts',(97.5552783364075,0.971211064490668,-9.10294776068794));
#38009=CARTESIAN_POINT('Ctrl Pts',(97.5185553567869,1.0126070324684,-9.09994421243025));
#38010=CARTESIAN_POINT('Ctrl Pts',(97.4795096651337,1.05188530668701,-9.09694066417256));
#38011=CARTESIAN_POINT('Ctrl Pts',(97.4384231939164,1.08878887610795,-9.09393711591487));
#38012=CARTESIAN_POINT('Ctrl Pts',(97.3972591789663,1.12576209474541,-9.09092789897022));
#38013=CARTESIAN_POINT('Ctrl Pts',(97.3540471035433,1.1603513245554,-9.08791868202556));
#38014=CARTESIAN_POINT('Ctrl Pts',(97.3091013852761,1.19234039020483,-9.08490946508091));
#38015=CARTESIAN_POINT('Ctrl Pts',(97.2747161311802,1.21681329203075,-9.08260729496858));
#38016=CARTESIAN_POINT('Ctrl Pts',(97.2393168890532,1.23976519452232,-9.08030512485625));
#38017=CARTESIAN_POINT('Ctrl Pts',(97.2030541301642,1.26111748916295,-9.07800295474392));
#38018=CARTESIAN_POINT('Ctrl Pts',(97.1556399234842,1.28903599680548,-9.0749928260923));
#38019=CARTESIAN_POINT('Ctrl Pts',(97.106549428113,1.3143355000925,-9.07198269744068));
#38020=CARTESIAN_POINT('Ctrl Pts',(97.0561030366792,1.33681209575469,-9.06897256878906));
#38021=CARTESIAN_POINT('Ctrl Pts',(97.0057463026643,1.35924874418782,-9.06596778998226));
#38022=CARTESIAN_POINT('Ctrl Pts',(96.9540389333658,1.37887222826887,-9.06296301117545));
#38023=CARTESIAN_POINT('Ctrl Pts',(96.9013267540754,1.39552399716242,-9.05995823236864));
#38024=CARTESIAN_POINT('Ctrl Pts',(96.8486667247321,1.41215929189612,-9.05695642629144));
#38025=CARTESIAN_POINT('Ctrl Pts',(96.7950043557571,1.42582853717711,-9.05395462021423));
#38026=CARTESIAN_POINT('Ctrl Pts',(96.7407045939896,1.43642158126091,-9.05095281413702));
#38027=CARTESIAN_POINT('Ctrl Pts',(96.686437105726,1.44700832928305,-9.0479527922076));
#38028=CARTESIAN_POINT('Ctrl Pts',(96.6315334928645,1.45452239912856,-9.04495277027818));
#38029=CARTESIAN_POINT('Ctrl Pts',(96.5763707253807,1.45890431826908,-9.04195274834876));
#38030=CARTESIAN_POINT('Ctrl Pts',(96.5212189576633,1.46328536363025,-9.03895332464061));
#38031=CARTESIAN_POINT('Ctrl Pts',(96.4658086641142,1.46453545685631,-9.03595390093245));
#38032=CARTESIAN_POINT('Ctrl Pts',(96.4105214799486,1.46264701872818,-9.03295447722429));
#38033=CARTESIAN_POINT('Ctrl Pts',(96.3551834671884,1.46075684445347,-9.02995229597849));
#38034=CARTESIAN_POINT('Ctrl Pts',(96.2999693188758,1.45572239218327,-9.02695011473269));
#38035=CARTESIAN_POINT('Ctrl Pts',(96.2452587000085,1.44758821261113,-9.02394793348689));
#38036=CARTESIAN_POINT('Ctrl Pts',(96.1905231780621,1.43945033053805,-9.02094438571373));
#38037=CARTESIAN_POINT('Ctrl Pts',(96.1362921604736,1.42821001594495,-9.01794083794056));
#38038=CARTESIAN_POINT('Ctrl Pts',(96.0829349476038,1.41396296500086,-9.0149372901674));
#38039=CARTESIAN_POINT('Ctrl Pts',(96.0294770319419,1.39968902513713,-9.01192807370148));
#38040=CARTESIAN_POINT('Ctrl Pts',(95.9768967183659,1.38239717819773,-9.00891885723555));
#38041=CARTESIAN_POINT('Ctrl Pts',(95.9255468559991,1.36223264001712,-9.00590964076962));
#38042=CARTESIAN_POINT('Ctrl Pts',(95.8862621062263,1.34680594167364,-9.00360746681184));
#38043=CARTESIAN_POINT('Ctrl Pts',(95.8476971975314,1.32969892730821,-9.00130529285405));
#38044=CARTESIAN_POINT('Ctrl Pts',(95.8100001843338,1.31099466972547,-8.99900311889627));
#38045=CARTESIAN_POINT('Ctrl Pts',(95.7607107484999,1.28653855965879,-8.99599299034906));
#38046=CARTESIAN_POINT('Ctrl Pts',(95.7126988815147,1.25924749918696,-8.99298286180186));
#38047=CARTESIAN_POINT('Ctrl Pts',(95.6663104191203,1.22927841376727,-8.98997273325465));
#38048=CARTESIAN_POINT('Ctrl Pts',(95.6200044021485,1.19936259189157,-8.98696795455753));
#38049=CARTESIAN_POINT('Ctrl Pts',(95.5753165039784,1.1667784748072,-8.98396317586041));
#38050=CARTESIAN_POINT('Ctrl Pts',(95.5325684727805,1.13172906890532,-8.9809583971633));
#38051=CARTESIAN_POINT('Ctrl Pts',(95.4898627337063,1.09671433860767,-8.97795659119893));
#38052=CARTESIAN_POINT('Ctrl Pts',(95.4490934661905,1.05923948422606,-8.97495478523457));
#38053=CARTESIAN_POINT('Ctrl Pts',(95.4105523308054,1.01954997203883,-8.9719529792702));
#38054=CARTESIAN_POINT('Ctrl Pts',(95.3720341026954,0.979884049674879,-8.96895295745657));
#38055=CARTESIAN_POINT('Ctrl Pts',(95.3357417490241,0.938006456621444,-8.96595293564295));
#38056=CARTESIAN_POINT('Ctrl Pts',(95.3019310545548,0.894200419785157,-8.96295291382932));
#38057=CARTESIAN_POINT('Ctrl Pts',(95.2681271021593,0.850403118159582,-8.95995349023969));
#38058=CARTESIAN_POINT('Ctrl Pts',(95.2368041486956,0.804678554277653,-8.95695406665006));
#38059=CARTESIAN_POINT('Ctrl Pts',(95.2081770659551,0.757342216613798,-8.95395464306043));
#38060=CARTESIAN_POINT('Ctrl Pts',(95.1795236647701,0.709962360063037,-8.95095246193648));
#38061=CARTESIAN_POINT('Ctrl Pts',(95.1535713598329,0.660968222178031,-8.94795028081252));
#38062=CARTESIAN_POINT('Ctrl Pts',(95.130490286213,0.610702124905847,-8.94494809968857));
#38063=CARTESIAN_POINT('Ctrl Pts',(95.1073987066075,0.560413147636743,-8.94194455203929));
#38064=CARTESIAN_POINT('Ctrl Pts',(95.0871811566967,0.50885154937697,-8.93894100439001));
#38065=CARTESIAN_POINT('Ctrl Pts',(95.0699592726423,0.456378917101341,-8.93593745674073));
#38066=CARTESIAN_POINT('Ctrl Pts',(95.0527048851785,0.40380725155866,-8.93292824040049));
#38067=CARTESIAN_POINT('Ctrl Pts',(95.0384575942161,0.350321628757899,-8.92991902406025));
#38068=CARTESIAN_POINT('Ctrl Pts',(95.0272885729733,0.296296914673333,-8.92690980772));
#38069=CARTESIAN_POINT('Ctrl Pts',(95.0187438100355,0.254965775212202,-8.92460763282959));
#38070=CARTESIAN_POINT('Ctrl Pts',(95.0119996768107,0.213319403626447,-8.92230545793917));
#38071=CARTESIAN_POINT('Ctrl Pts',(95.0070674939591,0.171527190348247,-8.92000328304876));
#38072=CARTESIAN_POINT('Ctrl Pts',(95.0006185897725,0.116883235068071,-8.91699315432163));
#38073=CARTESIAN_POINT('Ctrl Pts',(94.9972420918849,0.0617602724040382,
-8.9139830255945));
#38074=CARTESIAN_POINT('Ctrl Pts',(94.9969955342547,0.00653369260061267,
-8.91097289686737));
#38075=CARTESIAN_POINT('Ctrl Pts',(94.9967494148268,-0.0485947340357235,
-8.90796811798572));
#38076=CARTESIAN_POINT('Ctrl Pts',(94.9996221986122,-0.103825888511681,
-8.90496333910406));
#38077=CARTESIAN_POINT('Ctrl Pts',(95.0056196641916,-0.158779376137817,
-8.9019585602224));
#38078=CARTESIAN_POINT('Ctrl Pts',(95.0116111962741,-0.213678496407335,
-8.89895675407081));
#38079=CARTESIAN_POINT('Ctrl Pts',(95.0207212293115,-0.268299971587273,
-8.89595494791922));
#38080=CARTESIAN_POINT('Ctrl Pts',(95.032903540841,-0.322265406251912,-8.89295314176763));
#38081=CARTESIAN_POINT('Ctrl Pts',(95.0450786117127,-0.376198766112767,
-8.88995311976443));
#38082=CARTESIAN_POINT('Ctrl Pts',(95.0603222256967,-0.429476344186914,
-8.88695309776122));
#38083=CARTESIAN_POINT('Ctrl Pts',(95.0785369323875,-0.481729159750651,
-8.88395307575802));
#38084=CARTESIAN_POINT('Ctrl Pts',(95.0967480069588,-0.533971555796207,
-8.88095365197682));
#38085=CARTESIAN_POINT('Ctrl Pts',(95.1179288239113,-0.585189096742762,
-8.87795422819562));
#38086=CARTESIAN_POINT('Ctrl Pts',(95.1419325582224,-0.635029439991598,
-8.87495480441441));
#38087=CARTESIAN_POINT('Ctrl Pts',(95.1659583604917,-0.684915604220037,
-8.87195262309731));
#38088=CARTESIAN_POINT('Ctrl Pts',(95.1928120354714,-0.733421564348278,
-8.8689504417802));
#38089=CARTESIAN_POINT('Ctrl Pts',(95.2222998404152,-0.780217784285143,
-8.8659482604631));
#38090=CARTESIAN_POINT('Ctrl Pts',(95.2518010675552,-0.827035304825718,
-8.86294471261949));
#38091=CARTESIAN_POINT('Ctrl Pts',(95.2839385077947,-0.872141102954705,
-8.85994116477589));
#38092=CARTESIAN_POINT('Ctrl Pts',(95.3184757837967,-0.915235735387955,
-8.85693761693229));
#38093=CARTESIAN_POINT('Ctrl Pts',(95.3530782430878,-0.958411701678599,
-8.85392840039822));
#38094=CARTESIAN_POINT('Ctrl Pts',(95.3900892320945,-0.999568526048704,
-8.85091918386416));
#38095=CARTESIAN_POINT('Ctrl Pts',(95.4292336792077,-1.03844177369548,-8.84790996733009));
#38096=CARTESIAN_POINT('Ctrl Pts',(95.4591807777146,-1.06818139354997,-8.84560779395378));
#38097=CARTESIAN_POINT('Ctrl Pts',(95.4903757469049,-1.09658518088179,-8.84330562057747));
#38098=CARTESIAN_POINT('Ctrl Pts',(95.5226829035798,-1.12355110027266,-8.84100344720117));
#38099=CARTESIAN_POINT('Ctrl Pts',(95.5649250296687,-1.15880947285163,-8.83799331854705));
#38100=CARTESIAN_POINT('Ctrl Pts',(95.6092470880068,-1.19175635038038,-8.83498318989293));
#38101=CARTESIAN_POINT('Ctrl Pts',(95.6553661155136,-1.22213843486369,-8.83197306123881));
#38102=CARTESIAN_POINT('Ctrl Pts',(95.7014031765153,-1.2524665218232,-8.82896828243136));
#38103=CARTESIAN_POINT('Ctrl Pts',(95.7492304312742,-1.28023857365049,-8.82596350362391));
#38104=CARTESIAN_POINT('Ctrl Pts',(95.7985324464156,-1.30524190446156,-8.82295872481646));
#38105=CARTESIAN_POINT('Ctrl Pts',(95.8477856853823,-1.33022049861977,-8.81995691873976));
#38106=CARTESIAN_POINT('Ctrl Pts',(95.8985103257694,-1.3524355602715,-8.81695511266306));
#38107=CARTESIAN_POINT('Ctrl Pts',(95.9503641954715,-1.37171904819494,-8.81395330658636));
#38108=CARTESIAN_POINT('Ctrl Pts',(96.0021872453858,-1.39099107481361,-8.81095328465859));
#38109=CARTESIAN_POINT('Ctrl Pts',(96.05513770031,-1.40733479755419,-8.80795326273082));
#38110=CARTESIAN_POINT('Ctrl Pts',(96.1088532824566,-1.42063022413133,-8.80495324080305));
#38111=CARTESIAN_POINT('Ctrl Pts',(96.1625581533932,-1.43392299952051,-8.80195381709769));
#38112=CARTESIAN_POINT('Ctrl Pts',(96.217027336194,-1.44416855909082,-8.79895439339232));
#38113=CARTESIAN_POINT('Ctrl Pts',(96.2718855098507,-1.45129735413334,-8.79595496968695));
#38114=CARTESIAN_POINT('Ctrl Pts',(96.3267941176565,-1.4584327030709,-8.7929527884457));
#38115=CARTESIAN_POINT('Ctrl Pts',(96.38209190596,-1.4624454945538,-8.78995060720445));
#38116=CARTESIAN_POINT('Ctrl Pts',(96.437397019156,-1.46331793611516,-8.78694842596319));
#38117=CARTESIAN_POINT('Ctrl Pts',(96.492727306014,-1.46419077479258,-8.78394487819557));
#38118=CARTESIAN_POINT('Ctrl Pts',(96.5480643958186,-1.46192043578959,-8.78094133042795));
#38119=CARTESIAN_POINT('Ctrl Pts',(96.6030283411271,-1.45654127684809,-8.77793778266033));
#38120=CARTESIAN_POINT('Ctrl Pts',(96.6580960216373,-1.45115196564887,-8.77492856620149));
#38121=CARTESIAN_POINT('Ctrl Pts',(96.7127886276902,-1.44264219491228,-8.77191934974266));
#38122=CARTESIAN_POINT('Ctrl Pts',(96.7667343899895,-1.43109785837151,-8.76891013328383));
#38123=CARTESIAN_POINT('Ctrl Pts',(96.8080051100655,-1.42226596756989,-8.76660795930709));
#38124=CARTESIAN_POINT('Ctrl Pts',(96.8488388658894,-1.41165905690412,-8.76430578533036));
#38125=CARTESIAN_POINT('Ctrl Pts',(96.8890760631564,-1.39933501300291,-8.76200361135362));
#38126=CARTESIAN_POINT('Ctrl Pts',(96.9416868308212,-1.38322113195709,-8.75899348270548));
#38127=CARTESIAN_POINT('Ctrl Pts',(96.9934981260025,-1.36410225986774,-8.75598335405734));
#38128=CARTESIAN_POINT('Ctrl Pts',(97.0441431948968,-1.34207698489628,-8.75297322540921));
#38129=CARTESIAN_POINT('Ctrl Pts',(97.0946982532261,-1.32009085504767,-8.74996844660827));
#38130=CARTESIAN_POINT('Ctrl Pts',(97.1440907181985,-1.2952087821968,-8.74696366780734));
#38131=CARTESIAN_POINT('Ctrl Pts',(97.1919701081049,-1.26757873954884,-8.7439588890064));
#38132=CARTESIAN_POINT('Ctrl Pts',(97.2398021292832,-1.23997603225283,-8.74095708293653));
#38133=CARTESIAN_POINT('Ctrl Pts',(97.2861235855885,-1.20963100336278,-8.73795527686666));
#38134=CARTESIAN_POINT('Ctrl Pts',(97.3306067764798,-1.17673841415872,-8.73495347079679));
#38135=CARTESIAN_POINT('Ctrl Pts',(97.3750635284043,-1.14386537494774,-8.73195344887615));
#38136=CARTESIAN_POINT('Ctrl Pts',(97.4176837567095,-1.10844808996118,-8.72895342695551));
#38137=CARTESIAN_POINT('Ctrl Pts',(97.4581690174657,-1.07072441327945,-8.72595340503488));
#38138=CARTESIAN_POINT('Ctrl Pts',(97.4986462052135,-1.0330082589293,-8.72295398133694));
#38139=CARTESIAN_POINT('Ctrl Pts',(97.5369888847219,-0.992986986064892,
-8.719954557639));
#38140=CARTESIAN_POINT('Ctrl Pts',(97.5729337331488,-0.950936934987414,
-8.71695513394106));
#38141=CARTESIAN_POINT('Ctrl Pts',(97.6089116276557,-0.908848224980831,
-8.71395295270764));
#38142=CARTESIAN_POINT('Ctrl Pts',(97.6424869429693,-0.864727412699082,
-8.71095077147421));
#38143=CARTESIAN_POINT('Ctrl Pts',(97.673436133015,-0.818884590751871,-8.70794859024079));
#38144=CARTESIAN_POINT('Ctrl Pts',(97.7043994104438,-0.773020902171533,
-8.70494504248123));
#38145=CARTESIAN_POINT('Ctrl Pts',(97.7327339090918,-0.725434095993351,
-8.70194149472166));
#38146=CARTESIAN_POINT('Ctrl Pts',(97.7582608027001,-0.676461161359394,
-8.6989379469621));
#38147=CARTESIAN_POINT('Ctrl Pts',(97.7838358740242,-0.627395798553031,
-8.69592873051161));
#38148=CARTESIAN_POINT('Ctrl Pts',(97.8065925373085,-0.576939563854436,
-8.69291951406113));
#38149=CARTESIAN_POINT('Ctrl Pts',(97.826399597581,-0.525450756051471,-8.68991029761064));
#38150=CARTESIAN_POINT('Ctrl Pts',(97.8415528112552,-0.486059705802819,
-8.68760812357577));
#38151=CARTESIAN_POINT('Ctrl Pts',(97.8549806423813,-0.446064760952756,
-8.6853059495409));
#38152=CARTESIAN_POINT('Ctrl Pts',(97.8666443708632,-0.405631215066805,
-8.68300377550604));
#38153=CARTESIAN_POINT('Ctrl Pts',(97.8855156283708,-0.340212009061028,
-8.6792789872356));
#38154=CARTESIAN_POINT('Ctrl Pts',(97.8998320831828,-0.273424344156363,
-8.67555419896517));
#38155=CARTESIAN_POINT('Ctrl Pts',(97.9094335351068,-0.205836476083635,
-8.67182941069473));
#38156=CARTESIAN_POINT('Ctrl Pts',(97.9190349870308,-0.138248608010908,
-8.66810462242429));
#38157=CARTESIAN_POINT('Ctrl Pts',(97.9239212489841,-0.0698603808178389,
-8.66437983415386));
#38158=CARTESIAN_POINT('Ctrl Pts',(97.9239804054011,-0.00126206278290129,
-8.66065504588342));
#38159=CARTESIAN_POINT('Ctrl Pts',(97.9239803911303,-0.0012785042514516,
-8.58934495419103));
#38160=CARTESIAN_POINT('Ctrl Pts',(97.9239200622951,-0.0703367154818267,
-8.59309582578319));
#38161=CARTESIAN_POINT('Ctrl Pts',(97.9189678486473,-0.139181005785864,
-8.59684669737536));
#38162=CARTESIAN_POINT('Ctrl Pts',(97.9092372158365,-0.2072137325898,-8.60059756896753));
#38163=CARTESIAN_POINT('Ctrl Pts',(97.9002572469804,-0.269998114631265,
-8.60405908177312));
#38164=CARTESIAN_POINT('Ctrl Pts',(97.8872083114429,-0.332091715069842,
-8.60752059457871));
#38165=CARTESIAN_POINT('Ctrl Pts',(97.8702152329669,-0.393041346724699,
-8.61098210738429));
#38166=CARTESIAN_POINT('Ctrl Pts',(97.8554380660434,-0.446043095769913,
-8.61399223604393));
#38167=CARTESIAN_POINT('Ctrl Pts',(97.8376366364107,-0.498321683240691,
-8.61700236470357));
#38168=CARTESIAN_POINT('Ctrl Pts',(97.8169002182971,-0.549507977599035,
-8.62001249336321));
#38169=CARTESIAN_POINT('Ctrl Pts',(97.7962006546411,-0.600603299489819,
-8.62301727217607));
#38170=CARTESIAN_POINT('Ctrl Pts',(97.7725766509802,-0.650609695299955,
-8.62602205098893));
#38171=CARTESIAN_POINT('Ctrl Pts',(97.7461672626046,-0.699173050462825,
-8.62902682980179));
#38172=CARTESIAN_POINT('Ctrl Pts',(97.7197840019434,-0.747688360231573,
-8.63202863588384));
#38173=CARTESIAN_POINT('Ctrl Pts',(97.6906210664925,-0.794762995788685,
-8.63503044196589));
#38174=CARTESIAN_POINT('Ctrl Pts',(97.6588648612092,-0.840064432255704,
-8.63803224804794));
#38175=CARTESIAN_POINT('Ctrl Pts',(97.6271275304969,-0.885338943428206,
-8.64103226998098));
#38176=CARTESIAN_POINT('Ctrl Pts',(97.5928002875123,-0.928841912857858,
-8.64403229191403));
#38177=CARTESIAN_POINT('Ctrl Pts',(97.5561133566788,-0.970268972248528,
-8.64703231384707));
#38178=CARTESIAN_POINT('Ctrl Pts',(97.519433741441,-1.01168777083333,-8.65003173755762));
#38179=CARTESIAN_POINT('Ctrl Pts',(97.4803957227518,-1.05103108631773,-8.65303116126817));
#38180=CARTESIAN_POINT('Ctrl Pts',(97.439268887824,-1.08802868617618,-8.65603058497872));
#38181=CARTESIAN_POINT('Ctrl Pts',(97.3981042427277,-1.12506029996945,-8.65903276622497));
#38182=CARTESIAN_POINT('Ctrl Pts',(97.3548473382227,-1.1597415356758,-8.66203494747123));
#38183=CARTESIAN_POINT('Ctrl Pts',(97.3098025097481,-1.19184107054108,-8.66503712871748));
#38184=CARTESIAN_POINT('Ctrl Pts',(97.2647371778672,-1.22395521640227,-8.66804067649002));
#38185=CARTESIAN_POINT('Ctrl Pts',(97.2178827472799,-1.25348503680048,-8.67104422426255));
#38186=CARTESIAN_POINT('Ctrl Pts',(97.1695715731776,-1.28024323373403,-8.67404777203509));
#38187=CARTESIAN_POINT('Ctrl Pts',(97.1211692198638,-1.30705193226152,-8.67705698849862));
#38188=CARTESIAN_POINT('Ctrl Pts',(97.0713051076994,-1.33107832783885,-8.68006620496214));
#38189=CARTESIAN_POINT('Ctrl Pts',(97.0203341002193,-1.35218219915658,-8.68307542142567));
#38190=CARTESIAN_POINT('Ctrl Pts',(96.9813391903137,-1.36832752571337,-8.68537759536107));
#38191=CARTESIAN_POINT('Ctrl Pts',(96.9416969107454,-1.38276330684513,-8.68767976929647));
#38192=CARTESIAN_POINT('Ctrl Pts',(96.9015715221215,-1.39544665136734,-8.68998194323187));
#38193=CARTESIAN_POINT('Ctrl Pts',(96.8491069448719,-1.41203032398191,-8.69299207189151));
#38194=CARTESIAN_POINT('Ctrl Pts',(96.7955955896307,-1.42568596254133,-8.69600220055116));
#38195=CARTESIAN_POINT('Ctrl Pts',(96.7413953930831,-1.43628664459072,-8.6990123292108));
#38196=CARTESIAN_POINT('Ctrl Pts',(96.6872915255573,-1.44686848624104,-8.70201710802362));
#38197=CARTESIAN_POINT('Ctrl Pts',(96.6325017603913,-1.45440604574695,-8.70502188683643));
#38198=CARTESIAN_POINT('Ctrl Pts',(96.5773986573295,-1.45882229884722,-8.70802666564925));
#38199=CARTESIAN_POINT('Ctrl Pts',(96.5223500696595,-1.46323418279668,-8.71102847173122));
#38200=CARTESIAN_POINT('Ctrl Pts',(96.4669892820208,-1.46453083556759,-8.71403027781319));
#38201=CARTESIAN_POINT('Ctrl Pts',(96.4116966438851,-1.46268668603982,-8.71703208389516));
#38202=CARTESIAN_POINT('Ctrl Pts',(96.3564368694002,-1.46084363259806,-8.7200321058281));
#38203=CARTESIAN_POINT('Ctrl Pts',(96.3012456909032,-1.45586349447276,-8.72303212776103));
#38204=CARTESIAN_POINT('Ctrl Pts',(96.2465038187545,-1.4477727851721,-8.72603214969396));
#38205=CARTESIAN_POINT('Ctrl Pts',(96.1917728624664,-1.43968368920783,-8.72903157340438));
#38206=CARTESIAN_POINT('Ctrl Pts',(96.1374915567438,-1.42848533106342,-8.73203099711479));
#38207=CARTESIAN_POINT('Ctrl Pts',(96.0840335299944,-1.41425584329343,-8.73503042082521));
#38208=CARTESIAN_POINT('Ctrl Pts',(96.0305263563324,-1.40001327357046,-8.73803260207128));
#38209=CARTESIAN_POINT('Ctrl Pts',(95.9778444852455,-1.38273414292416,-8.74103478331735));
#38210=CARTESIAN_POINT('Ctrl Pts',(95.9263479434552,-1.36254694663021,-8.74403696456342));
#38211=CARTESIAN_POINT('Ctrl Pts',(95.8748279615823,-1.34235056157267,-8.74704051233575));
#38212=CARTESIAN_POINT('Ctrl Pts',(95.8244948653259,-1.31924369291081,-8.75004406010807));
#38213=CARTESIAN_POINT('Ctrl Pts',(95.7756871193749,-1.29340235816901,-8.7530476078804));
#38214=CARTESIAN_POINT('Ctrl Pts',(95.7267872570173,-1.26751225225669,-8.75605682434369));
#38215=CARTESIAN_POINT('Ctrl Pts',(95.679418948962,-1.23887764455704,-8.75906604080697));
#38216=CARTESIAN_POINT('Ctrl Pts',(95.6338935303719,-1.20771912645777,-8.76207525727026));
#38217=CARTESIAN_POINT('Ctrl Pts',(95.5990647191515,-1.1838815829843,-8.76437743120665));
#38218=CARTESIAN_POINT('Ctrl Pts',(95.5653139779917,-1.15856776108484,-8.76667960514303));
#38219=CARTESIAN_POINT('Ctrl Pts',(95.5327669807653,-1.13189179786391,-8.76898177907942));
#38220=CARTESIAN_POINT('Ctrl Pts',(95.4902112694213,-1.09701255592482,-8.77199190775025));
#38221=CARTESIAN_POINT('Ctrl Pts',(95.4495359100341,-1.0596567429178,-8.77500203642108));
#38222=CARTESIAN_POINT('Ctrl Pts',(95.411042778776,-1.02005479052148,-8.7780121650919));
#38223=CARTESIAN_POINT('Ctrl Pts',(95.372618060658,-0.980523221952778,-8.78101694391595));
#38224=CARTESIAN_POINT('Ctrl Pts',(95.3363682390082,-0.938753811825842,
-8.78402172273999));
#38225=CARTESIAN_POINT('Ctrl Pts',(95.3025613889011,-0.895016503202071,
-8.78702650156404));
#38226=CARTESIAN_POINT('Ctrl Pts',(95.2687879850711,-0.851322465398916,
-8.79002830765726));
#38227=CARTESIAN_POINT('Ctrl Pts',(95.2374530863764,-0.805664801623698,
-8.79303011375049));
#38228=CARTESIAN_POINT('Ctrl Pts',(95.208785930777,-0.758348092838164,-8.79603191984371));
#38229=CARTESIAN_POINT('Ctrl Pts',(95.1801358137459,-0.711059507141787,
-8.7990319417879));
#38230=CARTESIAN_POINT('Ctrl Pts',(95.154150570165,-0.662114281668448,-8.80203196373209));
#38231=CARTESIAN_POINT('Ctrl Pts',(95.1310160129044,-0.61184575847036,-8.80503198567627));
#38232=CARTESIAN_POINT('Ctrl Pts',(95.1078860688147,-0.561587259120174,
-8.80803140939792));
#38233=CARTESIAN_POINT('Ctrl Pts',(95.0876059028056,-0.51000646556631,-8.81103083311956));
#38234=CARTESIAN_POINT('Ctrl Pts',(95.0703142258555,-0.457458992978983,
-8.81403025684121));
#38235=CARTESIAN_POINT('Ctrl Pts',(95.0530066517137,-0.404863210603937,
-8.8170324380984));
#38236=CARTESIAN_POINT('Ctrl Pts',(95.0386932211769,-0.351299476376848,
-8.82003461935559));
#38237=CARTESIAN_POINT('Ctrl Pts',(95.0274630331812,-0.297139531682706,
-8.82303680061277));
#38238=CARTESIAN_POINT('Ctrl Pts',(95.0162277334534,-0.24295493458509,-8.82604034839616));
#38239=CARTESIAN_POINT('Ctrl Pts',(95.0080785517375,-0.188174109318222,
-8.82904389617956));
#38240=CARTESIAN_POINT('Ctrl Pts',(95.0030530043974,-0.133176704454972,
-8.83204744396295));
#38241=CARTESIAN_POINT('Ctrl Pts',(94.9980179721828,-0.0780755012498627,
-8.83505666043708));
#38242=CARTESIAN_POINT('Ctrl Pts',(94.9961183693583,-0.0227574309915909,
-8.83806587691121));
#38243=CARTESIAN_POINT('Ctrl Pts',(94.997339557011,0.0323962244713164,-8.84107509338534));
#38244=CARTESIAN_POINT('Ctrl Pts',(94.9982738155799,0.0745910297559468,
-8.84337726723256));
#38245=CARTESIAN_POINT('Ctrl Pts',(95.0010335501691,0.116689555092574,-8.84567944107978));
#38246=CARTESIAN_POINT('Ctrl Pts',(95.0055918355963,0.158524181184871,-8.847981614927));
#38247=CARTESIAN_POINT('Ctrl Pts',(95.0115518657483,0.213223615191785,-8.85099174357379));
#38248=CARTESIAN_POINT('Ctrl Pts',(95.0206135077032,0.267701392552597,-8.85400187222059));
#38249=CARTESIAN_POINT('Ctrl Pts',(95.0327487126871,0.321578776888731,-8.85701200086738));
#38250=CARTESIAN_POINT('Ctrl Pts',(95.0448623499927,0.375360405933311,-8.86001677966749));
#38251=CARTESIAN_POINT('Ctrl Pts',(95.0600385946801,0.428543248514046,-8.86302155846759));
#38252=CARTESIAN_POINT('Ctrl Pts',(95.0781978373417,0.480755288716801,-8.8660263372677));
#38253=CARTESIAN_POINT('Ctrl Pts',(95.0963391144416,0.532915673756977,-8.86902814333706));
#38254=CARTESIAN_POINT('Ctrl Pts',(95.1174573707341,0.584106662664619,-8.87202994940641));
#38255=CARTESIAN_POINT('Ctrl Pts',(95.1414227661909,0.633969840640893,-8.87503175547577));
#38256=CARTESIAN_POINT('Ctrl Pts',(95.1653739176115,0.68380338201401,-8.8780317773962));
#38257=CARTESIAN_POINT('Ctrl Pts',(95.1921686257863,0.732310201650655,-8.88103179931664));
#38258=CARTESIAN_POINT('Ctrl Pts',(95.2216292352011,0.779152539486286,-8.88403182123707));
#38259=CARTESIAN_POINT('Ctrl Pts',(95.2510839699935,0.825985536678473,-8.88703124493512));
#38260=CARTESIAN_POINT('Ctrl Pts',(95.2832032692917,0.871154264424761,-8.89003066863317));
#38261=CARTESIAN_POINT('Ctrl Pts',(95.317765086957,0.91434824181847,-8.89303009233122));
#38262=CARTESIAN_POINT('Ctrl Pts',(95.3523586792113,0.957581929822697,-8.89603227356523));
#38263=CARTESIAN_POINT('Ctrl Pts',(95.3893989454749,0.998836827102428,-8.89903445479925));
#38264=CARTESIAN_POINT('Ctrl Pts',(95.4286232256451,1.03783519287118,-8.90203663603327));
#38265=CARTESIAN_POINT('Ctrl Pts',(95.4678653598388,1.0768513098323,-8.90504018379369));
#38266=CARTESIAN_POINT('Ctrl Pts',(95.5092930939115,1.11360849667038,-8.90804373155411));
#38267=CARTESIAN_POINT('Ctrl Pts',(95.5526089607629,1.14786789393499,-8.91104727931453));
#38268=CARTESIAN_POINT('Ctrl Pts',(95.5960065790295,1.18219195005124,-8.91405649576631));
#38269=CARTESIAN_POINT('Ctrl Pts',(95.6412990155778,1.21400849501656,-8.91706571221808));
#38270=CARTESIAN_POINT('Ctrl Pts',(95.688158937957,1.24312145841316,-8.92007492866986));
#38271=CARTESIAN_POINT('Ctrl Pts',(95.7240087009461,1.26539406973398,-8.92237710270476));
#38272=CARTESIAN_POINT('Ctrl Pts',(95.7607752599711,1.28608518851768,-8.92467927673965));
#38273=CARTESIAN_POINT('Ctrl Pts',(95.7983035175063,1.30512577878773,-8.92698145077455));
#38274=CARTESIAN_POINT('Ctrl Pts',(95.8473723027826,1.33002164917598,-8.92999157942976));
#38275=CARTESIAN_POINT('Ctrl Pts',(95.8979501531717,1.35219872387525,-8.93300170808497));
#38276=CARTESIAN_POINT('Ctrl Pts',(95.949704541023,1.3714735544168,-8.93601183674018));
#38277=CARTESIAN_POINT('Ctrl Pts',(96.0013669467394,1.39071412815159,-8.93901661554832));
#38278=CARTESIAN_POINT('Ctrl Pts',(96.0542012493329,1.40706251119737,-8.94202139435647));
#38279=CARTESIAN_POINT('Ctrl Pts',(96.1078523771949,1.42038211053918,-8.94502617316461));
#38280=CARTESIAN_POINT('Ctrl Pts',(96.1614504261514,1.4336885323434,-8.94802797924176));
#38281=CARTESIAN_POINT('Ctrl Pts',(96.2158631895059,1.44397197970279,-8.95102978531892));
#38282=CARTESIAN_POINT('Ctrl Pts',(96.2707195411358,1.45114536069492,-8.95403159139607));
#38283=CARTESIAN_POINT('Ctrl Pts',(96.3255432884229,1.45831447812658,-8.95703161332405));
#38284=CARTESIAN_POINT('Ctrl Pts',(96.3808095788004,1.46237712468836,-8.96003163525204));
#38285=CARTESIAN_POINT('Ctrl Pts',(96.4361384588475,1.46329754087987,-8.96303165718002));
#38286=CARTESIAN_POINT('Ctrl Pts',(96.4914563059789,1.46421777353478,-8.96603108088536));
#38287=CARTESIAN_POINT('Ctrl Pts',(96.5468361902465,1.46199701140092,-8.9690305045907));
#38288=CARTESIAN_POINT('Ctrl Pts',(96.6018967503953,1.45665157854544,-8.97202992829604));
#38289=CARTESIAN_POINT('Ctrl Pts',(96.6570079307514,1.45130123133895,-8.97503210953689));
#38290=CARTESIAN_POINT('Ctrl Pts',(96.7117986736951,1.44282052530622,-8.97803429077774));
#38291=CARTESIAN_POINT('Ctrl Pts',(96.7658928473922,1.43127768887555,-8.98103647201859));
#38292=CARTESIAN_POINT('Ctrl Pts',(96.8200116435546,1.41972959840232,-8.98404001978561));
#38293=CARTESIAN_POINT('Ctrl Pts',(96.8734327281375,1.40511673864492,-8.98704356755263));
#38294=CARTESIAN_POINT('Ctrl Pts',(96.9257935150648,1.38755773443815,-8.99004711531964));
#38295=CARTESIAN_POINT('Ctrl Pts',(96.9782531241647,1.36996559056631,-8.99305633177754));
#38296=CARTESIAN_POINT('Ctrl Pts',(97.0296479464591,1.34941639112559,-8.99606554823543));
#38297=CARTESIAN_POINT('Ctrl Pts',(97.0796349145283,1.32607715374524,-8.99907476469333));
#38298=CARTESIAN_POINT('Ctrl Pts',(97.1178769947014,1.30822168017775,-9.00137693866959));
#38299=CARTESIAN_POINT('Ctrl Pts',(97.1552954661095,1.28873424402383,-9.00367911264585));
#38300=CARTESIAN_POINT('Ctrl Pts',(97.1917477645958,1.26770702264061,-9.00598128662211));
#38301=CARTESIAN_POINT('Ctrl Pts',(97.2394097189393,1.24021359953267,-9.0089914153521));
#38302=CARTESIAN_POINT('Ctrl Pts',(97.2856191558644,1.20997075436872,-9.01200154408208));
#38303=CARTESIAN_POINT('Ctrl Pts',(97.3300407405297,1.17715675250085,-9.01501167281207));
#38304=CARTESIAN_POINT('Ctrl Pts',(97.3743833755269,1.14440107035689,-9.01801645169545));
#38305=CARTESIAN_POINT('Ctrl Pts',(97.4169440427174,1.10908361129906,-9.02102123057883));
#38306=CARTESIAN_POINT('Ctrl Pts',(97.4574143320345,1.07142712348618,-9.02402600946221));
#38307=CARTESIAN_POINT('Ctrl Pts',(97.497844582707,1.03380789052766,-9.02702781561483));
#38308=CARTESIAN_POINT('Ctrl Pts',(97.5361881675456,0.993854570880955,-9.03002962176745));
#38309=CARTESIAN_POINT('Ctrl Pts',(97.5721693628588,0.951830405994109,-9.03303142792007));
#38310=CARTESIAN_POINT('Ctrl Pts',(97.6081291724419,0.909831218527945,-9.03603144992361));
#38311=CARTESIAN_POINT('Ctrl Pts',(97.6417290327405,0.865764025757706,-9.03903147192715));
#38312=CARTESIAN_POINT('Ctrl Pts',(97.6727313891479,0.819927510064312,-9.0420314939307));
#38313=CARTESIAN_POINT('Ctrl Pts',(97.7037275634962,0.774100134451781,-9.04503091771155));
#38314=CARTESIAN_POINT('Ctrl Pts',(97.7321269668841,0.726504573794474,-9.0480303414924));
#38315=CARTESIAN_POINT('Ctrl Pts',(97.7577348968595,0.677469147828813,-9.05102976527325));
#38316=CARTESIAN_POINT('Ctrl Pts',(97.78336636961,0.628388640905758,-9.05403194658895));
#38317=CARTESIAN_POINT('Ctrl Pts',(97.8062009967092,0.577866093130214,-9.05703412790464));
#38318=CARTESIAN_POINT('Ctrl Pts',(97.8260904043397,0.526253804796457,-9.06003630922034));
#38319=CARTESIAN_POINT('Ctrl Pts',(97.8459888651845,0.474618023701381,-9.06303985706194));
#38320=CARTESIAN_POINT('Ctrl Pts',(97.8629392722567,0.421892016905816,-9.06604340490354));
#38321=CARTESIAN_POINT('Ctrl Pts',(97.8768428614345,0.368444276165705,-9.06904695274514));
#38322=CARTESIAN_POINT('Ctrl Pts',(97.89077269129,0.314895661837429,-9.07205616927627));
#38323=CARTESIAN_POINT('Ctrl Pts',(97.9016441120435,0.26062311155624,-9.0750653858074));
#38324=CARTESIAN_POINT('Ctrl Pts',(97.9094095547582,0.206005211311661,-9.07807460233852));
#38325=CARTESIAN_POINT('Ctrl Pts',(97.9153504351482,0.164220290036205,-9.08037677571558));
#38326=CARTESIAN_POINT('Ctrl Pts',(97.9194744872999,0.122233465437668,-9.08267894909264));
#38327=CARTESIAN_POINT('Ctrl Pts',(97.9217810157308,0.0802145040429385,
-9.0849811224697));
#38328=CARTESIAN_POINT('Ctrl Pts',(97.9232383780006,0.0536651460853008,
-9.08643573303216));
#38329=CARTESIAN_POINT('Ctrl Pts',(97.923972265548,0.0270757141546565,-9.08789034359461));
#38330=CARTESIAN_POINT('Ctrl Pts',(97.923980872969,0.000473531057436198,
-9.08934495415708));
#38331=CARTESIAN_POINT('Origin',(96.460480949577,-8.32667268468867E-16,
1.18130019239114E-14));
#38332=CARTESIAN_POINT('',(97.9239806795947,0.000888953301123027,-9.66065504580791));
#38333=CARTESIAN_POINT('',(97.9239807107692,0.000836056531580603,-9.58934495412282));
#38334=CARTESIAN_POINT('',(97.923980949577,-1.01189432752408E-15,1.19922289829666E-14));
#38335=CARTESIAN_POINT('Ctrl Pts',(97.9239806795947,0.000888953301123711,
-9.66065504580791));
#38336=CARTESIAN_POINT('Ctrl Pts',(97.9239428755536,0.0631264227740048,
-9.65728431017794));
#38337=CARTESIAN_POINT('Ctrl Pts',(97.9199308592474,0.125216815453647,-9.65391357454797));
#38338=CARTESIAN_POINT('Ctrl Pts',(97.9120250762094,0.186686631655774,-9.650542838918));
#38339=CARTESIAN_POINT('Ctrl Pts',(97.9040582848518,0.248630805701209,-9.64714609158046));
#38340=CARTESIAN_POINT('Ctrl Pts',(97.8921375250518,0.30994452224196,-9.64374934424291));
#38341=CARTESIAN_POINT('Ctrl Pts',(97.8763950474731,0.370161474736446,-9.64035259690536));
#38342=CARTESIAN_POINT('Ctrl Pts',(97.8619494022101,0.425417880864817,-9.63723566649584));
#38343=CARTESIAN_POINT('Ctrl Pts',(97.8442864177926,0.479750852825148,-9.63411873608632));
#38344=CARTESIAN_POINT('Ctrl Pts',(97.8235433666888,0.532816194439787,-9.6310018056768));
#38345=CARTESIAN_POINT('Ctrl Pts',(97.8035109438714,0.58406359072966,-9.62799165699888));
#38346=CARTESIAN_POINT('Ctrl Pts',(97.7805422755616,0.634287334492359,-9.62498150832096));
#38347=CARTESIAN_POINT('Ctrl Pts',(97.7547633097597,0.683129140148358,-9.62197135964303));
#38348=CARTESIAN_POINT('Ctrl Pts',(97.7290301577865,0.731884145188208,-9.61896656053719));
#38349=CARTESIAN_POINT('Ctrl Pts',(97.7004968642633,0.779261622706428,-9.61596176143135));
#38350=CARTESIAN_POINT('Ctrl Pts',(97.6693373955263,0.824923234663004,-9.61295696232551));
#38351=CARTESIAN_POINT('Ctrl Pts',(97.6382087521334,0.870539674639368,-9.60995513579817));
#38352=CARTESIAN_POINT('Ctrl Pts',(97.6044593762844,0.914443177580305,-9.60695330927082));
#38353=CARTESIAN_POINT('Ctrl Pts',(97.5683081725724,0.956321647768353,-9.60395148274347));
#38354=CARTESIAN_POINT('Ctrl Pts',(97.5321784541071,0.998175228902307,-9.60095144025032));
#38355=CARTESIAN_POINT('Ctrl Pts',(97.493650081473,1.03800576375584,-9.59795139775717));
#38356=CARTESIAN_POINT('Ctrl Pts',(97.4529827248317,1.07553357740064,-9.59495135526402));
#38357=CARTESIAN_POINT('Ctrl Pts',(97.4123234764008,1.11305390879352,-9.59195191091586));
#38358=CARTESIAN_POINT('Ctrl Pts',(97.3695264788022,1.1482720728127,-9.5889524665677));
#38359=CARTESIAN_POINT('Ctrl Pts',(97.324887132431,1.18094631590257,-9.58595302221953));
#38360=CARTESIAN_POINT('Ctrl Pts',(97.2802067476131,1.21365059751875,-9.58295082038169));
#38361=CARTESIAN_POINT('Ctrl Pts',(97.2336810572276,1.24380597317031,-9.57994861854386));
#38362=CARTESIAN_POINT('Ctrl Pts',(97.1856361206834,1.27121289633863,-9.57694641670602));
#38363=CARTESIAN_POINT('Ctrl Pts',(97.1375693152027,1.29863229450026,-9.5739428483358));
#38364=CARTESIAN_POINT('Ctrl Pts',(97.0879823587091,1.32330051070059,-9.57093927996559));
#38365=CARTESIAN_POINT('Ctrl Pts',(97.0372247609889,1.34506461777794,-9.56793571159537));
#38366=CARTESIAN_POINT('Ctrl Pts',(96.9863713717002,1.36686979886287,-9.56492647478263));
#38367=CARTESIAN_POINT('Ctrl Pts',(96.9343434254315,1.38575974152273,-9.5619172379699));
#38368=CARTESIAN_POINT('Ctrl Pts',(96.8815080919921,1.40163062015273,-9.55890800115716));
#38369=CARTESIAN_POINT('Ctrl Pts',(96.8410900402114,1.4137715484391,-9.55660599071452));
#38370=CARTESIAN_POINT('Ctrl Pts',(96.8001998904651,1.42414674629186,-9.55430398027188));
#38371=CARTESIAN_POINT('Ctrl Pts',(96.7590053466449,1.432730063325,-9.55200196982924));
#38372=CARTESIAN_POINT('Ctrl Pts',(96.7051389254407,1.44395369946123,-9.54899183662664));
#38373=CARTESIAN_POINT('Ctrl Pts',(96.650525486727,1.45215886526455,-9.54598170342403));
#38374=CARTESIAN_POINT('Ctrl Pts',(96.5955339178958,1.45725527816793,-9.54297157022142));
#38375=CARTESIAN_POINT('Ctrl Pts',(96.5406400802778,1.46234263370801,-9.53996678663834));
#38376=CARTESIAN_POINT('Ctrl Pts',(96.4853699677669,1.46433215218327,-9.53696200305525));
#38377=CARTESIAN_POINT('Ctrl Pts',(96.4301019985479,1.46318466686005,-9.53395721947217));
#38378=CARTESIAN_POINT('Ctrl Pts',(96.3748887052482,1.46203831672989,-9.53095540848437));
#38379=CARTESIAN_POINT('Ctrl Pts',(96.3196780764452,1.45776112139514,-9.52795359749657));
#38380=CARTESIAN_POINT('Ctrl Pts',(96.2648511060458,1.45036588980848,-9.52495178650877));
#38381=CARTESIAN_POINT('Ctrl Pts',(96.2100567201579,1.44297505332166,-9.52195175954339));
#38382=CARTESIAN_POINT('Ctrl Pts',(96.1556460630646,1.43246992399667,-9.51895173257801));
#38383=CARTESIAN_POINT('Ctrl Pts',(96.1019952497374,1.4189151676582,-9.51595170561264));
#38384=CARTESIAN_POINT('Ctrl Pts',(96.0483551325816,1.40536311368317,-9.51295227675194));
#38385=CARTESIAN_POINT('Ctrl Pts',(95.9954750700827,1.38876276943336,-9.50995284789125));
#38386=CARTESIAN_POINT('Ctrl Pts',(95.9437189400153,1.36922944588326,-9.50695341903056));
#38387=CARTESIAN_POINT('Ctrl Pts',(95.8919152253086,1.34967816337534,-9.50395123249187));
#38388=CARTESIAN_POINT('Ctrl Pts',(95.8412380026789,1.32718870102126,-9.50094904595318));
#38389=CARTESIAN_POINT('Ctrl Pts',(95.7920325524046,1.30192510933525,-9.4979468594145));
#38390=CARTESIAN_POINT('Ctrl Pts',(95.7428047035116,1.27665001750948,-9.49494330626234));
#38391=CARTESIAN_POINT('Ctrl Pts',(95.6950504186494,1.24859854699928,-9.49193975311019));
#38392=CARTESIAN_POINT('Ctrl Pts',(95.6490887462701,1.21797986125091,-9.48893619995803));
#38393=CARTESIAN_POINT('Ctrl Pts',(95.6030403279506,1.18730338720749,-9.4859269780382));
#38394=CARTESIAN_POINT('Ctrl Pts',(95.558791703991,1.15405033685307,-9.48291775611838));
#38395=CARTESIAN_POINT('Ctrl Pts',(95.5166304482771,1.1184714932424,-9.47990853419856));
#38396=CARTESIAN_POINT('Ctrl Pts',(95.4843759858983,1.09125274813422,-9.47760640079293));
#38397=CARTESIAN_POINT('Ctrl Pts',(95.4533425452679,1.062673672895,-9.4753042673873));
#38398=CARTESIAN_POINT('Ctrl Pts',(95.423643678839,1.03286045718122,-9.47300213398168));
#38399=CARTESIAN_POINT('Ctrl Pts',(95.3848113592478,0.993878621850589,-9.46999201302764));
#38400=CARTESIAN_POINT('Ctrl Pts',(95.3480988934569,0.952621871770907,-9.4669818920736));
#38401=CARTESIAN_POINT('Ctrl Pts',(95.3137834545098,0.909349825318449,-9.46397177111957));
#38402=CARTESIAN_POINT('Ctrl Pts',(95.2795290061742,0.866154688520976,-9.4609670002098));
#38403=CARTESIAN_POINT('Ctrl Pts',(95.2476634554643,0.820951774086749,-9.45796222930003));
#38404=CARTESIAN_POINT('Ctrl Pts',(95.2184263725026,0.774036612550378,-9.45495745839026));
#38405=CARTESIAN_POINT('Ctrl Pts',(95.1892182159837,0.727167867708177,-9.45195566032611));
#38406=CARTESIAN_POINT('Ctrl Pts',(95.1626336536143,0.678590677608588,-9.44895386226196));
#38407=CARTESIAN_POINT('Ctrl Pts',(95.1388701321584,0.628631129743169,-9.44595206419781));
#38408=CARTESIAN_POINT('Ctrl Pts',(95.1151207355842,0.578701277506215,-9.44295205038279));
#38409=CARTESIAN_POINT('Ctrl Pts',(95.0941892827754,0.527391172060683,-9.43995203656777));
#38410=CARTESIAN_POINT('Ctrl Pts',(95.0762271233534,0.475051149441075,-9.43695202275275));
#38411=CARTESIAN_POINT('Ctrl Pts',(95.0582685462166,0.422721565259672,-9.43395260724582));
#38412=CARTESIAN_POINT('Ctrl Pts',(95.0432782577514,0.369362971065246,-9.43095319173889));
#38413=CARTESIAN_POINT('Ctrl Pts',(95.0313585046755,0.315343126576124,-9.42795377623196));
#38414=CARTESIAN_POINT('Ctrl Pts',(95.0194277933504,0.261273619739118,-9.42495160325659));
#38415=CARTESIAN_POINT('Ctrl Pts',(95.0105733711451,0.206542164902607,-9.42194943028122));
#38416=CARTESIAN_POINT('Ctrl Pts',(95.0048465025647,0.151527577263318,-9.41894725730585));
#38417=CARTESIAN_POINT('Ctrl Pts',(94.9991170273292,0.0964879490536366,
-9.4159437178543));
#38418=CARTESIAN_POINT('Ctrl Pts',(94.9965179682838,0.041165459602171,-9.41294017840274));
#38419=CARTESIAN_POINT('Ctrl Pts',(94.9970484736826,-0.0140583959776044,
-9.40993663895119));
#38420=CARTESIAN_POINT('Ctrl Pts',(94.9975799803276,-0.0693864779779125,
-9.40692743078704));
#38421=CARTESIAN_POINT('Ctrl Pts',(95.0012528155677,-0.124615025982781,
-9.40391822262288));
#38422=CARTESIAN_POINT('Ctrl Pts',(95.0080140725138,-0.179366164686339,
-9.40090901445873));
#38423=CARTESIAN_POINT('Ctrl Pts',(95.0131868711568,-0.221254325164286,
-9.39860677568386));
#38424=CARTESIAN_POINT('Ctrl Pts',(95.0201663132098,-0.262863105816736,
-9.39630453690899));
#38425=CARTESIAN_POINT('Ctrl Pts',(95.0289087496575,-0.304028430278557,
-9.39400229813412));
#38426=CARTESIAN_POINT('Ctrl Pts',(95.0403393128094,-0.357851279749002,
-9.39099216636315));
#38427=CARTESIAN_POINT('Ctrl Pts',(95.0548334808039,-0.411141685750961,
-9.38798203459218));
#38428=CARTESIAN_POINT('Ctrl Pts',(95.0723252594524,-0.463525651905658,
-9.3849719028212));
#38429=CARTESIAN_POINT('Ctrl Pts',(95.0897859506098,-0.515816517975453,
-9.38196712084606));
#38430=CARTESIAN_POINT('Ctrl Pts',(95.1102335139627,-0.567203644328016,
-9.37896233887091));
#38431=CARTESIAN_POINT('Ctrl Pts',(95.1335513319142,-0.617324906163024,
-9.37595755689577));
#38432=CARTESIAN_POINT('Ctrl Pts',(95.1568460809952,-0.66739658184479,-9.3729557476227));
#38433=CARTESIAN_POINT('Ctrl Pts',(95.1830052378704,-0.71620439737557,-9.36995393834964));
#38434=CARTESIAN_POINT('Ctrl Pts',(95.211863576753,-0.763404811539821,-9.36695212907658));
#38435=CARTESIAN_POINT('Ctrl Pts',(95.2407047636744,-0.810577172125566,
-9.36395210392964));
#38436=CARTESIAN_POINT('Ctrl Pts',(95.2722416779248,-0.856143575256737,
-9.36095207878271));
#38437=CARTESIAN_POINT('Ctrl Pts',(95.3062635977552,-0.899785838271265,
-9.35795205363577));
#38438=CARTESIAN_POINT('Ctrl Pts',(95.3402787336102,-0.943419399012564,
-9.35495262669426));
#38439=CARTESIAN_POINT('Ctrl Pts',(95.3767775664702,-0.985129165322661,
-9.35195319975275));
#38440=CARTESIAN_POINT('Ctrl Pts',(95.4155079522929,-1.02462855950198,-9.34895377281124));
#38441=CARTESIAN_POINT('Ctrl Pts',(95.4542739450643,-1.06416426762112,-9.34595158833353));
#38442=CARTESIAN_POINT('Ctrl Pts',(95.4952752190651,-1.10148516581086,-9.34294940385581));
#38443=CARTESIAN_POINT('Ctrl Pts',(95.5382225146415,-1.13634133480671,-9.3399472193781));
#38444=CARTESIAN_POINT('Ctrl Pts',(95.5811893589277,-1.171213369601,-9.33694366836886));
#38445=CARTESIAN_POINT('Ctrl Pts',(95.6261035615186,-1.20361812924814,-9.33394011735962));
#38446=CARTESIAN_POINT('Ctrl Pts',(95.672645142244,-1.2333478790203,-9.33093656635038));
#38447=CARTESIAN_POINT('Ctrl Pts',(95.7192745617813,-1.26313373831563,-9.3279273466821));
#38448=CARTESIAN_POINT('Ctrl Pts',(95.7675370334016,-1.29023424317224,-9.32491812701381));
#38449=CARTESIAN_POINT('Ctrl Pts',(95.8170871659795,-1.31448723433442,-9.32190890734553));
#38450=CARTESIAN_POINT('Ctrl Pts',(95.8549945867329,-1.33304154070413,-9.31960675899254));
#38451=CARTESIAN_POINT('Ctrl Pts',(95.893655098805,-1.34993021289996,-9.31730461063955));
#38452=CARTESIAN_POINT('Ctrl Pts',(95.9329074541082,-1.3651001636799,-9.31500246228656));
#38453=CARTESIAN_POINT('Ctrl Pts',(95.9842311014382,-1.38493533529771,-9.31199233335907));
#38454=CARTESIAN_POINT('Ctrl Pts',(96.0367827540384,-1.40191373683392,-9.30898220443158));
#38455=CARTESIAN_POINT('Ctrl Pts',(96.0902131217131,-1.41588628980189,-9.30597207550409));
#38456=CARTESIAN_POINT('Ctrl Pts',(96.1435485289823,-1.42983400971417,-9.30296729640061));
#38457=CARTESIAN_POINT('Ctrl Pts',(96.1977590452854,-1.44078635018952,-9.29996251729713));
#38458=CARTESIAN_POINT('Ctrl Pts',(96.2524776626869,-1.44864311776329,-9.29695773819365));
#38459=CARTESIAN_POINT('Ctrl Pts',(96.3071421453374,-1.45649211240387,-9.29395593180725));
#38460=CARTESIAN_POINT('Ctrl Pts',(96.3623132131176,-1.46125152620082,-9.29095412542086));
#38461=CARTESIAN_POINT('Ctrl Pts',(96.4176128629549,-1.46287203033942,-9.28795231903446));
#38462=CARTESIAN_POINT('Ctrl Pts',(96.4728796452205,-1.46449157132479,-9.2849522967839));
#38463=CARTESIAN_POINT('Ctrl Pts',(96.5282743312317,-1.46297588500209,-9.28195227453333));
#38464=CARTESIAN_POINT('Ctrl Pts',(96.5834152975203,-1.45832760245967,-9.27895225228277));
#38465=CARTESIAN_POINT('Ctrl Pts',(96.6385452686007,-1.45368024679317,-9.27595282824205));
#38466=CARTESIAN_POINT('Ctrl Pts',(96.6934210944778,-1.44590157976285,-9.27295340420133));
#38467=CARTESIAN_POINT('Ctrl Pts',(96.7476649886759,-1.43504619357248,-9.26995398016062));
#38468=CARTESIAN_POINT('Ctrl Pts',(96.8019587525819,-1.42418082736597,-9.26695179856713));
#38469=CARTESIAN_POINT('Ctrl Pts',(96.855618905139,-1.41023319464999,-9.26394961697364));
#38470=CARTESIAN_POINT('Ctrl Pts',(96.9082780824478,-1.39330900298271,-9.26094743538014));
#38471=CARTESIAN_POINT('Ctrl Pts',(96.9609612292185,-1.37637710774338,-9.25794388725036));
#38472=CARTESIAN_POINT('Ctrl Pts',(97.0126419988178,-1.35646614290013,-9.25494033912057));
#38473=CARTESIAN_POINT('Ctrl Pts',(97.0629715724583,-1.33373059473796,-9.25193679099078));
#38474=CARTESIAN_POINT('Ctrl Pts',(97.113396134891,-1.31095213696813,-9.24892757415791));
#38475=CARTESIAN_POINT('Ctrl Pts',(97.1624639377061,-1.28533869149056,-9.24591835732504));
#38476=CARTESIAN_POINT('Ctrl Pts',(97.2098504483552,-1.25709092920955,-9.24290914049218));
#38477=CARTESIAN_POINT('Ctrl Pts',(97.2461030261194,-1.23548026016615,-9.24060696914111));
#38478=CARTESIAN_POINT('Ctrl Pts',(97.2813720575643,-1.21232872965131,-9.23830479779005));
#38479=CARTESIAN_POINT('Ctrl Pts',(97.3155249713475,-1.18774238403558,-9.23600262643899));
#38480=CARTESIAN_POINT('Ctrl Pts',(97.3620994697563,-1.15421386222258,-9.23286314391614));
#38481=CARTESIAN_POINT('Ctrl Pts',(97.4068089063882,-1.11786234322615,-9.22972366139329));
#38482=CARTESIAN_POINT('Ctrl Pts',(97.4492910382359,-1.07892856972385,-9.22658417887044));
#38483=CARTESIAN_POINT('Ctrl Pts',(97.4896602430355,-1.04193123913399,-9.22360084429148));
#38484=CARTESIAN_POINT('Ctrl Pts',(97.5280179674677,-1.00260282258903,-9.22061750971251));
#38485=CARTESIAN_POINT('Ctrl Pts',(97.5640836833129,-0.961193662115265,
-9.21763417513355));
#38486=CARTESIAN_POINT('Ctrl Pts',(97.6001148729103,-0.919824143248592,
-9.21465369654529));
#38487=CARTESIAN_POINT('Ctrl Pts',(97.6338580477706,-0.876378227201588,
-9.21167321795702));
#38488=CARTESIAN_POINT('Ctrl Pts',(97.6650693991479,-0.831143138791571,
-9.20869273936876));
#38489=CARTESIAN_POINT('Ctrl Pts',(97.6962636541565,-0.78593282840995,-9.20571389337116));
#38490=CARTESIAN_POINT('Ctrl Pts',(97.7249285295215,-0.738935728421387,
-9.20273504737357));
#38491=CARTESIAN_POINT('Ctrl Pts',(97.7508619298017,-0.690470257052557,
-9.19975620137597));
#38492=CARTESIAN_POINT('Ctrl Pts',(97.7767917451654,-0.642011485332505,
-9.19677776716065));
#38493=CARTESIAN_POINT('Ctrl Pts',(97.7999905834695,-0.592085218786595,
-9.19379933294532));
#38494=CARTESIAN_POINT('Ctrl Pts',(97.8203021533147,-0.541034697469037,
-9.19082089873));
#38495=CARTESIAN_POINT('Ctrl Pts',(97.8406324961992,-0.489936992528979,
-9.18783971168645));
#38496=CARTESIAN_POINT('Ctrl Pts',(97.8580700469041,-0.437713458661016,
-9.18485852464291));
#38497=CARTESIAN_POINT('Ctrl Pts',(97.8725072188332,-0.384725960822175,
-9.18187733759937));
#38498=CARTESIAN_POINT('Ctrl Pts',(97.8869521583396,-0.331709954319111,
-9.17889454659897));
#38499=CARTESIAN_POINT('Ctrl Pts',(97.8983933956118,-0.277929690946204,
-9.17591175559857));
#38500=CARTESIAN_POINT('Ctrl Pts',(97.9067744264917,-0.223757521960541,
-9.17292896459817));
#38501=CARTESIAN_POINT('Ctrl Pts',(97.9151698002279,-0.169492645568799,
-9.16994106900585));
#38502=CARTESIAN_POINT('Ctrl Pts',(97.9204944698832,-0.114835059200487,
-9.16695317341352));
#38503=CARTESIAN_POINT('Ctrl Pts',(97.9227438919018,-0.0601609300440481,
-9.16396527782119));
#38504=CARTESIAN_POINT('Ctrl Pts',(97.9235745889996,-0.039970125455074,
-9.16286186717766));
#38505=CARTESIAN_POINT('Ctrl Pts',(97.9239864032088,-0.0197770426895552,
-9.16175845653414));
#38506=CARTESIAN_POINT('Ctrl Pts',(97.9239808950412,0.000399532766103907,
-9.16065504589061));
#38507=CARTESIAN_POINT('Ctrl Pts',(97.9239808729693,0.000473530088800385,
-9.08934495421004));
#38508=CARTESIAN_POINT('Ctrl Pts',(97.9239992748646,-0.0563996718694793,
-9.09245478771451));
#38509=CARTESIAN_POINT('Ctrl Pts',(97.920697403407,-0.113405113933069,-9.09556462121898));
#38510=CARTESIAN_POINT('Ctrl Pts',(97.9140598623374,-0.170119353332748,
-9.09867445472345));
#38511=CARTESIAN_POINT('Ctrl Pts',(97.9077000961744,-0.224460154678947,
-9.10165414459454));
#38512=CARTESIAN_POINT('Ctrl Pts',(97.8982783612853,-0.278533039653128,
-9.10463383446563));
#38513=CARTESIAN_POINT('Ctrl Pts',(97.885834129519,-0.331964700577071,-9.10761352433672));
#38514=CARTESIAN_POINT('Ctrl Pts',(97.8734012327862,-0.385347692392875,
-9.11059050010824));
#38515=CARTESIAN_POINT('Ctrl Pts',(97.8579514115358,-0.438090095080488,
-9.11356747587975));
#38516=CARTESIAN_POINT('Ctrl Pts',(97.8395755182899,-0.489826929176552,
-9.11654445165126));
#38517=CARTESIAN_POINT('Ctrl Pts',(97.8212087994914,-0.541537932862495,
-9.11951994112183));
#38518=CARTESIAN_POINT('Ctrl Pts',(97.7999190831797,-0.592243856755905,
-9.1224954305924));
#38519=CARTESIAN_POINT('Ctrl Pts',(97.775846883691,-0.641595440579602,-9.12547092006297));
#38520=CARTESIAN_POINT('Ctrl Pts',(97.7517767951269,-0.690942696694307,
-9.12844614860874));
#38521=CARTESIAN_POINT('Ctrl Pts',(97.7249249455963,-0.738935366394723,
-9.1314213771545));
#38522=CARTESIAN_POINT('Ctrl Pts',(97.6954787067503,-0.785246961010896,
-9.13439660570027));
#38523=CARTESIAN_POINT('Ctrl Pts',(97.6660034720907,-0.83160415881513,-9.13737476396391));
#38524=CARTESIAN_POINT('Ctrl Pts',(97.6339290411011,-0.876276524932001,
-9.14035292222756));
#38525=CARTESIAN_POINT('Ctrl Pts',(97.5994862869263,-0.918966316841838,
-9.1433310804912));
#38526=CARTESIAN_POINT('Ctrl Pts',(97.5650233597422,-0.961681112024216,
-9.14631098305248));
#38527=CARTESIAN_POINT('Ctrl Pts',(97.5281897118012,-1.00241062525302,-9.14929088561375));
#38528=CARTESIAN_POINT('Ctrl Pts',(97.4892544620633,-1.04089255449666,-9.15227078817503));
#38529=CARTESIAN_POINT('Ctrl Pts',(97.4502516700871,-1.07944123958886,-9.15525586006975));
#38530=CARTESIAN_POINT('Ctrl Pts',(97.4091404096045,-1.11573421150836,-9.15824093196448));
#38531=CARTESIAN_POINT('Ctrl Pts',(97.3662230882605,-1.14954922826867,-9.1612260038592));
#38532=CARTESIAN_POINT('Ctrl Pts',(97.353020138166,-1.15995197393756,-9.16214432201188));
#38533=CARTESIAN_POINT('Ctrl Pts',(97.3396464633258,-1.17012051846723,-9.16306264016456));
#38534=CARTESIAN_POINT('Ctrl Pts',(97.3261113723403,-1.18004924523795,-9.16398095831724));
#38535=CARTESIAN_POINT('Ctrl Pts',(97.2817450868536,-1.21259433318003,-9.16699108698006));
#38536=CARTESIAN_POINT('Ctrl Pts',(97.2354476357177,-1.2427022656766,-9.17000121564287));
#38537=CARTESIAN_POINT('Ctrl Pts',(97.1875172822922,-1.27013795349643,-9.17301134430569));
#38538=CARTESIAN_POINT('Ctrl Pts',(97.1396721146441,-1.29752488034895,-9.17601612311956));
#38539=CARTESIAN_POINT('Ctrl Pts',(97.0902002586328,-1.32224872737416,-9.17902090193344));
#38540=CARTESIAN_POINT('Ctrl Pts',(97.039429842127,-1.3441169702876,-9.18202568074732));
#38541=CARTESIAN_POINT('Ctrl Pts',(96.9887096545592,-1.36596357818815,-9.18502748682906));
#38542=CARTESIAN_POINT('Ctrl Pts',(96.9366939340987,-1.38495997056865,-9.18802929291081));
#38543=CARTESIAN_POINT('Ctrl Pts',(96.8837347003823,-1.40095985396772,-9.19103109899255));
#38544=CARTESIAN_POINT('Ctrl Pts',(96.8308069434604,-1.4169502276929,-9.19403112092399));
#38545=CARTESIAN_POINT('Ctrl Pts',(96.7769372893349,-1.42994747006969,-9.19703114285542));
#38546=CARTESIAN_POINT('Ctrl Pts',(96.7224948162786,-1.43985450086322,-9.20003116478686));
#38547=CARTESIAN_POINT('Ctrl Pts',(96.6680631994037,-1.44975955613073,-9.20303058849452));
#38548=CARTESIAN_POINT('Ctrl Pts',(96.6130595097337,-1.45657552908113,-9.20603001220218));
#38549=CARTESIAN_POINT('Ctrl Pts',(96.5578626856738,-1.46025650057611,-9.20902943590984));
#38550=CARTESIAN_POINT('Ctrl Pts',(96.5026151161637,-1.4639408561889,-9.21203161715126));
#38551=CARTESIAN_POINT('Ctrl Pts',(96.4471745856018,-1.46448441691308,-9.21503379839268));
#38552=CARTESIAN_POINT('Ctrl Pts',(96.3919233144981,-1.46189332739171,-9.2180359796341));
#38553=CARTESIAN_POINT('Ctrl Pts',(96.3366468942619,-1.45930105846482,-9.22103952740072));
#38554=CARTESIAN_POINT('Ctrl Pts',(96.2815604314095,-1.45357134975233,-9.22404307516733));
#38555=CARTESIAN_POINT('Ctrl Pts',(96.2270409776931,-1.4447622743991,-9.22704662293395));
#38556=CARTESIAN_POINT('Ctrl Pts',(96.1724186277122,-1.43593657340336,-9.23005583938989));
#38557=CARTESIAN_POINT('Ctrl Pts',(96.1183659416231,-1.42402000980274,-9.23306505584582));
#38558=CARTESIAN_POINT('Ctrl Pts',(96.0652485831776,-1.40912157976177,-9.23607427230176));
#38559=CARTESIAN_POINT('Ctrl Pts',(96.0246116263725,-1.39772367000578,-9.23837644625611));
#38560=CARTESIAN_POINT('Ctrl Pts',(95.9845218841768,-1.38458157294644,-9.24067862021046));
#38561=CARTESIAN_POINT('Ctrl Pts',(95.9451350145213,-1.36976305148794,-9.24298079416481));
#38562=CARTESIAN_POINT('Ctrl Pts',(95.8936360546815,-1.35038759849686,-9.24599092330318));
#38563=CARTESIAN_POINT('Ctrl Pts',(95.8431230973883,-1.32806308925686,-9.24900105244154));
#38564=CARTESIAN_POINT('Ctrl Pts',(95.7939560062024,-1.30291087563944,-9.25201118157991));
#38565=CARTESIAN_POINT('Ctrl Pts',(95.7448762987437,-1.27780336456836,-9.25501596087356));
#38566=CARTESIAN_POINT('Ctrl Pts',(95.6971381768513,-1.24987836108153,-9.2580207401672));
#38567=CARTESIAN_POINT('Ctrl Pts',(95.6510821726361,-1.2193054866958,-9.26102551946084));
#38568=CARTESIAN_POINT('Ctrl Pts',(95.6050717331857,-1.18876285909018,-9.26402732602457));
#38569=CARTESIAN_POINT('Ctrl Pts',(95.5607405525931,-1.15557784058576,-9.26702913258829));
#38570=CARTESIAN_POINT('Ctrl Pts',(95.51840349777,-1.1199653230332,-9.27003093915201));
#38571=CARTESIAN_POINT('Ctrl Pts',(95.4760916063315,-1.08437397207996,-9.27303096156675));
#38572=CARTESIAN_POINT('Ctrl Pts',(95.4357718948095,-1.04635832108944,-9.2760309839815));
#38573=CARTESIAN_POINT('Ctrl Pts',(95.3977273334798,-1.00617443888841,-9.27903100639624));
#38574=CARTESIAN_POINT('Ctrl Pts',(95.3596903584748,-0.965998569606039,
-9.28203043058766));
#38575=CARTESIAN_POINT('Ctrl Pts',(95.3239279955571,-0.923655711047762,
-9.28502985477908));
#38576=CARTESIAN_POINT('Ctrl Pts',(95.2906857537411,-0.87943814438493,-9.2880292789705));
#38577=CARTESIAN_POINT('Ctrl Pts',(95.2574129505596,-0.835179926155239,
-9.29103146069252));
#38578=CARTESIAN_POINT('Ctrl Pts',(95.2266652153427,-0.789043979490932,
-9.29403364241454));
#38579=CARTESIAN_POINT('Ctrl Pts',(95.198646245614,-0.741353781857565,-9.29703582413656));
#38580=CARTESIAN_POINT('Ctrl Pts',(95.1706145222937,-0.693641876741469,
-9.30003937238275));
#38581=CARTESIAN_POINT('Ctrl Pts',(95.1453142821186,-0.644374780994861,
-9.30304292062894));
#38582=CARTESIAN_POINT('Ctrl Pts',(95.1229029069058,-0.593900016638946,
-9.30604646887513));
#38583=CARTESIAN_POINT('Ctrl Pts',(95.10044923407,-0.543329989831342,-9.30905568580296));
#38584=CARTESIAN_POINT('Ctrl Pts',(95.0808955049108,-0.491548236500181,
-9.31206490273079));
#38585=CARTESIAN_POINT('Ctrl Pts',(95.0643502294876,-0.438920565048586,
-9.31507411965861));
#38586=CARTESIAN_POINT('Ctrl Pts',(95.0516924385786,-0.398658312277413,
-9.31737628977653));
#38587=CARTESIAN_POINT('Ctrl Pts',(95.040794441548,-0.357901351132589,-9.31967845989445));
#38588=CARTESIAN_POINT('Ctrl Pts',(95.0316845359028,-0.316817073832236,
-9.32198063001236));
#38589=CARTESIAN_POINT('Ctrl Pts',(95.0197731751921,-0.263098663837841,
-9.32499075764263));
#38590=CARTESIAN_POINT('Ctrl Pts',(95.0108704732858,-0.208594704812133,
-9.32800088527289));
#38591=CARTESIAN_POINT('Ctrl Pts',(95.0050714228735,-0.153672898003324,
-9.33101101290315));
#38592=CARTESIAN_POINT('Ctrl Pts',(94.9992826790039,-0.0988487026837372,
-9.33401579069047));
#38593=CARTESIAN_POINT('Ctrl Pts',(94.9965866949739,-0.0436086542901982,
-9.33702056847778));
#38594=CARTESIAN_POINT('Ctrl Pts',(94.9970274737238,0.0116693621642374,
-9.3400253462651));
#38595=CARTESIAN_POINT('Ctrl Pts',(94.9974678163966,0.0668926902181632,
-9.3430271513247));
#38596=CARTESIAN_POINT('Ctrl Pts',(95.0010387701615,0.122153386418911,-9.34602895638431));
#38597=CARTESIAN_POINT('Ctrl Pts',(95.007732399473,0.177070325494678,-9.34903076144392));
#38598=CARTESIAN_POINT('Ctrl Pts',(95.0144220503785,0.23195462429809,-9.3520307823594));
#38599=CARTESIAN_POINT('Ctrl Pts',(95.0242306343782,0.286495047751098,-9.35503080327488));
#38600=CARTESIAN_POINT('Ctrl Pts',(95.037098300903,0.340314685921306,-9.35803082419035));
#38601=CARTESIAN_POINT('Ctrl Pts',(95.0499634015649,0.394123592246064,-9.36103024688997));
#38602=CARTESIAN_POINT('Ctrl Pts',(95.0658862505955,0.447211485372616,-9.36402966958959));
#38603=CARTESIAN_POINT('Ctrl Pts',(95.0847561999249,0.499213043894782,-9.36702909228921));
#38604=CARTESIAN_POINT('Ctrl Pts',(95.1036434975602,0.551262410650516,-9.37003127254275));
#38605=CARTESIAN_POINT('Ctrl Pts',(95.1254831280923,0.602222949951803,-9.37303345279627));
#38606=CARTESIAN_POINT('Ctrl Pts',(95.1501154700795,0.651747313106343,-9.3760356330498));
#38607=CARTESIAN_POINT('Ctrl Pts',(95.1747590242363,0.701294218800918,-9.37903917983819));
#38608=CARTESIAN_POINT('Ctrl Pts',(95.2021975617758,0.749403185655384,-9.38204272662658));
#38609=CARTESIAN_POINT('Ctrl Pts',(95.2322260165785,0.795752517787265,-9.38504627341497));
#38610=CARTESIAN_POINT('Ctrl Pts',(95.2623111453174,0.842189326917629,-9.38805548892059));
#38611=CARTESIAN_POINT('Ctrl Pts',(95.2949956433555,0.886859439794644,-9.39106470442622));
#38612=CARTESIAN_POINT('Ctrl Pts',(95.3300324259056,0.929472100350025,-9.39407391993184));
#38613=CARTESIAN_POINT('Ctrl Pts',(95.3568371027837,0.962072656507588,-9.39637610190787));
#38614=CARTESIAN_POINT('Ctrl Pts',(95.3850176700251,0.99346963244608,-9.3986782838839));
#38615=CARTESIAN_POINT('Ctrl Pts',(95.4144493917181,1.02354786403143,-9.40098046585993));
#38616=CARTESIAN_POINT('Ctrl Pts',(95.4529317014846,1.06287549281125,-9.40399059489228));
#38617=CARTESIAN_POINT('Ctrl Pts',(95.4937158506339,1.10011250776548,-9.40700072392464));
#38618=CARTESIAN_POINT('Ctrl Pts',(95.5365457828554,1.13497843930852,-9.41001085295699));
#38619=CARTESIAN_POINT('Ctrl Pts',(95.5792995939972,1.16978240408632,-9.41301563212629));
#38620=CARTESIAN_POINT('Ctrl Pts',(95.624091566403,1.20222331764116,-9.41602041129558));
#38621=CARTESIAN_POINT('Ctrl Pts',(95.6706292539979,1.23205785131656,-9.41902519046488));
#38622=CARTESIAN_POINT('Ctrl Pts',(95.7171209001088,1.26186286856612,-9.42202699689317));
#38623=CARTESIAN_POINT('Ctrl Pts',(95.765354397691,1.28906633037508,-9.42502880332147));
#38624=CARTESIAN_POINT('Ctrl Pts',(95.8150062078859,1.31346663750505,-9.42803060974977));
#38625=CARTESIAN_POINT('Ctrl Pts',(95.8646285069314,1.33785244201956,-9.43103063201838));
#38626=CARTESIAN_POINT('Ctrl Pts',(95.915666974697,1.3594381616923,-9.43403065428699));
#38627=CARTESIAN_POINT('Ctrl Pts',(95.9677732366186,1.37806798075832,-9.4370306765556));
#38628=CARTESIAN_POINT('Ctrl Pts',(96.019869108044,1.39669408485694,-9.44003010059054));
#38629=CARTESIAN_POINT('Ctrl Pts',(96.0730318537501,1.41236528124424,-9.44302952462549));
#38630=CARTESIAN_POINT('Ctrl Pts',(96.1268950493132,1.42497463035143,-9.44602894866044));
#38631=CARTESIAN_POINT('Ctrl Pts',(96.180807763926,1.4375955718452,-9.44903113021146));
#38632=CARTESIAN_POINT('Ctrl Pts',(96.2354216996206,1.44714892160888,-9.45203331176249));
#38633=CARTESIAN_POINT('Ctrl Pts',(96.2903587257388,1.4535785768084,-9.45503549331352));
#38634=CARTESIAN_POINT('Ctrl Pts',(96.3453207577788,1.46001115862165,-9.4580390413804));
#38635=CARTESIAN_POINT('Ctrl Pts',(96.4006056453079,1.4633171799797,-9.46104258944727));
#38636=CARTESIAN_POINT('Ctrl Pts',(96.4558319117699,1.46349261578167,-9.46404613751415));
#38637=CARTESIAN_POINT('Ctrl Pts',(96.511162408129,1.46366838268796,-9.4670553542515));
#38638=CARTESIAN_POINT('Ctrl Pts',(96.5664335337557,1.46070178940326,-9.47006457098885));
#38639=CARTESIAN_POINT('Ctrl Pts',(96.6212667661651,1.45464090798523,-9.47307378772619));
#38640=CARTESIAN_POINT('Ctrl Pts',(96.6632163851004,1.45000409095428,-9.47537595905329));
#38641=CARTESIAN_POINT('Ctrl Pts',(96.7049097565665,1.44355731388188,-9.47767813038039));
#38642=CARTESIAN_POINT('Ctrl Pts',(96.7461822746122,1.43534212049711,-9.4799803017075));
#38643=CARTESIAN_POINT('Ctrl Pts',(96.8001468599256,1.42460060228424,-9.48299043355479));
#38644=CARTESIAN_POINT('Ctrl Pts',(96.8536182130661,1.41078892260863,-9.48600056540209));
#38645=CARTESIAN_POINT('Ctrl Pts',(96.9062215244966,1.39396828868893,-9.48901069724939));
#38646=CARTESIAN_POINT('Ctrl Pts',(96.9587313454702,1.37717754963149,-9.49201547926995));
#38647=CARTESIAN_POINT('Ctrl Pts',(97.0103756873712,1.35738862849228,-9.49502026129052));
#38648=CARTESIAN_POINT('Ctrl Pts',(97.0607909640459,1.33471350353864,-9.49802504331108));
#38649=CARTESIAN_POINT('Ctrl Pts',(97.1111563633747,1.31206081176646,-9.50102685261064));
#38650=CARTESIAN_POINT('Ctrl Pts',(97.1602946269448,1.28652778816772,-9.50402866191019));
#38651=CARTESIAN_POINT('Ctrl Pts',(97.2078601292047,1.25827525281991,-9.50703047120975));
#38652=CARTESIAN_POINT('Ctrl Pts',(97.2553973605972,1.23003950955129,-9.51003049636432));
#38653=CARTESIAN_POINT('Ctrl Pts',(97.3013632303254,1.1990877274236,-9.51303052151888));
#38654=CARTESIAN_POINT('Ctrl Pts',(97.3454368876451,1.16562654297076,-9.51603054667344));
#38655=CARTESIAN_POINT('Ctrl Pts',(97.3895017563951,1.13217203089258,-9.51902997360376));
#38656=CARTESIAN_POINT('Ctrl Pts',(97.4316747416874,1.09620942940807,-9.52202940053408));
#38657=CARTESIAN_POINT('Ctrl Pts',(97.4716660655663,1.05798719803303,-9.5250288274644));
#38658=CARTESIAN_POINT('Ctrl Pts',(97.5116941552569,1.01972982725206,-9.52803101190197));
#38659=CARTESIAN_POINT('Ctrl Pts',(97.5495361938056,0.979209041925372,-9.53103319633955));
#38660=CARTESIAN_POINT('Ctrl Pts',(97.5849385841689,0.936710882827834,-9.53403538077712));
#38661=CARTESIAN_POINT('Ctrl Pts',(97.620357088769,0.894193379686126,-9.53703893173008));
#38662=CARTESIAN_POINT('Ctrl Pts',(97.6533334165546,0.84969713362517,-9.54004248268305));
#38663=CARTESIAN_POINT('Ctrl Pts',(97.6836557588033,0.803539442761955,-9.54304603363601));
#38664=CARTESIAN_POINT('Ctrl Pts',(97.7140353287283,0.757294638002065,-9.54605525322236));
#38665=CARTESIAN_POINT('Ctrl Pts',(97.7417506419836,0.709382582729455,-9.54906447280871));
#38666=CARTESIAN_POINT('Ctrl Pts',(97.7666351367122,0.660146566626753,-9.55207369239506));
#38667=CARTESIAN_POINT('Ctrl Pts',(97.7856725641079,0.622479453348951,-9.55437584078172));
#38668=CARTESIAN_POINT('Ctrl Pts',(97.803054121417,0.584038015309721,-9.55667798916839));
#38669=CARTESIAN_POINT('Ctrl Pts',(97.8187246641583,0.544982808720181,-9.55898013755506));
#38670=CARTESIAN_POINT('Ctrl Pts',(97.8417157589475,0.487682817804549,-9.56235774308225));
#38671=CARTESIAN_POINT('Ctrl Pts',(97.8611038616657,0.428859176734495,-9.56573534860944));
#38672=CARTESIAN_POINT('Ctrl Pts',(97.8767107744066,0.368951667923016,-9.56911295413663));
#38673=CARTESIAN_POINT('Ctrl Pts',(97.8922917856593,0.309143582595085,-9.57248495413433));
#38674=CARTESIAN_POINT('Ctrl Pts',(97.9041039701687,0.24825547473603,-9.57585695413203));
#38675=CARTESIAN_POINT('Ctrl Pts',(97.9120173549428,0.186746656992054,-9.57922895412973));
#38676=CARTESIAN_POINT('Ctrl Pts',(97.9199307397169,0.125237839248078,-9.58260095412743));
#38677=CARTESIAN_POINT('Ctrl Pts',(97.9239451362168,0.0631085786241471,
-9.58597295412512));
#38678=CARTESIAN_POINT('Ctrl Pts',(97.9239807107692,0.000836056531596055,
-9.58934495412282));
#38679=CARTESIAN_POINT('Origin',(96.460480949577,-8.32667268468867E-16,
1.18130019239114E-14));
#38680=CARTESIAN_POINT('',(97.9239803647431,-0.00130836102040465,-10.1606550458429));
#38681=CARTESIAN_POINT('',(97.9239804027775,-0.00126510151654843,-10.0893449541571));
#38682=CARTESIAN_POINT('',(97.923980949577,-1.01189432752408E-15,1.19922289829666E-14));
#38683=CARTESIAN_POINT('Ctrl Pts',(97.9239803647431,-0.00130836102040465,
-10.1606550458429));
#38684=CARTESIAN_POINT('Ctrl Pts',(97.9240294293408,0.0535740521494451,
-10.1576764399972));
#38685=CARTESIAN_POINT('Ctrl Pts',(97.9209869965176,0.108513542155505,-10.1546978341516));
#38686=CARTESIAN_POINT('Ctrl Pts',(97.9148604658852,0.163133296855682,-10.151719228306));
#38687=CARTESIAN_POINT('Ctrl Pts',(97.9087364944472,0.217730235614312,-10.1487418666932));
#38688=CARTESIAN_POINT('Ctrl Pts',(97.8995310384136,0.272007171166325,-10.1457645050805));
#38689=CARTESIAN_POINT('Ctrl Pts',(97.887303411852,0.325591632489809,-10.1427871434677));
#38690=CARTESIAN_POINT('Ctrl Pts',(97.8750758843932,0.379175659520625,-10.139809805986));
#38691=CARTESIAN_POINT('Ctrl Pts',(97.859826357819,0.432066701307455,-10.1368324685043));
#38692=CARTESIAN_POINT('Ctrl Pts',(97.8416648848964,0.483904109112112,-10.1338551310225));
#38693=CARTESIAN_POINT('Ctrl Pts',(97.8234839976644,0.535796930234749,-10.130874610817));
#38694=CARTESIAN_POINT('Ctrl Pts',(97.802385134747,0.586633364343026,-10.1278940906115));
#38695=CARTESIAN_POINT('Ctrl Pts',(97.7785271432923,0.636071129067042,-10.1249135704061));
#38696=CARTESIAN_POINT('Ctrl Pts',(97.754653594347,0.685541131524163,-10.1219311066415));
#38697=CARTESIAN_POINT('Ctrl Pts',(97.7280176005758,0.733610182794539,-10.118948642877));
#38698=CARTESIAN_POINT('Ctrl Pts',(97.6988231611858,0.779962061223371,-10.1159661791125));
#38699=CARTESIAN_POINT('Ctrl Pts',(97.6695774261019,0.826395381591766,-10.1129784750504));
#38700=CARTESIAN_POINT('Ctrl Pts',(97.6377645955694,0.87110507949753,-10.1099907709883));
#38701=CARTESIAN_POINT('Ctrl Pts',(97.6036299865693,0.913806614784328,-10.1070030669263));
#38702=CARTESIAN_POINT('Ctrl Pts',(97.5960047456357,0.923345598951333,-10.1063356515382));
#38703=CARTESIAN_POINT('Ctrl Pts',(97.5882637899108,0.932784517046882,-10.1056682361502));
#38704=CARTESIAN_POINT('Ctrl Pts',(97.5804100987424,0.94212045453311,-10.1050008207621));
#38705=CARTESIAN_POINT('Ctrl Pts',(97.5449812473275,0.984235879614959,-10.1019900376656));
#38706=CARTESIAN_POINT('Ctrl Pts',(97.5070992123615,1.02443828878907,-10.0989792545691));
#38707=CARTESIAN_POINT('Ctrl Pts',(97.4669984367473,1.06242872608957,-10.0959684714726));
#38708=CARTESIAN_POINT('Ctrl Pts',(97.42696889155,1.10035168153606,-10.0929630363857));
#38709=CARTESIAN_POINT('Ctrl Pts',(97.384728807109,1.13607010244594,-10.0899576012988));
#38710=CARTESIAN_POINT('Ctrl Pts',(97.3405516921868,1.16931934816897,-10.086952166212));
#38711=CARTESIAN_POINT('Ctrl Pts',(97.296418264805,1.20253571311719,-10.0839497032537));
#38712=CARTESIAN_POINT('Ctrl Pts',(97.2503520213352,1.23328742422046,-10.0809472402954));
#38713=CARTESIAN_POINT('Ctrl Pts',(97.2026606000705,1.26134912549753,-10.0779447773372));
#38714=CARTESIAN_POINT('Ctrl Pts',(97.1549975280862,1.28939414601698,-10.0749440991373));
#38715=CARTESIAN_POINT('Ctrl Pts',(97.1057116471631,1.31475205899299,-10.0719434209374));
#38716=CARTESIAN_POINT('Ctrl Pts',(97.0551387920655,1.33724130222144,-10.0689427427376));
#38717=CARTESIAN_POINT('Ctrl Pts',(97.0045760499692,1.35972604829932,-10.0659426645802));
#38718=CARTESIAN_POINT('Ctrl Pts',(96.9527273268401,1.3793430495183,-10.0629425864228));
#38719=CARTESIAN_POINT('Ctrl Pts',(96.8999501221443,1.39595812844189,-10.0599425082655));
#38720=CARTESIAN_POINT('Ctrl Pts',(96.8471245503528,1.41258843407401,-10.0569396807191));
#38721=CARTESIAN_POINT('Ctrl Pts',(96.7933693015709,1.42621116223602,-10.0539368531727));
#38722=CARTESIAN_POINT('Ctrl Pts',(96.7390573629085,1.43674195036386,-10.0509340256263));
#38723=CARTESIAN_POINT('Ctrl Pts',(96.6847207719484,1.4472775184375,-10.0479298350904));
#38724=CARTESIAN_POINT('Ctrl Pts',(96.6298275113632,1.45471827768085,-10.0449256445546));
#38725=CARTESIAN_POINT('Ctrl Pts',(96.5747578178983,1.45903154433572,-10.0419214540188));
#38726=CARTESIAN_POINT('Ctrl Pts',(96.519584466998,1.46335292983294,-10.0389116087086));
#38727=CARTESIAN_POINT('Ctrl Pts',(96.4642345488208,1.46453505141985,-10.0359017633985));
#38728=CARTESIAN_POINT('Ctrl Pts',(96.409089269428,1.46259739682917,-10.0328919180884));
#38729=CARTESIAN_POINT('Ctrl Pts',(96.3670048878966,1.46111866653769,-10.0305949403638));
#38730=CARTESIAN_POINT('Ctrl Pts',(96.3250397233806,1.45782404885631,-10.0282979626392));
#38731=CARTESIAN_POINT('Ctrl Pts',(96.2833598762869,1.45274236373714,-10.0260009849147));
#38732=CARTESIAN_POINT('Ctrl Pts',(96.2287299609898,1.44608178201755,-10.0229903285115));
#38733=CARTESIAN_POINT('Ctrl Pts',(96.1743619734304,1.43632147095853,-10.0199796721084));
#38734=CARTESIAN_POINT('Ctrl Pts',(96.1206343740473,1.42349448720419,-10.0169690157053));
#38735=CARTESIAN_POINT('Ctrl Pts',(96.0670019208968,1.41069021876177,-10.0139636908751));
#38736=CARTESIAN_POINT('Ctrl Pts',(96.014008114684,1.3948301767368,-10.0109583660449));
#38737=CARTESIAN_POINT('Ctrl Pts',(95.9620240141196,1.375998885717,-10.0079530412147));
#38738=CARTESIAN_POINT('Ctrl Pts',(95.9100911476214,1.35718615428754,-10.004950678348));
#38739=CARTESIAN_POINT('Ctrl Pts',(95.8591665093319,1.33540815386084,-10.0019483154814));
#38740=CARTESIAN_POINT('Ctrl Pts',(95.8096068943097,1.31079945612587,-9.99894595261475));
#38741=CARTESIAN_POINT('Ctrl Pts',(95.7600765691199,1.28620530218085,-9.99594536415061));
#38742=CARTESIAN_POINT('Ctrl Pts',(95.7119101400558,1.25878400119002,-9.99294477568647));
#38743=CARTESIAN_POINT('Ctrl Pts',(95.6654431201801,1.22871766481477,-9.98994418722233));
#38744=CARTESIAN_POINT('Ctrl Pts',(95.6189852290236,1.19865723514804,-9.98694418824143));
#38745=CARTESIAN_POINT('Ctrl Pts',(95.5742265269607,1.16595308872611,-9.98394418926053));
#38746=CARTESIAN_POINT('Ctrl Pts',(95.5314746688416,1.13083136689526,-9.98094419027963));
#38747=CARTESIAN_POINT('Ctrl Pts',(95.4886833860961,1.09567725674667,-9.97794142477946));
#38748=CARTESIAN_POINT('Ctrl Pts',(95.4479030533949,1.05810145297181,-9.97493865927928));
#38749=CARTESIAN_POINT('Ctrl Pts',(95.4094080591436,1.01837028088799,-9.97193589377911));
#38750=CARTESIAN_POINT('Ctrl Pts',(95.3708954707516,0.978620949668397,-9.9689317558647));
#38751=CARTESIAN_POINT('Ctrl Pts',(95.3346706487805,0.936714686469186,-9.96592761795029));
#38752=CARTESIAN_POINT('Ctrl Pts',(95.3009686515576,0.892952115592899,-9.96292348003587));
#38753=CARTESIAN_POINT('Ctrl Pts',(95.2672030338939,0.84910693257838,-9.95991367110507));
#38754=CARTESIAN_POINT('Ctrl Pts',(95.2359700532083,0.803398878601056,-9.95690386217427));
#38755=CARTESIAN_POINT('Ctrl Pts',(95.2074615959471,0.756157886574571,-9.95389405324347));
#38756=CARTESIAN_POINT('Ctrl Pts',(95.1856987455871,0.720094951603775,-9.951596418518));
#38757=CARTESIAN_POINT('Ctrl Pts',(95.1655227269374,0.683139315342153,-9.94929878379252));
#38758=CARTESIAN_POINT('Ctrl Pts',(95.1470001770739,0.645445977805055,-9.94700114906704));
#38759=CARTESIAN_POINT('Ctrl Pts',(95.1227375337846,0.596071566085913,-9.94399148289449));
#38760=CARTESIAN_POINT('Ctrl Pts',(95.1012116407638,0.545223123099354,-9.94098181672195));
#38761=CARTESIAN_POINT('Ctrl Pts',(95.0826017297944,0.493235345136,-9.9379721505494));
#38762=CARTESIAN_POINT('Ctrl Pts',(95.0640249644206,0.441340161159751,-9.93496784480966));
#38763=CARTESIAN_POINT('Ctrl Pts',(95.0483540511211,0.388310162559924,-9.93196353906993));
#38764=CARTESIAN_POINT('Ctrl Pts',(95.0357210892669,0.334502003654749,-9.92895923333019));
#38765=CARTESIAN_POINT('Ctrl Pts',(95.0231006533233,0.280747196940334,-9.92595790643783));
#38766=CARTESIAN_POINT('Ctrl Pts',(95.013512322027,0.226216270114416,-9.92295657954548));
#38767=CARTESIAN_POINT('Ctrl Pts',(95.0070384973276,0.17128131246392,-9.91995525265312));
#38768=CARTESIAN_POINT('Ctrl Pts',(95.0005685323207,0.116379107019746,-9.91695571515101));
#38769=CARTESIAN_POINT('Ctrl Pts',(94.9972094552371,0.0610738718124895,
-9.9139561776489));
#38770=CARTESIAN_POINT('Ctrl Pts',(94.9969922291307,0.00574587908985627,
-9.91095664014679));
#38771=CARTESIAN_POINT('Ctrl Pts',(94.9967750466643,-0.0495709984394848,
-9.9079577052409));
#38772=CARTESIAN_POINT('Ctrl Pts',(94.9996984637714,-0.104910096399853,
-9.90495877033501));
#38773=CARTESIAN_POINT('Ctrl Pts',(95.0057413464022,-0.159890390439509,
-9.90195983542912));
#38774=CARTESIAN_POINT('Ctrl Pts',(95.0117897796947,-0.214921186371307,
-9.89895814586558));
#38775=CARTESIAN_POINT('Ctrl Pts',(95.0209633453419,-0.26959199365133,-9.89595645630205));
#38776=CARTESIAN_POINT('Ctrl Pts',(95.0331890750857,-0.323527672712909,
-9.89295476673851));
#38777=CARTESIAN_POINT('Ctrl Pts',(95.0454203610206,-0.377487863762713,
-9.88995171300602));
#38778=CARTESIAN_POINT('Ctrl Pts',(95.0607064300513,-0.430711751943461,
-9.88694865927353));
#38779=CARTESIAN_POINT('Ctrl Pts',(95.0789240932648,-0.482838381631814,
-9.88394560554103));
#38780=CARTESIAN_POINT('Ctrl Pts',(95.0971761588704,-0.535063447696359,
-9.88093688081602));
#38781=CARTESIAN_POINT('Ctrl Pts',(95.1183706749341,-0.586186626761002,
-9.87792815609101));
#38782=CARTESIAN_POINT('Ctrl Pts',(95.1423363114514,-0.635867095375006,
-9.874919431366));
#38783=CARTESIAN_POINT('Ctrl Pts',(95.1607047920133,-0.673944728797587,
-9.87261339198383));
#38784=CARTESIAN_POINT('Ctrl Pts',(95.1807001516218,-0.711175248614454,
-9.87030735260166));
#38785=CARTESIAN_POINT('Ctrl Pts',(95.2022278909176,-0.74741654408645,-9.86800131321949));
#38786=CARTESIAN_POINT('Ctrl Pts',(95.2303296931089,-0.794725074839264,
-9.8649910639001));
#38787=CARTESIAN_POINT('Ctrl Pts',(95.2611623134059,-0.840545858886474,
-9.8619808145807));
#38788=CARTESIAN_POINT('Ctrl Pts',(95.294543180829,-0.884545854892223,-9.85897056526131));
#38789=CARTESIAN_POINT('Ctrl Pts',(95.3278647364916,-0.928467670867626,
-9.8559656646102));
#38790=CARTESIAN_POINT('Ctrl Pts',(95.3637252372699,-0.970574701818236,
-9.85296076395909));
#38791=CARTESIAN_POINT('Ctrl Pts',(95.4018979789767,-1.01056140058635,-9.84995586330798));
#38792=CARTESIAN_POINT('Ctrl Pts',(95.4400329645613,-1.05050854907286,-9.84695393476187));
#38793=CARTESIAN_POINT('Ctrl Pts',(95.4804752977666,-1.08833913973975,-9.84395200621574));
#38794=CARTESIAN_POINT('Ctrl Pts',(95.5229582040928,-1.12378082903198,-9.84095007766962));
#38795=CARTESIAN_POINT('Ctrl Pts',(95.5654158670453,-1.15920145884675,-9.83794993287162));
#38796=CARTESIAN_POINT('Ctrl Pts',(95.6099112951568,-1.19223566320698,-9.83494978807362));
#38797=CARTESIAN_POINT('Ctrl Pts',(95.6561427654742,-1.22264971909135,-9.83194964327562));
#38798=CARTESIAN_POINT('Ctrl Pts',(95.7023650200588,-1.25305771226978,-9.82895009652333));
#38799=CARTESIAN_POINT('Ctrl Pts',(95.75032218867,-1.28084630417462,-9.82595054977104));
#38800=CARTESIAN_POINT('Ctrl Pts',(95.799683462524,-1.30582500018356,-9.82295100301875));
#38801=CARTESIAN_POINT('Ctrl Pts',(95.8490901032074,-1.33082665354655,-9.81994869945094));
#38802=CARTESIAN_POINT('Ctrl Pts',(95.8999029551621,-1.3530130125462,-9.81694639588313));
#38803=CARTESIAN_POINT('Ctrl Pts',(95.9517678242792,-1.37224021444855,-9.81394409231532));
#38804=CARTESIAN_POINT('Ctrl Pts',(96.0036562965077,-1.39147616643153,-9.81094042243335));
#38805=CARTESIAN_POINT('Ctrl Pts',(96.0565972346435,-1.40775012135957,-9.80793675255138));
#38806=CARTESIAN_POINT('Ctrl Pts',(96.110220888847,-1.42096802914683,-9.80493308266941));
#38807=CARTESIAN_POINT('Ctrl Pts',(96.1639457109321,-1.43421087420756,-9.80192374598007));
#38808=CARTESIAN_POINT('Ctrl Pts',(96.2183553017883,-1.44438605707627,-9.79891440929072));
#38809=CARTESIAN_POINT('Ctrl Pts',(96.2730704726965,-1.45145084765397,-9.79590507260138));
#38810=CARTESIAN_POINT('Ctrl Pts',(96.3149104119537,-1.45685319591917,-9.79360387419156));
#38811=CARTESIAN_POINT('Ctrl Pts',(96.356928825872,-1.4604378223726,-9.79130267578174));
#38812=CARTESIAN_POINT('Ctrl Pts',(96.3989561765355,-1.46220619349741,-9.78900147737192));
#38813=CARTESIAN_POINT('Ctrl Pts',(96.4539318564525,-1.46451938724857,-9.78599129602081));
#38814=CARTESIAN_POINT('Ctrl Pts',(96.5091536315192,-1.46373268468115,-9.7829811146697));
#38815=CARTESIAN_POINT('Ctrl Pts',(96.5642428293329,-1.45981701672145,-9.77997093331859));
#38816=CARTESIAN_POINT('Ctrl Pts',(96.6192341581163,-1.45590830516413,-9.77696609972243));
#38817=CARTESIAN_POINT('Ctrl Pts',(96.6740928545523,-1.44888169680325,-9.77396126612626));
#38818=CARTESIAN_POINT('Ctrl Pts',(96.7284391581908,-1.43876010802235,-9.77095643253009));
#38819=CARTESIAN_POINT('Ctrl Pts',(96.7827317185529,-1.42864852852097,-9.76795457042585));
#38820=CARTESIAN_POINT('Ctrl Pts',(96.8365123732653,-1.41544812780354,-9.76495270832161));
#38821=CARTESIAN_POINT('Ctrl Pts',(96.889407276111,-1.39923352461482,-9.76195084621737));
#38822=CARTESIAN_POINT('Ctrl Pts',(96.9422707610342,-1.38302855239467,-9.75895076712559));
#38823=CARTESIAN_POINT('Ctrl Pts',(96.994249032978,-1.36381308075201,-9.75595068803382));
#38824=CARTESIAN_POINT('Ctrl Pts',(97.0449814957135,-1.34171210084955,-9.75295060894204));
#38825=CARTESIAN_POINT('Ctrl Pts',(97.0957038597974,-1.31961552030177,-9.749951127037));
#38826=CARTESIAN_POINT('Ctrl Pts',(97.1451804232903,-1.29463478298976,-9.74695164513195));
#38827=CARTESIAN_POINT('Ctrl Pts',(97.1930709028164,-1.26694285996356,-9.74395216322691));
#38828=CARTESIAN_POINT('Ctrl Pts',(97.2410054281509,-1.23922546813551,-9.74094992263984));
#38829=CARTESIAN_POINT('Ctrl Pts',(97.2873504969757,-1.20879217377013,-9.73794768205278));
#38830=CARTESIAN_POINT('Ctrl Pts',(97.3317921040487,-1.17586101308499,-9.73494544146571));
#38831=CARTESIAN_POINT('Ctrl Pts',(97.3762539503339,-1.14291485517552,-9.7319418336242));
#38832=CARTESIAN_POINT('Ctrl Pts',(97.4188102003654,-1.10746890187683,-9.7289382257827));
#38833=CARTESIAN_POINT('Ctrl Pts',(97.4591800696255,-1.0697814345063,-9.72593461794119));
#38834=CARTESIAN_POINT('Ctrl Pts',(97.4996261347469,-1.03202283415745,-9.72292534095855));
#38835=CARTESIAN_POINT('Ctrl Pts',(97.537877209595,-0.992014650837638,-9.71991606397592));
#38836=CARTESIAN_POINT('Ctrl Pts',(97.5736903348873,-0.950051111497216,
-9.71690678699328));
#38837=CARTESIAN_POINT('Ctrl Pts',(97.6010828327383,-0.917954327097042,
-9.71460507183697));
#38838=CARTESIAN_POINT('Ctrl Pts',(97.6270498305126,-0.884714358085679,
-9.71230335668067));
#38839=CARTESIAN_POINT('Ctrl Pts',(97.6514998639153,-0.850474100539441,
-9.71000164152436));
#38840=CARTESIAN_POINT('Ctrl Pts',(97.683736559021,-0.8053292647564,-9.70696689353479));
#38841=CARTESIAN_POINT('Ctrl Pts',(97.7134696579605,-0.758255660224419,
-9.70393214554522));
#38842=CARTESIAN_POINT('Ctrl Pts',(97.7404646736664,-0.709558958837252,
-9.70089739755565));
#38843=CARTESIAN_POINT('Ctrl Pts',(97.767415230793,-0.660942456927828,-9.6978676475474));
#38844=CARTESIAN_POINT('Ctrl Pts',(97.7916363977639,-0.610708606457505,
-9.69483789753914));
#38845=CARTESIAN_POINT('Ctrl Pts',(97.8129364109217,-0.55919269941482,-9.69180814753089));
#38846=CARTESIAN_POINT('Ctrl Pts',(97.8342065427992,-0.507749062809193,
-9.68878264788665));
#38847=CARTESIAN_POINT('Ctrl Pts',(97.8525634604831,-0.455027415355879,
-9.68575714824241));
#38848=CARTESIAN_POINT('Ctrl Pts',(97.8678619595953,-0.401386276097912,
-9.68273164859817));
#38849=CARTESIAN_POINT('Ctrl Pts',(97.8831479351127,-0.347789048330475,
-9.6797086256761));
#38850=CARTESIAN_POINT('Ctrl Pts',(97.8953803175433,-0.293274317348441,
-9.67668560275404));
#38851=CARTESIAN_POINT('Ctrl Pts',(97.9044632059323,-0.238217323742553,
-9.67366257983197));
#38852=CARTESIAN_POINT('Ctrl Pts',(97.9135431559158,-0.183178141626121,
-9.67064053488813));
#38853=CARTESIAN_POINT('Ctrl Pts',(97.9194755451615,-0.127597553509319,
-9.66761848994428));
#38854=CARTESIAN_POINT('Ctrl Pts',(97.9222156394325,-0.0718606044574211,
-9.66459644500044));
#38855=CARTESIAN_POINT('Ctrl Pts',(97.9234068642987,-0.0476295988393163,
-9.66328264528126));
#38856=CARTESIAN_POINT('Ctrl Pts',(97.923995414332,-0.0233691259645077,
-9.66196884556208));
#38857=CARTESIAN_POINT('Ctrl Pts',(97.9239806795951,0.000888952655002563,
-9.6606550458429));
#38858=CARTESIAN_POINT('Ctrl Pts',(97.9239807107695,0.000836055898965084,
-9.58934495415708));
#38859=CARTESIAN_POINT('Ctrl Pts',(97.9240126572801,-0.0550856961044943,
-9.59237306577497));
#38860=CARTESIAN_POINT('Ctrl Pts',(97.920835028295,-0.111014615602546,-9.59540117739287));
#38861=CARTESIAN_POINT('Ctrl Pts',(97.9144717574115,-0.166562242818737,
-9.59842928901076));
#38862=CARTESIAN_POINT('Ctrl Pts',(97.9081069032638,-0.222123691003714,
-9.60145815406203));
#38863=CARTESIAN_POINT('Ctrl Pts',(97.8985548953864,-0.277303148660256,
-9.6044870191133));
#38864=CARTESIAN_POINT('Ctrl Pts',(97.8858913123318,-0.331719079570828,
-9.60751588416457));
#38865=CARTESIAN_POINT('Ctrl Pts',(97.8732102931455,-0.386209934247392,
-9.610548919575));
#38866=CARTESIAN_POINT('Ctrl Pts',(97.8574092691731,-0.439934663777601,
-9.61358195498544));
#38867=CARTESIAN_POINT('Ctrl Pts',(97.8386142670535,-0.49252493262916,-9.61661499039588));
#38868=CARTESIAN_POINT('Ctrl Pts',(97.8198043156689,-0.545157030997792,
-9.61965043823754));
#38869=CARTESIAN_POINT('Ctrl Pts',(97.7979958479512,-0.596652400285083,
-9.62268588607919));
#38870=CARTESIAN_POINT('Ctrl Pts',(97.7733625727979,-0.646663817921657,
-9.62572133392085));
#38871=CARTESIAN_POINT('Ctrl Pts',(97.7486806606055,-0.696773980335626,
-9.62876277508634));
#38872=CARTESIAN_POINT('Ctrl Pts',(97.7211630645337,-0.745393897980012,
-9.63180421625184));
#38873=CARTESIAN_POINT('Ctrl Pts',(97.6910282055441,-0.792203067926339,
-9.63484565741733));
#38874=CARTESIAN_POINT('Ctrl Pts',(97.6806765153304,-0.808282586553376,
-9.63589042941243));
#38875=CARTESIAN_POINT('Ctrl Pts',(97.6700163442168,-0.824148714008224,
-9.63693520140752));
#38876=CARTESIAN_POINT('Ctrl Pts',(97.6590576291842,-0.839789374249164,
-9.63797997340262));
#38877=CARTESIAN_POINT('Ctrl Pts',(97.6274840396244,-0.884852302285955,
-9.64099010753408));
#38878=CARTESIAN_POINT('Ctrl Pts',(97.5932992289051,-0.928226826130445,
-9.64400024166554));
#38879=CARTESIAN_POINT('Ctrl Pts',(97.5567102281248,-0.969594564163086,
-9.64701037579701));
#38880=CARTESIAN_POINT('Ctrl Pts',(97.5201862576479,-1.0108887785548,-9.65001515996176));
#38881=CARTESIAN_POINT('Ctrl Pts',(97.4812669239856,-1.05018289288802,-9.65301994412652));
#38882=CARTESIAN_POINT('Ctrl Pts',(97.4402012041658,-1.08718925341837,-9.65602472829128));
#38883=CARTESIAN_POINT('Ctrl Pts',(97.3991761130537,-1.12415900140154,-9.65902653964811));
#38884=CARTESIAN_POINT('Ctrl Pts',(97.3560092328158,-1.1588451274842,-9.66202835100494));
#38885=CARTESIAN_POINT('Ctrl Pts',(97.3109870062691,-1.19099609467454,-9.66503016236177));
#38886=CARTESIAN_POINT('Ctrl Pts',(97.2659915403011,-1.22312795178188,-9.66803018948412));
#38887=CARTESIAN_POINT('Ctrl Pts',(97.2191433427515,-1.25272733040001,-9.67103021660648));
#38888=CARTESIAN_POINT('Ctrl Pts',(97.1707608078467,-1.27958382802237,-9.67403024372883));
#38889=CARTESIAN_POINT('Ctrl Pts',(97.1223879222096,-1.30643496946541,-9.67702967253478));
#38890=CARTESIAN_POINT('Ctrl Pts',(97.0724817684151,-1.33054406012878,-9.68002910134072));
#38891=CARTESIAN_POINT('Ctrl Pts',(97.021386499642,-1.35174598719816,-9.68302853014666));
#38892=CARTESIAN_POINT('Ctrl Pts',(96.970244259382,-1.3729674050357,-9.68603071630439));
#38893=CARTESIAN_POINT('Ctrl Pts',(96.9179112090179,-1.39127611706288,-9.68903290246212));
#38894=CARTESIAN_POINT('Ctrl Pts',(96.8647513203896,-1.40655526634507,-9.69203508861985));
#38895=CARTESIAN_POINT('Ctrl Pts',(96.8115672362733,-1.42184136986442,-9.69503864120932));
#38896=CARTESIAN_POINT('Ctrl Pts',(96.7575560796247,-1.4340950448615,-9.69804219379879));
#38897=CARTESIAN_POINT('Ctrl Pts',(96.7030935938257,-1.44325027450219,-9.70104574638826));
#38898=CARTESIAN_POINT('Ctrl Pts',(96.6485283232801,-1.45242278242067,-9.70405496745554));
#38899=CARTESIAN_POINT('Ctrl Pts',(96.5935105482571,-1.45848510557856,-9.70706418852281));
#38900=CARTESIAN_POINT('Ctrl Pts',(96.538421570746,-1.46142311107078,-9.71007340959008));
#38901=CARTESIAN_POINT('Ctrl Pts',(96.496277054823,-1.46367076250384,-9.71237554281011));
#38902=CARTESIAN_POINT('Ctrl Pts',(96.454090998094,-1.46409093678363,-9.71467767603014));
#38903=CARTESIAN_POINT('Ctrl Pts',(96.412032562978,-1.46269785117637,-9.71697980925017));
#38904=CARTESIAN_POINT('Ctrl Pts',(96.3570391548051,-1.46087632535857,-9.71998995814154));
#38905=CARTESIAN_POINT('Ctrl Pts',(96.302033080692,-1.45594525977901,-9.72300010703291));
#38906=CARTESIAN_POINT('Ctrl Pts',(96.2473941183345,-1.44790408948626,-9.72601025592429));
#38907=CARTESIAN_POINT('Ctrl Pts',(96.1928522608653,-1.43987721003852,-9.72901505515016));
#38908=CARTESIAN_POINT('Ctrl Pts',(96.1386767386452,-1.42875127113368,-9.73201985437604));
#38909=CARTESIAN_POINT('Ctrl Pts',(96.085244512539,-1.41457762824069,-9.73502465360192));
#38910=CARTESIAN_POINT('Ctrl Pts',(96.0318651467173,-1.40041800727509,-9.73802648019212));
#38911=CARTESIAN_POINT('Ctrl Pts',(95.9792281282806,-1.38321678979531,-9.74102830678232));
#38912=CARTESIAN_POINT('Ctrl Pts',(95.9277006400562,-1.363076443853,-9.74403013337251));
#38913=CARTESIAN_POINT('Ctrl Pts',(95.876203776431,-1.34294806802687,-9.74703017587155));
#38914=CARTESIAN_POINT('Ctrl Pts',(95.825815626866,-1.31988421793841,-9.7500302183706));
#38915=CARTESIAN_POINT('Ctrl Pts',(95.7768863807261,-1.29403659741045,-9.75303026086964));
#38916=CARTESIAN_POINT('Ctrl Pts',(95.727966890969,-1.26819413084046,-9.75602970516689));
#38917=CARTESIAN_POINT('Ctrl Pts',(95.6805061936124,-1.23956924273064,-9.75902914946414));
#38918=CARTESIAN_POINT('Ctrl Pts',(95.6348306210236,-1.20835995670149,-9.76202859376139));
#38919=CARTESIAN_POINT('Ctrl Pts',(95.5891130586785,-1.17712197983742,-9.76503079546107));
#38920=CARTESIAN_POINT('Ctrl Pts',(95.5451843367288,-1.14329515699568,-9.76803299716075));
#38921=CARTESIAN_POINT('Ctrl Pts',(95.503341200612,-1.10712047716194,-9.77103519886043));
#38922=CARTESIAN_POINT('Ctrl Pts',(95.4614790191512,-1.07092933204171,-9.77403876704383));
#38923=CARTESIAN_POINT('Ctrl Pts',(95.4217046957669,-1.03238856778564,-9.77704233522723));
#38924=CARTESIAN_POINT('Ctrl Pts',(95.3842788277877,-0.991776811110299,
-9.78004590341063));
#38925=CARTESIAN_POINT('Ctrl Pts',(95.346782329318,-0.951088411501984,-9.7830551399594));
#38926=CARTESIAN_POINT('Ctrl Pts',(95.3116434760072,-0.908321620881624,
-9.78606437650817));
#38927=CARTESIAN_POINT('Ctrl Pts',(95.2790824481551,-0.863788070557825,
-9.78907361305693));
#38928=CARTESIAN_POINT('Ctrl Pts',(95.2541738599928,-0.829720722639403,
-9.7913756237372));
#38929=CARTESIAN_POINT('Ctrl Pts',(95.230772976813,-0.79462017121957,-9.79367763441747));
#38930=CARTESIAN_POINT('Ctrl Pts',(95.2089603081028,-0.758635837516282,
-9.79597964509773));
#38931=CARTESIAN_POINT('Ctrl Pts',(95.1804384897308,-0.711583427572393,
-9.79898970917496));
#38932=CARTESIAN_POINT('Ctrl Pts',(95.1545139061549,-0.662821427610296,
-9.80199977325219));
#38933=CARTESIAN_POINT('Ctrl Pts',(95.131394539733,-0.612667581293462,-9.80500983732941));
#38934=CARTESIAN_POINT('Ctrl Pts',(95.1083162632534,-0.562602873174066,
-9.80801455163378));
#38935=CARTESIAN_POINT('Ctrl Pts',(95.0880335290975,-0.51115170356423,-9.81101926593814));
#38936=CARTESIAN_POINT('Ctrl Pts',(95.0707092966997,-0.458657827643519,
-9.8140239802425));
#38937=CARTESIAN_POINT('Ctrl Pts',(95.0534022035883,-0.406215885197136,
-9.81702572190957));
#38938=CARTESIAN_POINT('Ctrl Pts',(95.0390479788662,-0.352733779004543,
-9.82002746357664));
#38939=CARTESIAN_POINT('Ctrl Pts',(95.0277614316403,-0.298575003848839,
-9.82302920524371));
#38940=CARTESIAN_POINT('Ctrl Pts',(95.0164815920401,-0.244448415399853,
-9.82602916296758));
#38941=CARTESIAN_POINT('Ctrl Pts',(95.0082659239144,-0.18964647106752,-9.82902912069145));
#38942=CARTESIAN_POINT('Ctrl Pts',(95.0031787151428,-0.134545336274049,
-9.83202907841532));
#38943=CARTESIAN_POINT('Ctrl Pts',(94.9980925202735,-0.0794551833708021,
-9.83502843823487));
#38944=CARTESIAN_POINT('Ctrl Pts',(94.9961335950115,-0.0240664840386528,
-9.83802779805443));
#38945=CARTESIAN_POINT('Ctrl Pts',(94.9973143978304,0.0312392677565819,
-9.84102715787398));
#38946=CARTESIAN_POINT('Ctrl Pts',(94.9984962866418,0.0865958846348152,
-9.84402927622553));
#38947=CARTESIAN_POINT('Ctrl Pts',(95.0028236613408,0.141868872408044,-9.84703139457709));
#38948=CARTESIAN_POINT('Ctrl Pts',(95.0102568295359,0.196678040591868,-9.85003351292864));
#38949=CARTESIAN_POINT('Ctrl Pts',(95.017693382345,0.251512165546761,-9.85303699826282));
#38950=CARTESIAN_POINT('Ctrl Pts',(95.0282384469924,0.305881530527964,-9.85604048359699));
#38951=CARTESIAN_POINT('Ctrl Pts',(95.0418010573405,0.359415655424122,-9.85904396893116));
#38952=CARTESIAN_POINT('Ctrl Pts',(95.0553892722402,0.413050846208539,-9.86205312447876));
#38953=CARTESIAN_POINT('Ctrl Pts',(95.072006254042,0.465847141931595,-9.86506228002635));
#38954=CARTESIAN_POINT('Ctrl Pts',(95.0915113107741,0.517449879733214,-9.86807143557394));
#38955=CARTESIAN_POINT('Ctrl Pts',(95.1064370725862,0.556937597398208,-9.87037411736439));
#38956=CARTESIAN_POINT('Ctrl Pts',(95.1230529646099,0.595726717173825,-9.87267679915484));
#38957=CARTESIAN_POINT('Ctrl Pts',(95.1412777538414,0.633668034826621,-9.8749794809453));
#38958=CARTESIAN_POINT('Ctrl Pts',(95.1651021765784,0.683266961841729,-9.87798967018303));
#38959=CARTESIAN_POINT('Ctrl Pts',(95.1917777436817,0.731624607382276,-9.88099985942075));
#38960=CARTESIAN_POINT('Ctrl Pts',(95.2211519553535,0.778393148785941,-9.88401004865848));
#38961=CARTESIAN_POINT('Ctrl Pts',(95.2504739534409,0.825078557637538,-9.88701488719024));
#38962=CARTESIAN_POINT('Ctrl Pts',(95.2824847979448,0.870180024375918,-9.89001972572201));
#38963=CARTESIAN_POINT('Ctrl Pts',(95.316985604283,0.913373223436577,-9.89302456425377));
#38964=CARTESIAN_POINT('Ctrl Pts',(95.351452271939,0.956523682658692,-9.89602642948611));
#38965=CARTESIAN_POINT('Ctrl Pts',(95.3884036927349,0.997769204124672,-9.89902829471845));
#38966=CARTESIAN_POINT('Ctrl Pts',(95.4275981411842,1.03681500477504,-9.9020301599508));
#38967=CARTESIAN_POINT('Ctrl Pts',(95.4667692858438,1.07583759001698,-9.90503024036822));
#38968=CARTESIAN_POINT('Ctrl Pts',(95.5081804414227,1.11266267479681,-9.90803032078565));
#38969=CARTESIAN_POINT('Ctrl Pts',(95.551551666227,1.14703086613607,-9.91103040120308));
#38970=CARTESIAN_POINT('Ctrl Pts',(95.5949142316723,1.18139219563296,-9.91402988263411));
#38971=CARTESIAN_POINT('Ctrl Pts',(95.6402356754912,1.21329727807385,-9.91702936406515));
#38972=CARTESIAN_POINT('Ctrl Pts',(95.6872032737517,1.24252721743639,-9.92002884549619));
#38973=CARTESIAN_POINT('Ctrl Pts',(95.7342140256209,1.27178401312992,-9.92303108283667));
#38974=CARTESIAN_POINT('Ctrl Pts',(95.7828735043524,1.29836047552374,-9.92603332017715));
#38975=CARTESIAN_POINT('Ctrl Pts',(95.832841582506,1.32208209839733,-9.92903555751764));
#38976=CARTESIAN_POINT('Ctrl Pts',(95.8828323910048,1.34581451217376,-9.93203916056786));
#38977=CARTESIAN_POINT('Ctrl Pts',(95.9341324955781,1.36668929823868,-9.93504276361809));
#38978=CARTESIAN_POINT('Ctrl Pts',(95.9863818843884,1.38458019861157,-9.93804636666831));
#38979=CARTESIAN_POINT('Ctrl Pts',(96.038729848288,1.40250485243388,-9.9410556363961));
#38980=CARTESIAN_POINT('Ctrl Pts',(96.0920301643488,1.41743423200839,-9.94406490612388));
#38981=CARTESIAN_POINT('Ctrl Pts',(96.1459088968136,1.42929236813893,-9.94707417585166));
#38982=CARTESIAN_POINT('Ctrl Pts',(96.1871193648072,1.43836235395923,-9.94937588949873));
#38983=CARTESIAN_POINT('Ctrl Pts',(96.2286679205669,1.44563660279784,-9.9516776031458));
#38984=CARTESIAN_POINT('Ctrl Pts',(96.2703854375572,1.45110163197136,-9.95397931679287));
#38985=CARTESIAN_POINT('Ctrl Pts',(96.3249448203917,1.45824895617449,-9.95698956488781));
#38986=CARTESIAN_POINT('Ctrl Pts',(96.3800224167897,1.46232997560268,-9.95999981298275));
#38987=CARTESIAN_POINT('Ctrl Pts',(96.4352435718802,1.46328238039245,-9.96301006107769));
#38988=CARTESIAN_POINT('Ctrl Pts',(96.4903666159433,1.46423309305151,-9.96601496088659));
#38989=CARTESIAN_POINT('Ctrl Pts',(96.5456321888077,1.46206621312329,-9.96901986069548));
#38990=CARTESIAN_POINT('Ctrl Pts',(96.6006599733415,1.45677111836295,-9.97202476050438));
#38991=CARTESIAN_POINT('Ctrl Pts',(96.6556333349422,1.45148126049503,-9.97502668844256));
#38992=CARTESIAN_POINT('Ctrl Pts',(96.7103688510263,1.44306936687821,-9.97802861638075));
#38993=CARTESIAN_POINT('Ctrl Pts',(96.7644875417311,1.43157683759092,-9.98103054431893));
#38994=CARTESIAN_POINT('Ctrl Pts',(96.8185740792824,1.42009113627848,-9.98403068874298));
#38995=CARTESIAN_POINT('Ctrl Pts',(96.8720440023069,1.40552853651072,-9.98703083316703));
#38996=CARTESIAN_POINT('Ctrl Pts',(96.9245270922357,1.38798178211517,-9.99003097759107));
#38997=CARTESIAN_POINT('Ctrl Pts',(96.9769997243323,1.37043852410319,-9.99303052420339));
#38998=CARTESIAN_POINT('Ctrl Pts',(97.0284854133109,1.34991245971505,-9.99603007081569));
#38999=CARTESIAN_POINT('Ctrl Pts',(97.0786299477101,1.32654591556683,-9.99902961742801));
#39000=CARTESIAN_POINT('Ctrl Pts',(97.1288205748707,1.30315789293534,-10.0020319212179));
#39001=CARTESIAN_POINT('Ctrl Pts',(97.1776671048263,1.27692439770182,-10.0050342250078));
#39002=CARTESIAN_POINT('Ctrl Pts',(97.224837531989,1.24803496141875,-10.0080365287977));
#39003=CARTESIAN_POINT('Ctrl Pts',(97.2720294290388,1.21913237594506,-10.0110401991032));
#39004=CARTESIAN_POINT('Ctrl Pts',(97.3175432678237,1.18757174105362,-10.0140438694086));
#39005=CARTESIAN_POINT('Ctrl Pts',(97.361076588278,1.15358560391186,-10.0170475397141));
#39006=CARTESIAN_POINT('Ctrl Pts',(97.4046920445891,1.11953534392202,-10.0200568771507));
#39007=CARTESIAN_POINT('Ctrl Pts',(97.4463191197987,1.0830507887586,-10.0230662145873));
#39008=CARTESIAN_POINT('Ctrl Pts',(97.4856898648184,1.04440362413652,-10.0260755520238));
#39009=CARTESIAN_POINT('Ctrl Pts',(97.5157961484908,1.01485065274464,-10.0283767522294));
#39010=CARTESIAN_POINT('Ctrl Pts',(97.5445837589622,0.984033929331002,-10.0306779524349));
#39011=CARTESIAN_POINT('Ctrl Pts',(97.571949066195,0.952087640788239,-10.0329791526404));
#39012=CARTESIAN_POINT('Ctrl Pts',(97.6074588746238,0.910633452953977,-10.0359652392851));
#39013=CARTESIAN_POINT('Ctrl Pts',(97.6407275751511,0.867094924415226,-10.0389513259298));
#39014=CARTESIAN_POINT('Ctrl Pts',(97.6714995489266,0.821745825684147,-10.0419374125744));
#39015=CARTESIAN_POINT('Ctrl Pts',(97.7022257692905,0.776464154411317,-10.0449190593462));
#39016=CARTESIAN_POINT('Ctrl Pts',(97.7304623148778,0.729377683712454,-10.0479007061181));
#39017=CARTESIAN_POINT('Ctrl Pts',(97.7559932347603,0.680793778569701,-10.0508823528899));
#39018=CARTESIAN_POINT('Ctrl Pts',(97.7814966803646,0.632262155433588,-10.0538607910584));
#39019=CARTESIAN_POINT('Ctrl Pts',(97.8043000205057,0.582236763687155,-10.056839229227));
#39020=CARTESIAN_POINT('Ctrl Pts',(97.8242314826978,0.531052477079951,-10.0598176673955));
#39021=CARTESIAN_POINT('Ctrl Pts',(97.8441534630728,0.47989253991768,-10.0627946886582));
#39022=CARTESIAN_POINT('Ctrl Pts',(97.8612060710213,0.427575297084985,-10.0657717099209));
#39023=CARTESIAN_POINT('Ctrl Pts',(97.875265199105,0.374456642733757,-10.0687487311836));
#39024=CARTESIAN_POINT('Ctrl Pts',(97.889320627778,0.321351965616041,-10.0717249690958));
#39025=CARTESIAN_POINT('Ctrl Pts',(97.9003840081287,0.267446816066161,-10.0747012070081));
#39026=CARTESIAN_POINT('Ctrl Pts',(97.9083815176956,0.213110757217513,-10.0776774449203));
#39027=CARTESIAN_POINT('Ctrl Pts',(97.9163831135109,0.158746935896923,-10.0806552035119));
#39028=CARTESIAN_POINT('Ctrl Pts',(97.9213156428349,0.103952298681166,-10.0836329621035));
#39029=CARTESIAN_POINT('Ctrl Pts',(97.9231569701812,0.0491030421626044,
-10.0866107206951));
#39030=CARTESIAN_POINT('Ctrl Pts',(97.9237205505487,0.0323151721445975,
-10.0875221318491));
#39031=CARTESIAN_POINT('Ctrl Pts',(97.9239949143218,0.015522197232046,-10.0884335430031));
#39032=CARTESIAN_POINT('Ctrl Pts',(97.9239804027775,-0.00126510151654843,
-10.0893449541571));
#39033=CARTESIAN_POINT('Origin',(96.460480949577,-8.32667268468867E-16,
1.18130019239114E-14));
#39034=CARTESIAN_POINT('',(97.0954317298417,1.32103105766813,-10.4999624929899));
#39035=CARTESIAN_POINT('Ctrl Pts',(97.9232424573285,-0.00127078615709219,
-10.0893452975919));
#39036=CARTESIAN_POINT('Ctrl Pts',(97.9243963473812,-0.140165259671045,
-10.096889861224));
#39037=CARTESIAN_POINT('Ctrl Pts',(97.8427247309318,-0.762515797147353,
-10.1307677034719));
#39038=CARTESIAN_POINT('Ctrl Pts',(96.9603351573397,-1.65300340041201,-10.1909788243355));
#39039=CARTESIAN_POINT('Ctrl Pts',(95.3490596299417,-1.32199308459857,-10.2699786601832));
#39040=CARTESIAN_POINT('Ctrl Pts',(94.7462060275777,0.208822451170032,-10.3489784960306));
#39041=CARTESIAN_POINT('Ctrl Pts',(95.6701133225779,1.50956345563644,-10.425639773633));
#39042=CARTESIAN_POINT('Ctrl Pts',(96.6979102974993,1.50901532054598,-10.4759677726193));
#39043=CARTESIAN_POINT('Ctrl Pts',(97.0954317298416,1.32103105766813,-10.4999624929899));
#39044=CARTESIAN_POINT('',(95.8264738550018,1.31904027763685,-10.5));
#39045=CARTESIAN_POINT('Origin',(96.460480949577,-2.11854640757359E-15,
-10.5));
#39046=CARTESIAN_POINT('Ctrl Pts',(95.8264738550018,1.31904027763685,-10.5));
#39047=CARTESIAN_POINT('Ctrl Pts',(95.389985305394,1.10923861968599,-10.4736667213841));
#39048=CARTESIAN_POINT('Ctrl Pts',(94.7489680295834,0.225931430401009,-10.4210001641525));
#39049=CARTESIAN_POINT('Ctrl Pts',(95.3368678391471,-1.31284583226671,-10.3420003283048));
#39050=CARTESIAN_POINT('Ctrl Pts',(96.945745154454,-1.65698344561198,-10.2630004924574));
#39051=CARTESIAN_POINT('Ctrl Pts',(97.8393255414646,-0.771433645423267,
-10.202552200022));
#39052=CARTESIAN_POINT('Ctrl Pts',(97.9242498774361,-0.1446116846944,-10.1684371862026));
#39053=CARTESIAN_POINT('Ctrl Pts',(97.923091047352,-0.00131502666372312,
-10.160655450999));
#39054=CARTESIAN_POINT('Origin',(96.460480949577,-7.19464945638997E-16,
0.924367114736168));
#39055=CARTESIAN_POINT('',(95.7870390291235,-0.966214801312794,-10.4999999999999));
#39056=CARTESIAN_POINT('Ctrl Pts',(95.7870390291235,-0.966214801312794,
-10.4999999999999));
#39057=CARTESIAN_POINT('Ctrl Pts',(95.8544328204863,-1.01318759061422,-10.4940933826723));
#39058=CARTESIAN_POINT('Ctrl Pts',(95.9265691194591,-1.05298970580012,-10.4879796024791));
#39059=CARTESIAN_POINT('Ctrl Pts',(96.0554830599743,-1.10743282480879,-10.4778357939815));
#39060=CARTESIAN_POINT('Ctrl Pts',(96.1102754510535,-1.12596123198284,-10.4737357746006));
#39061=CARTESIAN_POINT('Ctrl Pts',(96.1769942019014,-1.14317726828716,-10.468999148222));
#39062=CARTESIAN_POINT('Ctrl Pts',(96.1878131566054,-1.14580595743389,-10.4682386528551));
#39063=CARTESIAN_POINT('Ctrl Pts',(96.2048531906659,-1.14969115664634,-10.4670523381136));
#39064=CARTESIAN_POINT('Ctrl Pts',(96.2110496912719,-1.15105141364629,-10.4666233064918));
#39065=CARTESIAN_POINT('Ctrl Pts',(96.2226437963609,-1.15349853120499,-10.4658248528591));
#39066=CARTESIAN_POINT('Ctrl Pts',(96.2280385893279,-1.15459773247405,-10.4654550574637));
#39067=CARTESIAN_POINT('Ctrl Pts',(96.2401001084916,-1.1569673301482,-10.4646320323687));
#39068=CARTESIAN_POINT('Ctrl Pts',(96.246770542536,-1.15821802060255,-10.4641794217779));
#39069=CARTESIAN_POINT('Ctrl Pts',(96.263714378522,-1.1612435848658,-10.4630359371115));
#39070=CARTESIAN_POINT('Ctrl Pts',(96.274001356937,-1.16293986064668,-10.4623474742393));
#39071=CARTESIAN_POINT('Ctrl Pts',(96.3548783104421,-1.17517532307434,-10.4569766409464));
#39072=CARTESIAN_POINT('Ctrl Pts',(96.4262750274982,-1.17941544920117,-10.4524975226811));
#39073=CARTESIAN_POINT('Ctrl Pts',(96.5497825983152,-1.17551838631524,-10.4448125440057));
#39074=CARTESIAN_POINT('Ctrl Pts',(96.601771553668,-1.17040794904005,-10.4415932459585));
#39075=CARTESIAN_POINT('Ctrl Pts',(96.6881374820688,-1.15607887547855,-10.4360515066784));
#39076=CARTESIAN_POINT('Ctrl Pts',(96.7227452443597,-1.14872223958326,-10.4337764625604));
#39077=CARTESIAN_POINT('Ctrl Pts',(96.7615628452717,-1.1386251872194,-10.4311094906997));
#39078=CARTESIAN_POINT('Ctrl Pts',(96.7661524950613,-1.13740165701946,-10.4307923009737));
#39079=CARTESIAN_POINT('Ctrl Pts',(96.7746719986907,-1.13507519880498,-10.4301998464747));
#39080=CARTESIAN_POINT('Ctrl Pts',(96.7786037828066,-1.13397953423189,-10.4299249650611));
#39081=CARTESIAN_POINT('Ctrl Pts',(96.7855076302119,-1.13201691859115,-10.4294395959154));
#39082=CARTESIAN_POINT('Ctrl Pts',(96.7884821506178,-1.13115863551943,-10.4292295890975));
#39083=CARTESIAN_POINT('Ctrl Pts',(96.7943229246815,-1.12944833415548,-10.4288154131124));
#39084=CARTESIAN_POINT('Ctrl Pts',(96.7971893854899,-1.12859710816218,-10.4286112916624));
#39085=CARTESIAN_POINT('Ctrl Pts',(96.8049184708953,-1.12626980804266,-10.4280586412863));
#39086=CARTESIAN_POINT('Ctrl Pts',(96.8097747654666,-1.12477318355665,-10.4277089822683));
#39087=CARTESIAN_POINT('Ctrl Pts',(96.8291389597203,-1.11866798158017,-10.4263054554145));
#39088=CARTESIAN_POINT('Ctrl Pts',(96.8435658790611,-1.11380997684799,-10.4252389078994));
#39089=CARTESIAN_POINT('Ctrl Pts',(96.9301100207214,-1.08278756005178,-10.4187301073203));
#39090=CARTESIAN_POINT('Ctrl Pts',(96.9996200957762,-1.04990869045323,-10.413046761696));
#39091=CARTESIAN_POINT('Ctrl Pts',(97.1236429017441,-0.975660603296374,
-10.4024873564727));
#39092=CARTESIAN_POINT('Ctrl Pts',(97.1787381628072,-0.935845439251295,
-10.3976122234331));
#39093=CARTESIAN_POINT('Ctrl Pts',(97.2414089403017,-0.88174232736521,-10.3918796147378));
#39094=CARTESIAN_POINT('Ctrl Pts',(97.2525263581025,-0.871769559373845,
-10.3908541924939));
#39095=CARTESIAN_POINT('Ctrl Pts',(97.2686268689341,-0.856764426683987,
-10.3893557592327));
#39096=CARTESIAN_POINT('Ctrl Pts',(97.2737587148631,-0.851894588580639,
-10.3888760717168));
#39097=CARTESIAN_POINT('Ctrl Pts',(97.2827930595554,-0.843165448093971,
-10.3880277521992));
#39098=CARTESIAN_POINT('Ctrl Pts',(97.2867130062517,-0.839324591167573,
-10.3876583536494));
#39099=CARTESIAN_POINT('Ctrl Pts',(97.2949060595357,-0.831183820705522,
-10.3868833974825));
#39100=CARTESIAN_POINT('Ctrl Pts',(97.2991731141308,-0.826878022056163,
-10.3864781093615));
#39101=CARTESIAN_POINT('Ctrl Pts',(97.3103903347578,-0.815382785178269,
-10.385408034293));
#39102=CARTESIAN_POINT('Ctrl Pts',(97.3172826109272,-0.80813734758312,-10.3847457259154));
#39103=CARTESIAN_POINT('Ctrl Pts',(97.3475906889598,-0.775452621156036,
-10.3818100475003));
#39104=CARTESIAN_POINT('Ctrl Pts',(97.3699731455309,-0.749075933191025,
-10.379579532275));
#39105=CARTESIAN_POINT('Ctrl Pts',(97.4528343737023,-0.642227973803992,
-10.3709885142502));
#39106=CARTESIAN_POINT('Ctrl Pts',(97.5040530417584,-0.555137170636209,
-10.3649501606482));
#39107=CARTESIAN_POINT('Ctrl Pts',(97.5520536274543,-0.442752743614256,
-10.3572000895141));
#39108=CARTESIAN_POINT('Ctrl Pts',(97.5599834921799,-0.42267593765064,-10.3558154250398));
#39109=CARTESIAN_POINT('Ctrl Pts',(97.5719878230905,-0.389655297475727,
-10.3535205560766));
#39110=CARTESIAN_POINT('Ctrl Pts',(97.5763983259937,-0.376838362017642,
-10.3526255996791));
#39111=CARTESIAN_POINT('Ctrl Pts',(97.5820623258186,-0.359406579672633,
-10.351399133887));
#39112=CARTESIAN_POINT('Ctrl Pts',(97.5835105443611,-0.354855464003163,
-10.3510780794959));
#39113=CARTESIAN_POINT('Ctrl Pts',(97.5858802805173,-0.347248606473874,
-10.3505398544353));
#39114=CARTESIAN_POINT('Ctrl Pts',(97.5868171454956,-0.344197649506389,
-10.3503235540892));
#39115=CARTESIAN_POINT('Ctrl Pts',(97.5885622074047,-0.338431329294745,
-10.3499138704001));
#39116=CARTESIAN_POINT('Ctrl Pts',(97.5893730286879,-0.33571678845484,-10.3497206413114));
#39117=CARTESIAN_POINT('Ctrl Pts',(97.5912690164379,-0.329284691960429,
-10.349261959504));
#39118=CARTESIAN_POINT('Ctrl Pts',(97.5923456507548,-0.32556467510609,-10.3489960287361));
#39119=CARTESIAN_POINT('Ctrl Pts',(97.5960487638755,-0.312529164963181,
-10.3480620536682));
#39120=CARTESIAN_POINT('Ctrl Pts',(97.5985786550422,-0.303186967959959,
-10.3473889344492));
#39121=CARTESIAN_POINT('Ctrl Pts',(97.6191712142058,-0.223252113596779,
-10.3416035584047));
#39122=CARTESIAN_POINT('Ctrl Pts',(97.6307600479905,-0.15116091643948,-10.3362245342904));
#39123=CARTESIAN_POINT('Ctrl Pts',(97.6394621080441,-0.0208403352663324,
-10.3266425998832));
#39124=CARTESIAN_POINT('Ctrl Pts',(97.6390662658986,0.0369986000578744,
-10.322437653745));
#39125=CARTESIAN_POINT('Ctrl Pts',(97.6327439017465,0.115472762149749,-10.3168608650334));
#39126=CARTESIAN_POINT('Ctrl Pts',(97.630503176332,0.136317535264723,-10.3153913038444));
#39127=CARTESIAN_POINT('Ctrl Pts',(97.6256336464841,0.172499027029182,-10.3128608564475));
#39128=CARTESIAN_POINT('Ctrl Pts',(97.6232552394847,0.187863547373732,-10.3117927216581));
#39129=CARTESIAN_POINT('Ctrl Pts',(97.6193416384434,0.21020926217041,-10.3102479267851));
#39130=CARTESIAN_POINT('Ctrl Pts',(97.6180461034964,0.217230173878387,-10.3097638116526));
#39131=CARTESIAN_POINT('Ctrl Pts',(97.6156502914679,0.229583295954162,-10.3089140995947));
#39132=CARTESIAN_POINT('Ctrl Pts',(97.6145767434501,0.234920408880118,-10.3085476710602));
#39133=CARTESIAN_POINT('Ctrl Pts',(97.6122587266158,0.246044819460985,-10.3077852557351));
#39134=CARTESIAN_POINT('Ctrl Pts',(97.6110075523271,0.251830576791391,-10.3073894926348));
#39135=CARTESIAN_POINT('Ctrl Pts',(97.6076239740772,0.266925351739846,-10.3063588146737));
#39136=CARTESIAN_POINT('Ctrl Pts',(97.6054218443306,0.276218425295059,-10.3057261275267));
#39137=CARTESIAN_POINT('Ctrl Pts',(97.5956113847424,0.315483983633561,-10.3030594832556));
#39138=CARTESIAN_POINT('Ctrl Pts',(97.5869368786744,0.345179010834586,-10.3010596485522));
#39139=CARTESIAN_POINT('Ctrl Pts',(97.547397980448,0.463069430320239,-10.2931337270882));
#39140=CARTESIAN_POINT('Ctrl Pts',(97.5072630980035,0.547785210173771,-10.2874971016047));
#39141=CARTESIAN_POINT('Ctrl Pts',(97.4420020619828,0.651585577764651,-10.2798142703053));
#39142=CARTESIAN_POINT('Ctrl Pts',(97.4255496640518,0.675714136159123,-10.2779637442871));
#39143=CARTESIAN_POINT('Ctrl Pts',(97.3983104963319,0.712635510535071,-10.2749872081784));
#39144=CARTESIAN_POINT('Ctrl Pts',(97.3881180466705,0.725853274181756,-10.2738906294118));
#39145=CARTESIAN_POINT('Ctrl Pts',(97.3744323299601,0.742841992305386,-10.272433478883));
#39146=CARTESIAN_POINT('Ctrl Pts',(97.3711898349455,0.746813681537597,-10.2720893151264));
#39147=CARTESIAN_POINT('Ctrl Pts',(97.3658513982501,0.753266194593324,-10.2715241822711));
#39148=CARTESIAN_POINT('Ctrl Pts',(97.3637709005156,0.75575979859333,-10.2713043034189));
#39149=CARTESIAN_POINT('Ctrl Pts',(97.359675432883,0.760627398716923,-10.2708721093703));
#39150=CARTESIAN_POINT('Ctrl Pts',(97.3576613078154,0.763002072540364,-10.27065985779));
#39151=CARTESIAN_POINT('Ctrl Pts',(97.3531416538762,0.768288151389158,-10.270184287716));
#39152=CARTESIAN_POINT('Ctrl Pts',(97.3506312644098,0.771195327094181,-10.2699206247326));
#39153=CARTESIAN_POINT('Ctrl Pts',(97.3418921451673,0.781216211562879,-10.2690045975254));
#39154=CARTESIAN_POINT('Ctrl Pts',(97.3355921982093,0.788266930284467,-10.2683474316679));
#39155=CARTESIAN_POINT('Ctrl Pts',(97.276907786255,0.852374250616028,-10.2622608328277));
#39156=CARTESIAN_POINT('Ctrl Pts',(97.2191032641449,0.904204020466417,-10.256530893841));
#39157=CARTESIAN_POINT('Ctrl Pts',(97.0933804315891,0.996334927992151,-10.2451102858897));
#39158=CARTESIAN_POINT('Ctrl Pts',(97.0256430012394,1.03626305308206,-10.2394527221208));
#39159=CARTESIAN_POINT('Ctrl Pts',(96.9424876350059,1.07468022866367,-10.2331302766877));
#39160=CARTESIAN_POINT('Ctrl Pts',(96.9304562243289,1.07999597408983,-10.2322292109008));
#39161=CARTESIAN_POINT('Ctrl Pts',(96.9121499761785,1.08772021213893,-10.2308782264583));
#39162=CARTESIAN_POINT('Ctrl Pts',(96.9059397625232,1.09027822993904,-10.2304233460956));
#39163=CARTESIAN_POINT('Ctrl Pts',(96.8946617679668,1.09481124239496,-10.2296033276849));
#39164=CARTESIAN_POINT('Ctrl Pts',(96.889601582798,1.09680450553919,-10.2292375921824));
#39165=CARTESIAN_POINT('Ctrl Pts',(96.8786931441526,1.10101441187411,-10.2284537654709));
#39166=CARTESIAN_POINT('Ctrl Pts',(96.8728406540623,1.10321967508768,-10.228036058337));
#39167=CARTESIAN_POINT('Ctrl Pts',(96.856970520403,1.1090557297753,-10.2269107840463));
#39168=CARTESIAN_POINT('Ctrl Pts',(96.8469205608273,1.11259742517426,-10.226206133973));
#39169=CARTESIAN_POINT('Ctrl Pts',(96.7940470706375,1.13042763136496,-10.2225381149314));
#39170=CARTESIAN_POINT('Ctrl Pts',(96.7504735294051,1.1423825970985,-10.2196509506409));
#39171=CARTESIAN_POINT('Ctrl Pts',(96.6291979447398,1.16826704834721,-10.2118497624505));
#39172=CARTESIAN_POINT('Ctrl Pts',(96.5506246965517,1.17693956619396,-10.2070614215352));
#39173=CARTESIAN_POINT('Ctrl Pts',(96.4319188657766,1.17807812333763,-10.1995940008165));
#39174=CARTESIAN_POINT('Ctrl Pts',(96.3920717450702,1.17643669864132,-10.197044697995));
#39175=CARTESIAN_POINT('Ctrl Pts',(96.3457644474222,1.17216869514144,-10.1939543964287));
#39176=CARTESIAN_POINT('Ctrl Pts',(96.3391449464109,1.17150198250603,-10.193509574419));
#39177=CARTESIAN_POINT('Ctrl Pts',(96.3289477913203,1.17038758031127,-10.1928191065292));
#39178=CARTESIAN_POINT('Ctrl Pts',(96.3253658202838,1.16997947026224,-10.1925755673221));
#39179=CARTESIAN_POINT('Ctrl Pts',(96.3187527039388,1.16919523441498,-10.1921240024915));
#39180=CARTESIAN_POINT('Ctrl Pts',(96.3157210921172,1.16882375693528,-10.191916233542));
#39181=CARTESIAN_POINT('Ctrl Pts',(96.3088014968668,1.1679485331352,-10.1914402719191));
#39182=CARTESIAN_POINT('Ctrl Pts',(96.3049145869711,1.16743716667682,-10.1911716704924));
#39183=CARTESIAN_POINT('Ctrl Pts',(96.2947177621872,1.16604383335837,-10.1904638917223));
#39184=CARTESIAN_POINT('Ctrl Pts',(96.2884124258897,1.16513006754865,-10.1900230702317));
#39185=CARTESIAN_POINT('Ctrl Pts',(96.2360481625204,1.15710714948915,-10.1863375570663));
#39186=CARTESIAN_POINT('Ctrl Pts',(96.1904459829458,1.14732172480013,-10.1829709595529));
#39187=CARTESIAN_POINT('Ctrl Pts',(96.0682801739044,1.11341990657611,-10.1737106503624));
#39188=CARTESIAN_POINT('Ctrl Pts',(95.9933936369627,1.08413893770357,-10.1677827019961));
#39189=CARTESIAN_POINT('Ctrl Pts',(95.9219746556536,1.04742829986771,-10.1620534757847));
#39190=CARTESIAN_POINT('Ctrl Pts',(95.9218881615534,1.04738382680279,-10.1620465370855));
#39191=CARTESIAN_POINT('Ctrl Pts',(95.9218016730735,1.04733934308113,-10.1620395986893));
#39192=CARTESIAN_POINT('',(97.1451453741165,-0.958295198918411,-10.5));
#39193=CARTESIAN_POINT('Origin',(96.460480949577,-2.11854640757359E-15,
-10.5));
#39194=CARTESIAN_POINT('',(97.6382309406263,0.000145201367806521,-10.4243671147812));
#39195=CARTESIAN_POINT('Ctrl Pts',(97.6382309406263,0.000145201367822534,
-10.4243671147812));
#39196=CARTESIAN_POINT('Ctrl Pts',(97.6382368014081,-0.0473924754352446,
-10.4276037988433));
#39197=CARTESIAN_POINT('Ctrl Pts',(97.6353602115632,-0.0950271641440371,
-10.4308404829053));
#39198=CARTESIAN_POINT('Ctrl Pts',(97.6295919559438,-0.142388613631584,
-10.4340771669673));
#39199=CARTESIAN_POINT('Ctrl Pts',(97.6238335157924,-0.189669471200782,
-10.4373083433732));
#39200=CARTESIAN_POINT('Ctrl Pts',(97.6151932243682,-0.236677487308967,
-10.440539519779));
#39201=CARTESIAN_POINT('Ctrl Pts',(97.6037137770981,-0.283043750289888,
-10.4437706961849));
#39202=CARTESIAN_POINT('Ctrl Pts',(97.5922494600277,-0.329348901371691,
-10.4469976138191));
#39203=CARTESIAN_POINT('Ctrl Pts',(97.5779535327664,-0.37501346219832,-10.4502245314534));
#39204=CARTESIAN_POINT('Ctrl Pts',(97.5609199362858,-0.419677374933826,
-10.4534514490876));
#39205=CARTESIAN_POINT('Ctrl Pts',(97.5439022631352,-0.464299534994062,
-10.4566753501378));
#39206=CARTESIAN_POINT('Ctrl Pts',(97.5241521862377,-0.507922406356242,
-10.4598992511881));
#39207=CARTESIAN_POINT('Ctrl Pts',(97.5018131201261,-0.550202120206348,
-10.4631231522383));
#39208=CARTESIAN_POINT('Ctrl Pts',(97.4794789809893,-0.592472509088109,
-10.4663463422436));
#39209=CARTESIAN_POINT('Ctrl Pts',(97.454557220798,-0.633399850627232,-10.4695695322489));
#39210=CARTESIAN_POINT('Ctrl Pts',(97.4272380850568,-0.672663142664198,
-10.4727927222543));
#39211=CARTESIAN_POINT('Ctrl Pts',(97.3999245324198,-0.711918410616832,
-10.4760152535489));
#39212=CARTESIAN_POINT('Ctrl Pts',(97.370214886659,-0.749509870604237,-10.4792377848436));
#39213=CARTESIAN_POINT('Ctrl Pts',(97.3383422154285,-0.785146266893978,
-10.4824603161383));
#39214=CARTESIAN_POINT('Ctrl Pts',(97.3064421588081,-0.820813282412446,
-10.4856856162714));
#39215=CARTESIAN_POINT('Ctrl Pts',(97.2723757229821,-0.854521483376949,
-10.4889109164044));
#39216=CARTESIAN_POINT('Ctrl Pts',(97.236414587066,-0.886014702312063,-10.4921362165375));
#39217=CARTESIAN_POINT('Ctrl Pts',(97.2071883058683,-0.911609824628666,
-10.4947574776917));
#39218=CARTESIAN_POINT('Ctrl Pts',(97.1767113679881,-0.935742531375487,
-10.4973787388458));
#39219=CARTESIAN_POINT('Ctrl Pts',(97.1451453741165,-0.958295198918386,
-10.5));
#39220=CARTESIAN_POINT('Ctrl Pts',(95.9218016730721,1.04733934308042,-10.2615611054409));
#39221=CARTESIAN_POINT('Ctrl Pts',(95.9280836198898,1.05057034417782,-10.262040901113));
#39222=CARTESIAN_POINT('Ctrl Pts',(95.9343926980404,1.05374382729346,-10.2625206967852));
#39223=CARTESIAN_POINT('Ctrl Pts',(95.9407277584678,1.05685934865135,-10.2630004924573));
#39224=CARTESIAN_POINT('Ctrl Pts',(95.9841897259695,1.07823352330357,-10.2662921522843));
#39225=CARTESIAN_POINT('Ctrl Pts',(96.0290697844585,1.09697019344544,-10.2695838121113));
#39226=CARTESIAN_POINT('Ctrl Pts',(96.0750142256799,1.11288385165212,-10.2728754719383));
#39227=CARTESIAN_POINT('Ctrl Pts',(96.1193341606865,1.12823483380984,-10.2760507450664));
#39228=CARTESIAN_POINT('Ctrl Pts',(96.164643883886,1.14095891506093,-10.2792260181944));
#39229=CARTESIAN_POINT('Ctrl Pts',(96.2106024746863,1.15093692715382,-10.2824012913225));
#39230=CARTESIAN_POINT('Ctrl Pts',(96.2565163429393,1.16090522959048,-10.2855734745756));
#39231=CARTESIAN_POINT('Ctrl Pts',(96.3030772877012,1.16813263488393,-10.2887456578286));
#39232=CARTESIAN_POINT('Ctrl Pts',(96.3499301376088,1.17255003324939,-10.2919178410817));
#39233=CARTESIAN_POINT('Ctrl Pts',(96.3967578963307,1.17696506595808,-10.2950883255301));
#39234=CARTESIAN_POINT('Ctrl Pts',(96.4438766976299,1.17857302092982,-10.2982588099785));
#39235=CARTESIAN_POINT('Ctrl Pts',(96.4909248041402,1.17735646013403,-10.3014292944269));
#39236=CARTESIAN_POINT('Ctrl Pts',(96.5379683002796,1.17614001855231,-10.304599468191));
#39237=CARTESIAN_POINT('Ctrl Pts',(96.584940559731,1.1720996274432,-10.3077696419551));
#39238=CARTESIAN_POINT('Ctrl Pts',(96.6314811217072,1.16526992736938,-10.3109398157192));
#39239=CARTESIAN_POINT('Ctrl Pts',(96.678069400412,1.15843322499627,-10.3141132397733));
#39240=CARTESIAN_POINT('Ctrl Pts',(96.724224547625,1.14880159031184,-10.3172866638273));
#39241=CARTESIAN_POINT('Ctrl Pts',(96.7695944703289,1.13646112726673,-10.3204600878813));
#39242=CARTESIAN_POINT('Ctrl Pts',(96.8149924393552,1.12411303571833,-10.3236354736507));
#39243=CARTESIAN_POINT('Ctrl Pts',(96.8596036908615,1.1090529615634,-10.3268108594201));
#39244=CARTESIAN_POINT('Ctrl Pts',(96.9030930134713,1.09141633824824,-10.3299862451895));
#39245=CARTESIAN_POINT('Ctrl Pts',(96.9466605320552,1.07374800340354,-10.3331673404611));
#39246=CARTESIAN_POINT('Ctrl Pts',(96.9891015976539,1.05349412008248,-10.3363484357327));
#39247=CARTESIAN_POINT('Ctrl Pts',(97.0301043730256,1.03083665920392,-10.3395295310043));
#39248=CARTESIAN_POINT('Ctrl Pts',(97.0407201660206,1.02497054618352,-10.3403531301045));
#39249=CARTESIAN_POINT('Ctrl Pts',(97.0512397004402,1.0189435435138,-10.3411767292047));
#39250=CARTESIAN_POINT('Ctrl Pts',(97.0616578984223,1.01275926985492,-10.3420003283049));
#39251=CARTESIAN_POINT('Ctrl Pts',(97.1032960737916,0.988042723713015,-10.3452919881319));
#39252=CARTESIAN_POINT('Ctrl Pts',(97.1435148709796,0.960690062866965,-10.3485836479588));
#39253=CARTESIAN_POINT('Ctrl Pts',(97.1819585355496,0.930894814379747,-10.3518753077858));
#39254=CARTESIAN_POINT('Ctrl Pts',(97.2186428708157,0.902463110558934,-10.3550163286543));
#39255=CARTESIAN_POINT('Ctrl Pts',(97.2537105004253,0.871807916615277,-10.3581573495228));
#39256=CARTESIAN_POINT('Ctrl Pts',(97.2868787612889,0.839143443815064,-10.3612983703912));
#39257=CARTESIAN_POINT('Ctrl Pts',(97.3200145729144,0.806510927386065,-10.36443631833));
#39258=CARTESIAN_POINT('Ctrl Pts',(97.351254286152,0.7718734167847,-10.3675742662687));
#39259=CARTESIAN_POINT('Ctrl Pts',(97.380349063542,0.735484680608969,-10.3707122142075));
#39260=CARTESIAN_POINT('Ctrl Pts',(97.4094288083644,0.699114745612872,-10.3738485408445));
#39261=CARTESIAN_POINT('Ctrl Pts',(97.4363654556145,0.66099582000426,-10.3769848674815));
#39262=CARTESIAN_POINT('Ctrl Pts',(97.4609497080266,0.621415582252544,-10.3801211941184));
#39263=CARTESIAN_POINT('Ctrl Pts',(97.4855326067524,0.581837523913344,-10.3832573480594));
#39264=CARTESIAN_POINT('Ctrl Pts',(97.5077630698396,0.540798798312993,-10.3863935020003));
#39265=CARTESIAN_POINT('Ctrl Pts',(97.5274760904889,0.498614512193911,-10.3895296559413));
#39266=CARTESIAN_POINT('Ctrl Pts',(97.5472123600316,0.45638047530423,-10.3926695085599));
#39267=CARTESIAN_POINT('Ctrl Pts',(97.5644250256606,0.412998700993198,-10.3958093611785));
#39268=CARTESIAN_POINT('Ctrl Pts',(97.5789967832024,0.36880535846057,-10.398949213797));
#39269=CARTESIAN_POINT('Ctrl Pts',(97.5935786471709,0.32458136507679,-10.4020912441001));
#39270=CARTESIAN_POINT('Ctrl Pts',(97.6055158193112,0.279545235778642,-10.4052332744031));
#39271=CARTESIAN_POINT('Ctrl Pts',(97.6147416237034,0.234045633723838,-10.4083753047062));
#39272=CARTESIAN_POINT('Ctrl Pts',(97.6239861174384,0.188453860014178,-10.4115237000348));
#39273=CARTESIAN_POINT('Ctrl Pts',(97.6305082170572,0.142397304832613,-10.4146720953635));
#39274=CARTESIAN_POINT('Ctrl Pts',(97.6342930436276,0.0962300907233125,
-10.4178204906922));
#39275=CARTESIAN_POINT('Ctrl Pts',(97.6355671860971,0.0806881346777844,
-10.4188803818456));
#39276=CARTESIAN_POINT('Ctrl Pts',(97.6365315514698,0.0651336273818042,
-10.419940272999));
#39277=CARTESIAN_POINT('Ctrl Pts',(97.6371868971856,0.0495799895370037,
-10.4210001641524));
#39278=CARTESIAN_POINT('Ctrl Pts',(97.6378808416011,0.0331102700276012,
-10.4221224810136));
#39279=CARTESIAN_POINT('Ctrl Pts',(97.6382289083969,0.0166288424470303,
-10.4232447978749));
#39280=CARTESIAN_POINT('Ctrl Pts',(97.6382309406262,0.000145202030728477,
-10.4243671147361));
#39281=CARTESIAN_POINT('Ctrl Pts',(96.9698189919063,1.05966857234488,0.166148582192736));
#39282=CARTESIAN_POINT('Ctrl Pts',(97.3204778808345,0.89112161655769,0.139815303576882));
#39283=CARTESIAN_POINT('Ctrl Pts',(97.8354473421669,0.181504183543753,0.0871487463451743));
#39284=CARTESIAN_POINT('Ctrl Pts',(97.3631507055241,-1.05469178959263,0.00814891049761157));
#39285=CARTESIAN_POINT('Ctrl Pts',(96.0706374094237,-1.33116003884258,-0.0708509253499507));
#39286=CARTESIAN_POINT('Ctrl Pts',(95.1324539764634,-0.40140754516674,-0.149850761197514));
#39287=CARTESIAN_POINT('Ctrl Pts',(95.398731272582,0.893221222269588,-0.228850597045076));
#39288=CARTESIAN_POINT('Ctrl Pts',(96.6284070005896,1.37714878342488,-0.307850432892638));
#39289=CARTESIAN_POINT('Ctrl Pts',(97.7056520100152,0.611901250598986,-0.386850268740201));
#39290=CARTESIAN_POINT('Ctrl Pts',(97.6533122610813,-0.708562065134396,
-0.465850104587763));
#39291=CARTESIAN_POINT('Ctrl Pts',(96.5188040922679,-1.38616440608763,-0.544849940435326));
#39292=CARTESIAN_POINT('Ctrl Pts',(95.3313961518403,-0.806251887258617,
-0.623849776282889));
#39293=CARTESIAN_POINT('Ctrl Pts',(95.1682969837761,0.505111073403053,-0.702849612130451));
#39294=CARTESIAN_POINT('Ctrl Pts',(96.177480216103,1.35822699414563,-0.781849447978014));
#39295=CARTESIAN_POINT('Ctrl Pts',(97.4434024291193,0.97915193147552,-0.860849283825576));
#39296=CARTESIAN_POINT('Ctrl Pts',(97.8176113252564,-0.288219083786204,
-0.939849119673137));
#39297=CARTESIAN_POINT('Ctrl Pts',(96.9606204994759,-1.29411465266134,-1.0188489555207));
#39298=CARTESIAN_POINT('Ctrl Pts',(95.6498993457129,-1.12597967087778,-1.09784879136826));
#39299=CARTESIAN_POINT('Ctrl Pts',(95.0745440861015,0.0636531236609935,
-1.17684862721583));
#39300=CARTESIAN_POINT('Ctrl Pts',(95.7565216816914,1.19553919527067,-1.25584846306339));
#39301=CARTESIAN_POINT('Ctrl Pts',(97.0771366259267,1.24282277813268,-1.33484829891095));
#39302=CARTESIAN_POINT('Ctrl Pts',(97.8383167123646,0.162607750675068,-1.41384813475851));
#39303=CARTESIAN_POINT('Ctrl Pts',(97.3495133703376,-1.06512629046087,-1.49284797060608));
#39304=CARTESIAN_POINT('Ctrl Pts',(96.054172839641,-1.32656940567028,-1.57184780645364));
#39305=CARTESIAN_POINT('Ctrl Pts',(95.1274382145455,-0.38453833712907,-1.6508476423012));
#39306=CARTESIAN_POINT('Ctrl Pts',(95.4100504255828,0.906348928056774,-1.72984747814876));
#39307=CARTESIAN_POINT('Ctrl Pts',(96.6456214547034,1.37498933072291,-1.80884731399633));
#39308=CARTESIAN_POINT('Ctrl Pts',(97.713231564224,0.596228616712231,-1.88784714984389));
#39309=CARTESIAN_POINT('Ctrl Pts',(97.6443364803891,-0.723435379256512,
-1.96684698569145));
#39310=CARTESIAN_POINT('Ctrl Pts',(96.5014383643424,-1.38679311943509,-2.04584682153901));
#39311=CARTESIAN_POINT('Ctrl Pts',(95.3213833600239,-0.792041253569239,
-2.12484665738657));
#39312=CARTESIAN_POINT('Ctrl Pts',(95.1747266322779,0.521256655997792,-2.20384649323414));
#39313=CARTESIAN_POINT('Ctrl Pts',(96.1945163159272,1.36166643475577,-2.2828463290817));
#39314=CARTESIAN_POINT('Ctrl Pts',(97.4555912033766,0.966761733141859,-2.36184616492926));
#39315=CARTESIAN_POINT('Ctrl Pts',(97.8138942557399,-0.305196803040322,
-2.44084600077682));
#39316=CARTESIAN_POINT('Ctrl Pts',(96.9443701307973,-1.300278403337,-2.51984583662439));
#39317=CARTESIAN_POINT('Ctrl Pts',(95.6358579415274,-1.11573722734368,-2.59884567247195));
#39318=CARTESIAN_POINT('Ctrl Pts',(95.0754502194629,0.0810095212020413,
-2.67784550831951));
#39319=CARTESIAN_POINT('Ctrl Pts',(95.7715532499494,1.20426379608938,-2.75684534416707));
#39320=CARTESIAN_POINT('Ctrl Pts',(97.092656898466,1.23500050021526,-2.83584518001464));
#39321=CARTESIAN_POINT('Ctrl Pts',(97.8402455627935,0.145335054276059,-2.9148450158622));
#39322=CARTESIAN_POINT('Ctrl Pts',(97.3361009371651,-1.076179493961,-2.99384485170976));
#39323=CARTESIAN_POINT('Ctrl Pts',(96.037586984105,-1.32137555594659,-3.07284468755733));
#39324=CARTESIAN_POINT('Ctrl Pts',(95.1227257567579,-0.36780933915736,-3.15184452340489));
#39325=CARTESIAN_POINT('Ctrl Pts',(95.4214865433566,0.919436397870225,-3.23084435925245));
#39326=CARTESIAN_POINT('Ctrl Pts',(96.66283121266,1.37256221604562,-3.30984419510002));
#39327=CARTESIAN_POINT('Ctrl Pts',(97.7206021345964,0.580488815526218,-3.38884403094757));
#39328=CARTESIAN_POINT('Ctrl Pts',(97.6351812239852,-0.738208595988316,
-3.46784386679515));
#39329=CARTESIAN_POINT('Ctrl Pts',(96.4840630015917,-1.38719737337863,-3.54684370264269));
#39330=CARTESIAN_POINT('Ctrl Pts',(95.3115509564625,-0.777709802437698,
-3.62584353849027));
#39331=CARTESIAN_POINT('Ctrl Pts',(95.1813572215973,0.53732220725129,-3.70484337433782));
#39332=CARTESIAN_POINT('Ctrl Pts',(96.2115945754469,1.36489129188303,-3.78384321018539));
#39333=CARTESIAN_POINT('Ctrl Pts',(97.4676236019706,0.954220280446444,-3.86284304603295));
#39334=CARTESIAN_POINT('Ctrl Pts',(97.809964906937,-0.322126861211645,-3.94184288188052));
#39335=CARTESIAN_POINT('Ctrl Pts',(96.9280437706806,-1.30623798528726,-4.02084271772807));
#39336=CARTESIAN_POINT('Ctrl Pts',(95.6219459721774,-1.10531975353869,-4.09984255357564));
#39337=CARTESIAN_POINT('Ctrl Pts',(95.0765736886995,0.098353236737004,-4.1788423894232));
#39338=CARTESIAN_POINT('Ctrl Pts',(95.7866929376608,1.21279939845126,-4.25784222527076));
#39339=CARTESIAN_POINT('Ctrl Pts',(97.1080779610953,1.22698442392656,-4.33684206111833));
#39340=CARTESIAN_POINT('Ctrl Pts',(97.8419578912489,0.128039546681841,-4.41584189696589));
#39341=CARTESIAN_POINT('Ctrl Pts',(97.3225510936281,-1.08706381258025,-4.49484173281344));
#39342=CARTESIAN_POINT('Ctrl Pts',(96.0210674930154,-1.31597434628425,-4.57384156866102));
#39343=CARTESIAN_POINT('Ctrl Pts',(95.1182232301301,-0.351022621025214,
-4.65284140450857));
#39344=CARTESIAN_POINT('Ctrl Pts',(95.433085708698,0.932379581986348,-4.73184124035615));
#39345=CARTESIAN_POINT('Ctrl Pts',(96.6800092161049,1.36991970789569,-4.81084107620369));
#39346=CARTESIAN_POINT('Ctrl Pts',(97.7277749565514,0.564657919250789,-4.88984091205127));
#39347=CARTESIAN_POINT('Ctrl Pts',(97.6258416240571,-0.752865966996209,
-4.96884074789882));
#39348=CARTESIAN_POINT('Ctrl Pts',(96.4666839381626,-1.38738393706227,-5.04784058374639));
#39349=CARTESIAN_POINT('Ctrl Pts',(95.3018988523223,-0.763256306758528,
-5.12684041959395));
#39350=CARTESIAN_POINT('Ctrl Pts',(95.188188541403,0.553303437535439,-5.20584025544151));
#39351=CARTESIAN_POINT('Ctrl Pts',(96.2287118922362,1.3679019591861,-5.28484009128907));
#39352=CARTESIAN_POINT('Ctrl Pts',(97.4794979515607,0.941529083753663,-5.36383992713664));
#39353=CARTESIAN_POINT('Ctrl Pts',(97.8058237861511,-0.339006368619123,
-5.4428397629842));
#39354=CARTESIAN_POINT('Ctrl Pts',(96.911644036809,-1.31199258176452,-5.52183959883176));
#39355=CARTESIAN_POINT('Ctrl Pts',(95.6081655925459,-1.09472882398092,-5.60083943467933));
#39356=CARTESIAN_POINT('Ctrl Pts',(95.077914331903,0.115681517883201,-5.67983927052688));
#39357=CARTESIAN_POINT('Ctrl Pts',(95.8019383616594,1.22114467848177,-5.75883910637445));
#39358=CARTESIAN_POINT('Ctrl Pts',(97.1233973975418,1.21877579927701,-5.83783894222201));
#39359=CARTESIAN_POINT('Ctrl Pts',(97.8434534271231,0.110723946082075,-5.91683877806957));
#39360=CARTESIAN_POINT('Ctrl Pts',(97.3088659670429,-1.0977775403174,-5.99583861391714));
#39361=CARTESIAN_POINT('Ctrl Pts',(96.0046169582537,-1.31036662323974,-6.0748384497647));
#39362=CARTESIAN_POINT('Ctrl Pts',(95.1139313414852,-0.334180817572524,
-6.15383828561227));
#39363=CARTESIAN_POINT('Ctrl Pts',(95.4448461012445,0.9451764495261,-6.23283812145983));
#39364=CARTESIAN_POINT('Ctrl Pts',(96.6971527693917,1.36706222081932,-6.31183795730738));
#39365=CARTESIAN_POINT('Ctrl Pts',(97.7347489044381,0.548738412268767,-6.39083779315495));
#39366=CARTESIAN_POINT('Ctrl Pts',(97.6163191462674,-0.767405192162125,
-6.46983762900251));
#39367=CARTESIAN_POINT('Ctrl Pts',(96.4493039013101,-1.3873527811908,-6.54883746485007));
#39368=CARTESIAN_POINT('Ctrl Pts',(95.2924285622943,-0.748683034700886,
-6.62783730069764));
#39369=CARTESIAN_POINT('Ctrl Pts',(95.1952195196663,0.569197838950488,-6.7068371365452));
#39370=CARTESIAN_POINT('Ctrl Pts',(96.2458655801085,1.37069796420425,-6.78583697239276));
#39371=CARTESIAN_POINT('Ctrl Pts',(97.4912123887268,0.928690134670386,-6.86483680824032));
#39372=CARTESIAN_POINT('Ctrl Pts',(97.8014715432413,-0.355832676393984,
-6.94383664408789));
#39373=CARTESIAN_POINT('Ctrl Pts',(96.8951735027615,-1.31754128971044,-7.02283647993545));
#39374=CARTESIAN_POINT('Ctrl Pts',(95.5945189651623,-1.08396610068519,-7.10183631578301));
#39375=CARTESIAN_POINT('Ctrl Pts',(95.079471938689,0.132991645346109,-7.18083615163058));
#39376=CARTESIAN_POINT('Ctrl Pts',(95.8172871295089,1.22929832657175,-7.25983598747813));
#39377=CARTESIAN_POINT('Ctrl Pts',(97.1386128037557,1.21037591443069,-7.3388358233257));
#39378=CARTESIAN_POINT('Ctrl Pts',(97.8447319357241,0.093390969781441,-7.41783565917326));
#39379=CARTESIAN_POINT('Ctrl Pts',(97.2950477049903,-1.10831899588724,-7.49683549502083));
#39380=CARTESIAN_POINT('Ctrl Pts',(95.9882379613722,-1.30455326682254,-7.57583533086838));
#39381=CARTESIAN_POINT('Ctrl Pts',(95.1098507643406,-0.317286571751796,
-7.65483516671596));
#39382=CARTESIAN_POINT('Ctrl Pts',(95.4567658754601,0.957824992300916,-7.7338350025635));
#39383=CARTESIAN_POINT('Ctrl Pts',(96.7142591822142,1.36399020323693,-7.81283483841108));
#39384=CARTESIAN_POINT('Ctrl Pts',(97.7415228838485,0.532732792797828,-7.89183467425863));
#39385=CARTESIAN_POINT('Ctrl Pts',(97.6066152849611,-0.781823989871474,
-7.9708345101062));
#39386=CARTESIAN_POINT('Ctrl Pts',(96.4319256184501,-1.38710391065599,-8.04983434595377));
#39387=CARTESIAN_POINT('Ctrl Pts',(95.2831415725345,-0.733992273215962,
-8.12883418180132));
#39388=CARTESIAN_POINT('Ctrl Pts',(95.2024490530263,0.585002917208061,-8.2078340176489));
#39389=CARTESIAN_POINT('Ctrl Pts',(96.2630529471728,1.373278868185,-8.28683385349645));
#39390=CARTESIAN_POINT('Ctrl Pts',(97.502765075134,0.915705447950804,-8.36583368934401));
#39391=CARTESIAN_POINT('Ctrl Pts',(97.7969088612167,-0.37260314394072,-8.44483352519157));
#39392=CARTESIAN_POINT('Ctrl Pts',(96.878634753188,-1.32288323852336,-8.52383336103914));
#39393=CARTESIAN_POINT('Ctrl Pts',(95.5810082316452,-1.07303327233716,-8.6028331968867));
#39394=CARTESIAN_POINT('Ctrl Pts',(95.08124626447,0.150280902113239,-8.68183303273427));
#39395=CARTESIAN_POINT('Ctrl Pts',(95.8327368328608,1.23725906429836,-8.76083286858181));
#39396=CARTESIAN_POINT('Ctrl Pts',(97.1537217914135,1.20178608537639,-8.8398327044294));
#39397=CARTESIAN_POINT('Ctrl Pts',(97.8457932175932,0.0760433421147284,
-8.91883254027695));
#39398=CARTESIAN_POINT('Ctrl Pts',(97.2810984736349,-1.11868653349764,-8.99783237612451));
#39399=CARTESIAN_POINT('Ctrl Pts',(95.9719330772361,-1.29853517268555,-9.07683221197208));
#39400=CARTESIAN_POINT('Ctrl Pts',(95.1059821301293,-0.300342567425433,
-9.15583204781964));
#39401=CARTESIAN_POINT('Ctrl Pts',(95.4688431783388,0.970323289634254,-9.2348318836672));
#39402=CARTESIAN_POINT('Ctrl Pts',(96.7313257356152,1.36070401097439,-9.31383171951477));
#39403=CARTESIAN_POINT('Ctrl Pts',(97.7480958995279,0.516643820744214,-9.39283155536233));
#39404=CARTESIAN_POINT('Ctrl Pts',(97.5967314297322,-0.796120585216384,
-9.47183139120988));
#39405=CARTESIAN_POINT('Ctrl Pts',(96.4145520785679,-1.38663640568844,-9.55083122705745));
#39406=CARTESIAN_POINT('Ctrl Pts',(95.2740388257579,-0.719188212344122,
-9.62983106290501));
#39407=CARTESIAN_POINT('Ctrl Pts',(95.2098770186021,0.600719896472962,-9.70883089875258));
#39408=CARTESIAN_POINT('Ctrl Pts',(96.2802693077949,1.37563698476155,-9.78783073460014));
#39409=CARTESIAN_POINT('Ctrl Pts',(97.5141581063061,0.902591373346843,-9.86683057044771));
#39410=CARTESIAN_POINT('Ctrl Pts',(97.7921287736904,-0.389343271126291,
-9.94583040629525));
#39411=CARTESIAN_POINT('Ctrl Pts',(96.8620454838072,-1.32796229432384,-10.0248302421428));
#39412=CARTESIAN_POINT('Ctrl Pts',(95.5676058319486,-1.06204074913918,-10.1038300779904));
#39413=CARTESIAN_POINT('Ctrl Pts',(95.0832953624497,0.167760296979913,-10.182829913838));
#39414=CARTESIAN_POINT('Ctrl Pts',(95.8481704737817,1.24460472281043,-10.2618297496855));
#39415=CARTESIAN_POINT('Ctrl Pts',(97.1689462680908,1.19384435828083,-10.3408295855331));
#39416=CARTESIAN_POINT('Ctrl Pts',(97.846259559098,0.0568453784873504,-10.4198356323639));
#39417=CARTESIAN_POINT('Ctrl Pts',(97.4604426383845,-0.730656199282666,
-10.4725084005789));
#39418=CARTESIAN_POINT('Ctrl Pts',(97.1437425383552,-0.956805267514262,
-10.4988478901781));
#39419=CARTESIAN_POINT('Ctrl Pts',(97.0116446152009,1.14668602409723,0.110406857325715));
#39420=CARTESIAN_POINT('Ctrl Pts',(97.39109877441,0.964298394937262,0.0840735787098607));
#39421=CARTESIAN_POINT('Ctrl Pts',(97.9483562977128,0.196408873506787,0.0314070214781526));
#39422=CARTESIAN_POINT('Ctrl Pts',(97.4372757895234,-1.14130055983423,-0.0475928143694103));
#39423=CARTESIAN_POINT('Ctrl Pts',(96.0386243891912,-1.44047172126636,-0.126592650216973));
#39424=CARTESIAN_POINT('Ctrl Pts',(95.0233995739129,-0.434370173866093,
-0.205592486064536));
#39425=CARTESIAN_POINT('Ctrl Pts',(95.3115429254873,0.966570415254535,-0.284592321912098));
#39426=CARTESIAN_POINT('Ctrl Pts',(96.6421966867455,1.4902369516927,-0.363592157759661));
#39427=CARTESIAN_POINT('Ctrl Pts',(97.807902482949,0.662149119546701,-0.442591993607223));
#39428=CARTESIAN_POINT('Ctrl Pts',(97.7512647188651,-0.766747489261799,
-0.521591829454785));
#39429=CARTESIAN_POINT('Ctrl Pts',(96.5235934494195,-1.49999291575139,-0.600591665302348));
#39430=CARTESIAN_POINT('Ctrl Pts',(95.238678405485,-0.872459366210753,-0.679591501149911));
#39431=CARTESIAN_POINT('Ctrl Pts',(95.0621859233619,0.546589588107095,-0.758591336997473));
#39432=CARTESIAN_POINT('Ctrl Pts',(96.1542408719215,1.46976135027951,-0.837591172845036));
#39433=CARTESIAN_POINT('Ctrl Pts',(97.5241175929496,1.05955754902332,-0.916591008692599));
#39434=CARTESIAN_POINT('Ctrl Pts',(97.9290556297016,-0.3118869464293,-0.995590844540159));
#39435=CARTESIAN_POINT('Ctrl Pts',(97.0016907645461,-1.40038425646847,-1.07459068038772));
#39436=CARTESIAN_POINT('Ctrl Pts',(95.5833363207763,-1.21844243163316,-1.15359051623528));
#39437=CARTESIAN_POINT('Ctrl Pts',(94.9607342616933,0.0688801661171027,
-1.23259035208285));
#39438=CARTESIAN_POINT('Ctrl Pts',(95.6987142282786,1.29371401800065,-1.31159018793041));
#39439=CARTESIAN_POINT('Ctrl Pts',(97.1277749169594,1.34488041573305,-1.39059002377797));
#39440=CARTESIAN_POINT('Ctrl Pts',(97.9514612937366,0.175960710712014,-1.46958985962553));
#39441=CARTESIAN_POINT('Ctrl Pts',(97.4225185889493,-1.15259191698711,-1.5485896954731));
#39442=CARTESIAN_POINT('Ctrl Pts',(96.0208077882696,-1.43550411626438,-1.62758953132066));
#39443=CARTESIAN_POINT('Ctrl Pts',(95.0179719296082,-0.416115706762684,
-1.70658936716822));
#39444=CARTESIAN_POINT('Ctrl Pts',(95.3237915802923,0.980776136880604,-1.78558920301579));
#39445=CARTESIAN_POINT('Ctrl Pts',(96.6608247507084,1.4879001698935,-1.86458903886335));
#39446=CARTESIAN_POINT('Ctrl Pts',(97.8161044520424,0.645189486405023,-1.94358887471091));
#39447=CARTESIAN_POINT('Ctrl Pts',(97.7415518685047,-0.782842164409236,
-2.02258871055847));
#39448=CARTESIAN_POINT('Ctrl Pts',(96.5048016894009,-1.50067325753703,-2.10158854640604));
#39449=CARTESIAN_POINT('Ctrl Pts',(95.2278433871241,-0.857081789230136,
-2.1805883822536));
#39450=CARTESIAN_POINT('Ctrl Pts',(95.0691435592389,0.564061007374844,-2.25958821810116));
#39451=CARTESIAN_POINT('Ctrl Pts',(96.1726759355667,1.47348322953618,-2.33858805394872));
#39452=CARTESIAN_POINT('Ctrl Pts',(97.5373072802312,1.04614989720104,-2.41758788979629));
#39453=CARTESIAN_POINT('Ctrl Pts',(97.9250333233159,-0.330258835431031,
-2.49658772564385));
#39454=CARTESIAN_POINT('Ctrl Pts',(96.9841059544115,-1.40705415962521,-2.57558756149141));
#39455=CARTESIAN_POINT('Ctrl Pts',(95.5681418700222,-1.20735890310389,-2.65458739733897));
#39456=CARTESIAN_POINT('Ctrl Pts',(94.9617148045619,0.087661829562074,-2.73358723318654));
#39457=CARTESIAN_POINT('Ctrl Pts',(95.7149801530134,1.30315506219667,-2.81258706903409));
#39458=CARTESIAN_POINT('Ctrl Pts',(97.1445696772038,1.33641579103944,-2.89158690488166));
#39459=CARTESIAN_POINT('Ctrl Pts',(97.9535485367549,0.157269621746915,-2.97058674072922));
#39460=CARTESIAN_POINT('Ctrl Pts',(97.408004758805,-1.16455278315403,-3.04958657657678));
#39461=CARTESIAN_POINT('Ctrl Pts',(96.0028599418983,-1.4298837600088,-3.12858641242435));
#39462=CARTESIAN_POINT('Ctrl Pts',(95.0128724960447,-0.398012963440909,
-3.20758624827191));
#39463=CARTESIAN_POINT('Ctrl Pts',(95.3361668047384,0.994938318450894,-3.28658608411947));
#39464=CARTESIAN_POINT('Ctrl Pts',(96.6794477328763,1.48527374635697,-3.36558591996704));
#39465=CARTESIAN_POINT('Ctrl Pts',(97.8240802760465,0.628157170345926,-3.44458575581459));
#39466=CARTESIAN_POINT('Ctrl Pts',(97.7316448043156,-0.798828522407786,
-3.52358559166216));
#39467=CARTESIAN_POINT('Ctrl Pts',(96.4859995033687,-1.5011107078487,-3.60258542750972));
#39468=CARTESIAN_POINT('Ctrl Pts',(95.2172035700704,-0.841573473567619,
-3.68158526335729));
#39469=CARTESIAN_POINT('Ctrl Pts',(95.0763186367137,0.581445823318793,-3.76058509920484));
#39470=CARTESIAN_POINT('Ctrl Pts',(96.1911566209602,1.47697290422696,-3.83958493505241));
#39471=CARTESIAN_POINT('Ctrl Pts',(97.5503277506541,1.03257857037017,-3.91858477089997));
#39472=CARTESIAN_POINT('Ctrl Pts',(97.9207813057759,-0.348579149535705,
-3.99758460674753));
#39473=CARTESIAN_POINT('Ctrl Pts',(96.9664389126037,-1.41350312820859,-4.0765844425951));
#39474=CARTESIAN_POINT('Ctrl Pts',(95.5530874829827,-1.19608597123602,-4.15558427844266));
#39475=CARTESIAN_POINT('Ctrl Pts',(94.9629305304085,0.106429769584916,-4.23458411429023));
#39476=CARTESIAN_POINT('Ctrl Pts',(95.731363075713,1.31239158783408,-4.31358395013778));
#39477=CARTESIAN_POINT('Ctrl Pts',(97.1612570806572,1.32774145371525,-4.39258378598535));
#39478=CARTESIAN_POINT('Ctrl Pts',(97.9554014775327,0.138553848385749,-4.47158362183291));
#39479=CARTESIAN_POINT('Ctrl Pts',(97.3933422344856,-1.1763308960171,-4.55058345768047));
#39480=CARTESIAN_POINT('Ctrl Pts',(95.9849839096634,-1.42403901591176,-4.62958329352804));
#39481=CARTESIAN_POINT('Ctrl Pts',(95.0080002326859,-0.379847760117011,
-4.7085831293756));
#39482=CARTESIAN_POINT('Ctrl Pts',(95.3487184658291,1.00894436592707,-4.78758296522316));
#39483=CARTESIAN_POINT('Ctrl Pts',(96.6980363529281,1.48241424175037,-4.86658280107073));
#39484=CARTESIAN_POINT('Ctrl Pts',(97.8318421130057,0.611026278686286,-4.94558263691828));
#39485=CARTESIAN_POINT('Ctrl Pts',(97.7215382587522,-0.814689521708318,
-5.02458247276585));
#39486=CARTESIAN_POINT('Ctrl Pts',(96.4671933127673,-1.50131259169636,-5.10358230861341));
#39487=CARTESIAN_POINT('Ctrl Pts',(95.2067588581957,-0.825933091350775,
-5.18258214446097));
#39488=CARTESIAN_POINT('Ctrl Pts',(95.0837109281827,0.598739394056823,-5.26158198030854));
#39489=CARTESIAN_POINT('Ctrl Pts',(96.2096795709132,1.48023080033689,-5.3405818161561));
#39490=CARTESIAN_POINT('Ctrl Pts',(97.5631771934661,1.01884520292257,-5.41958165200366));
#39491=CARTESIAN_POINT('Ctrl Pts',(97.9163001260439,-0.366844761768566,
-5.49858148785122));
#39492=CARTESIAN_POINT('Ctrl Pts',(96.9486924717633,-1.41973027840158,-5.57758132369879));
#39493=CARTESIAN_POINT('Ctrl Pts',(95.5381754914957,-1.18462533984329,-5.65658115954635));
#39494=CARTESIAN_POINT('Ctrl Pts',(94.9643812640292,0.125181007783859,-5.73558099539391));
#39495=CARTESIAN_POINT('Ctrl Pts',(95.747860417511,1.32142216232493,-5.81458083124147));
#39496=CARTESIAN_POINT('Ctrl Pts',(97.1778345126287,1.31885875641881,-5.89358066708904));
#39497=CARTESIAN_POINT('Ctrl Pts',(97.9570198232402,0.119816332029419,-5.9725805029366));
#39498=CARTESIAN_POINT('Ctrl Pts',(97.3785333179971,-1.18792440948235,-6.05158033878416));
#39499=CARTESIAN_POINT('Ctrl Pts',(95.9671824962854,-1.41797080004694,-6.13058017463173));
#39500=CARTESIAN_POINT('Ctrl Pts',(95.0033559043983,-0.361622947997633,
-6.20958001047928));
#39501=CARTESIAN_POINT('Ctrl Pts',(95.3614445937175,1.02279208165916,-6.28857984632685));
#39502=CARTESIAN_POINT('Ctrl Pts',(96.7165876938569,1.47932210466145,-6.36757968217441));
#39503=CARTESIAN_POINT('Ctrl Pts',(97.8393887448333,0.593799499820503,-6.44657951802197));
#39504=CARTESIAN_POINT('Ctrl Pts',(97.7112338178343,-0.830422673312564,
-6.52557935386954));
#39505=CARTESIAN_POINT('Ctrl Pts',(96.4483860688072,-1.50127887737916,-6.6045791897171));
#39506=CARTESIAN_POINT('Ctrl Pts',(95.1965108905739,-0.810163097005384,
-6.68357902556466));
#39507=CARTESIAN_POINT('Ctrl Pts',(95.0913192735848,0.615939005746443,-6.76257886141222));
#39508=CARTESIAN_POINT('Ctrl Pts',(96.2282418786556,1.48325640660785,-6.84157869725979));
#39509=CARTESIAN_POINT('Ctrl Pts',(97.5758535922281,1.00495195001113,-6.92057853310735));
#39510=CARTESIAN_POINT('Ctrl Pts',(97.9115904873431,-0.385052805742064,
-6.9995783689549));
#39511=CARTESIAN_POINT('Ctrl Pts',(96.9308694168058,-1.42573463298888,-7.07857820480248));
#39512=CARTESIAN_POINT('Ctrl Pts',(95.5234082356713,-1.17297880742125,-7.15757804065002));
#39513=CARTESIAN_POINT('Ctrl Pts',(94.9660667777636,0.143912601562404,-7.23657787649761));
#39514=CARTESIAN_POINT('Ctrl Pts',(95.7644695895102,1.33024536851806,-7.31557771234515));
#39515=CARTESIAN_POINT('Ctrl Pts',(97.1942993716535,1.30976909309513,-7.39457754819273));
#39516=CARTESIAN_POINT('Ctrl Pts',(97.958403319913,0.101060013121175,-7.47357738404029));
#39517=CARTESIAN_POINT('Ctrl Pts',(97.363580333275,-1.19933150420143,-7.55257721988785));
#39518=CARTESIAN_POINT('Ctrl Pts',(95.9494584953071,-1.41168006468811,-7.63157705573541));
#39519=CARTESIAN_POINT('Ctrl Pts',(94.9989402400067,-0.343341387068236,
-7.71057689158298));
#39520=CARTESIAN_POINT('Ctrl Pts',(95.3743431913168,1.03647929255094,-7.78957672743054));
#39521=CARTESIAN_POINT('Ctrl Pts',(96.7350988444355,1.47599782033385,-7.8685765632781));
#39522=CARTESIAN_POINT('Ctrl Pts',(97.8467189872506,0.576479537113928,-7.94757639912566));
#39523=CARTESIAN_POINT('Ctrl Pts',(97.7007330986187,-0.846025508245198,
-8.02657623497322));
#39524=CARTESIAN_POINT('Ctrl Pts',(96.429580722873,-1.50100957019055,-8.1055760708208));
#39525=CARTESIAN_POINT('Ctrl Pts',(95.1864612754006,-0.794265965281614,
-8.18457590666833));
#39526=CARTESIAN_POINT('Ctrl Pts',(95.0991424789539,0.633041959274281,-8.26357574251592));
#39527=CARTESIAN_POINT('Ctrl Pts',(96.2468406312449,1.48604924825804,-8.34257557836346));
#39528=CARTESIAN_POINT('Ctrl Pts',(97.5883549576452,0.990900991836843,-8.42157541421104));
#39529=CARTESIAN_POINT('Ctrl Pts',(97.9066531287706,-0.403200424021302,
-8.50057525005859));
#39530=CARTESIAN_POINT('Ctrl Pts',(96.9129725446261,-1.43151524987712,-8.57957508590616));
#39531=CARTESIAN_POINT('Ctrl Pts',(95.5087880329934,-1.16114820132636,-8.65857492175372));
#39532=CARTESIAN_POINT('Ctrl Pts',(94.9679868069389,0.162621610793496,-8.73757475760129));
#39533=CARTESIAN_POINT('Ctrl Pts',(95.7811879855942,1.33885982300962,-8.81657459344884));
#39534=CARTESIAN_POINT('Ctrl Pts',(97.2106490732843,1.30047388779886,-8.89557442929642));
#39535=CARTESIAN_POINT('Ctrl Pts',(97.9595517517141,0.0822878397116671,
-8.97457426514396));
#39536=CARTESIAN_POINT('Ctrl Pts',(97.3484856243634,-1.21055039923371,-9.05357410099154));
#39537=CARTESIAN_POINT('Ctrl Pts',(95.9318146930359,-1.40516777903702,-9.1325739368391));
#39538=CARTESIAN_POINT('Ctrl Pts',(94.9947539227958,-0.325005981583586,
-9.21157377268665));
#39539=CARTESIAN_POINT('Ctrl Pts',(95.3874122534566,1.05000392020451,-9.29057360853423));
#39540=CARTESIAN_POINT('Ctrl Pts',(96.7535668624323,1.47244177381299,-9.36957344438178));
#39541=CARTESIAN_POINT('Ctrl Pts',(97.8538317632754,0.559069377109707,-9.44857328022934));
#39542=CARTESIAN_POINT('Ctrl Pts',(97.69003760481,-0.86149610584715,-9.52757311607691));
#39543=CARTESIAN_POINT('Ctrl Pts',(96.4107805093987,-1.50050367483187,-9.60657295192447));
#39544=CARTESIAN_POINT('Ctrl Pts',(95.1766110328037,-0.778246230295927,
-9.68557278777204));
#39545=CARTESIAN_POINT('Ctrl Pts',(95.1071804113186,0.650049579330621,-9.76457262361959));
#39546=CARTESIAN_POINT('Ctrl Pts',(96.2654707582736,1.48860100773463,-9.84357245946716));
#39547=CARTESIAN_POINT('Ctrl Pts',(97.6006835573209,0.976710020754203,-9.92257229531473));
#39548=CARTESIAN_POINT('Ctrl Pts',(97.9014805118753,-0.421315210461393,
-10.0015721311623));
#39549=CARTESIAN_POINT('Ctrl Pts',(96.8950210040736,-1.43701138560673,-10.0805719670098));
#39550=CARTESIAN_POINT('Ctrl Pts',(95.49428506025,-1.14925299838305,-10.1595718028574));
#39551=CARTESIAN_POINT('Ctrl Pts',(94.9702041719499,0.181536371810648,-10.238571638705));
#39552=CARTESIAN_POINT('Ctrl Pts',(95.7978890002384,1.34680868945089,-10.3175714745525));
#39553=CARTESIAN_POINT('Ctrl Pts',(97.2271237476169,1.29188000504595,-10.3965713104001));
#39554=CARTESIAN_POINT('Ctrl Pts',(97.9600563880694,0.0615133851726164,
-10.4755773572309));
#39555=CARTESIAN_POINT('Ctrl Pts',(97.5425571034927,-0.790655940926349,
-10.5282501254459));
#39556=CARTESIAN_POINT('Ctrl Pts',(97.1998503478036,-1.03537583040079,-10.5545896150451));
#39557=CARTESIAN_POINT('Ctrl Pts',(97.0534702384955,1.23370347584956,0.0546651324586929));
#39558=CARTESIAN_POINT('Ctrl Pts',(97.4617196679856,1.03747517331684,0.0283318538428387));
#39559=CARTESIAN_POINT('Ctrl Pts',(98.0612652532588,0.21131356346982,-0.0243347033888694));
#39560=CARTESIAN_POINT('Ctrl Pts',(97.5114008735226,-1.22790933007582,-0.103334539236432));
#39561=CARTESIAN_POINT('Ctrl Pts',(96.0066113689587,-1.54978340369014,-0.182334375083995));
#39562=CARTESIAN_POINT('Ctrl Pts',(94.9143451713624,-0.467332802565443,
-0.261334210931557));
#39563=CARTESIAN_POINT('Ctrl Pts',(95.2243545783925,1.03991960823948,-0.340334046779121));
#39564=CARTESIAN_POINT('Ctrl Pts',(96.6559863729016,1.60332511996053,-0.419333882626682));
#39565=CARTESIAN_POINT('Ctrl Pts',(97.9101529558824,0.712396988494417,-0.498333718474245));
#39566=CARTESIAN_POINT('Ctrl Pts',(97.8492171766492,-0.824932913389202,
-0.577333554321806));
#39567=CARTESIAN_POINT('Ctrl Pts',(96.5283828065708,-1.61382142541515,-0.656333390169371));
#39568=CARTESIAN_POINT('Ctrl Pts',(95.1459606591299,-0.938666845162889,
-0.735333226016932));
#39569=CARTESIAN_POINT('Ctrl Pts',(94.9560748629476,0.588068102811137,-0.814333061864496));
#39570=CARTESIAN_POINT('Ctrl Pts',(96.1310015277402,1.58129570641339,-0.893332897712057));
#39571=CARTESIAN_POINT('Ctrl Pts',(97.6048327567796,1.13996316657112,-0.97233273355962));
#39572=CARTESIAN_POINT('Ctrl Pts',(98.0404999341466,-0.335554809072396,
-1.05133256940718));
#39573=CARTESIAN_POINT('Ctrl Pts',(97.0427610296164,-1.50665386027559,-1.13033240525474));
#39574=CARTESIAN_POINT('Ctrl Pts',(95.5167732958396,-1.31090519238855,-1.20933224110231));
#39575=CARTESIAN_POINT('Ctrl Pts',(94.8469244372853,0.0741072085732126,
-1.28833207694987));
#39576=CARTESIAN_POINT('Ctrl Pts',(95.6409067748658,1.39188884073063,-1.36733191279743));
#39577=CARTESIAN_POINT('Ctrl Pts',(97.178413207992,1.44693805333341,-1.44633174864499));
#39578=CARTESIAN_POINT('Ctrl Pts',(98.0646058751086,0.18931367074896,-1.52533158449256));
#39579=CARTESIAN_POINT('Ctrl Pts',(97.4955238075608,-1.24005754351337,-1.60433142034012));
#39580=CARTESIAN_POINT('Ctrl Pts',(95.9874427368982,-1.54443882685847,-1.68333125618768));
#39581=CARTESIAN_POINT('Ctrl Pts',(94.9085056446709,-0.447693076396299,
-1.76233109203524));
#39582=CARTESIAN_POINT('Ctrl Pts',(95.2375327350021,1.05520334570443,-1.84133092788281));
#39583=CARTESIAN_POINT('Ctrl Pts',(96.676028046713,1.60081100906409,-1.92033076373037));
#39584=CARTESIAN_POINT('Ctrl Pts',(97.918977339861,0.694150356097816,-1.99933059957793));
#39585=CARTESIAN_POINT('Ctrl Pts',(97.83876725662,-0.842248949561958,-2.07833043542549));
#39586=CARTESIAN_POINT('Ctrl Pts',(96.5081650144597,-1.61455339563897,-2.15733027127306));
#39587=CARTESIAN_POINT('Ctrl Pts',(95.1343034142239,-0.922122324891032,
-2.23633010712062));
#39588=CARTESIAN_POINT('Ctrl Pts',(94.9635604862002,0.606865358751896,-2.31532994296818));
#39589=CARTESIAN_POINT('Ctrl Pts',(96.1508355552055,1.5853000243166,-2.39432977881574));
#39590=CARTESIAN_POINT('Ctrl Pts',(97.6190233570862,1.12553806126023,-2.47332961466331));
#39591=CARTESIAN_POINT('Ctrl Pts',(98.0361723908918,-0.355320867821741,
-2.55232945051087));
#39592=CARTESIAN_POINT('Ctrl Pts',(97.0238417780262,-1.51382991591343,-2.63132928635843));
#39593=CARTESIAN_POINT('Ctrl Pts',(95.5004257985166,-1.2989805788641,-2.71032912220599));
#39594=CARTESIAN_POINT('Ctrl Pts',(94.8479793896609,0.0943141379221071,
-2.78932895805356));
#39595=CARTESIAN_POINT('Ctrl Pts',(95.6584070560774,1.40204632830397,-2.86832879390112));
#39596=CARTESIAN_POINT('Ctrl Pts',(97.1964824559416,1.43783108186362,-2.94732862974868));
#39597=CARTESIAN_POINT('Ctrl Pts',(98.0668515107163,0.16920418921777,-3.02632846559624));
#39598=CARTESIAN_POINT('Ctrl Pts',(97.4799085804449,-1.25292607234706,-3.10532830144381));
#39599=CARTESIAN_POINT('Ctrl Pts',(95.9681328996918,-1.53839196407101,-3.18432813729137));
#39600=CARTESIAN_POINT('Ctrl Pts',(94.9030192353312,-0.428216587724458,
-3.26332797313893));
#39601=CARTESIAN_POINT('Ctrl Pts',(95.2508470661204,1.07044023903157,-3.34232780898649));
#39602=CARTESIAN_POINT('Ctrl Pts',(96.6960642530924,1.59798527666832,-3.42132764483406));
#39603=CARTESIAN_POINT('Ctrl Pts',(97.9275584174969,0.675825525165635,-3.50032748068162));
#39604=CARTESIAN_POINT('Ctrl Pts',(97.8281083846458,-0.859448448827256,
-3.57932731652918));
#39605=CARTESIAN_POINT('Ctrl Pts',(96.4879360051457,-1.61502404231877,-3.65832715237675));
#39606=CARTESIAN_POINT('Ctrl Pts',(95.1228561836784,-0.905437144697542,
-3.7373269882243));
#39607=CARTESIAN_POINT('Ctrl Pts',(94.9712800518301,0.625569439386297,-3.81632682407187));
#39608=CARTESIAN_POINT('Ctrl Pts',(96.1707186664732,1.58905451657091,-3.89532665991943));
#39609=CARTESIAN_POINT('Ctrl Pts',(97.6330318993376,1.11093686029388,-3.97432649576699));
#39610=CARTESIAN_POINT('Ctrl Pts',(98.0315977046149,-0.375031437859765,
-4.05332633161456));
#39611=CARTESIAN_POINT('Ctrl Pts',(97.0048340545268,-1.5207682711299,-4.13232616746212));
#39612=CARTESIAN_POINT('Ctrl Pts',(95.4842289937883,-1.28685218893334,-4.21132600330968));
#39613=CARTESIAN_POINT('Ctrl Pts',(94.8492873721174,0.114506302432829,-4.29032583915724));
#39614=CARTESIAN_POINT('Ctrl Pts',(95.6760332137652,1.41198377721691,-4.36932567500481));
#39615=CARTESIAN_POINT('Ctrl Pts',(97.2144362002192,1.42849848350396,-4.44832551085237));
#39616=CARTESIAN_POINT('Ctrl Pts',(98.0688450638164,0.149068150089657,-4.52732534669993));
#39617=CARTESIAN_POINT('Ctrl Pts',(97.464133375343,-1.26559797945395,-4.60632518254749));
#39618=CARTESIAN_POINT('Ctrl Pts',(95.9489003263115,-1.53210368553927,-4.68532501839506));
#39619=CARTESIAN_POINT('Ctrl Pts',(94.8977772352419,-0.408672899208807,
-4.76432485424261));
#39620=CARTESIAN_POINT('Ctrl Pts',(95.2643512229599,1.0855091498678,-4.84332469009019));
#39621=CARTESIAN_POINT('Ctrl Pts',(96.7160634897512,1.59490877560504,-4.92232452593774));
#39622=CARTESIAN_POINT('Ctrl Pts',(97.93590926946,0.657394638121783,-5.00132436178531));
#39623=CARTESIAN_POINT('Ctrl Pts',(97.8172348934474,-0.876513076420429,
-5.08032419763286));
#39624=CARTESIAN_POINT('Ctrl Pts',(96.4677026873718,-1.61524124633046,-5.15932403348044));
#39625=CARTESIAN_POINT('Ctrl Pts',(95.1116188640692,-0.888609875943022,
-5.23832386932799));
#39626=CARTESIAN_POINT('Ctrl Pts',(94.9792333149623,0.644175350578207,-5.31732370517556));
#39627=CARTESIAN_POINT('Ctrl Pts',(96.1906472495902,1.59255964148767,-5.39632354102312));
#39628=CARTESIAN_POINT('Ctrl Pts',(97.6468564353717,1.09616132209147,-5.47532337687068));
#39629=CARTESIAN_POINT('Ctrl Pts',(98.0267764659365,-0.394683154918008,
-5.55432321271824));
#39630=CARTESIAN_POINT('Ctrl Pts',(96.9857409067177,-1.52746797503865,-5.6333230485658));
#39631=CARTESIAN_POINT('Ctrl Pts',(95.4681853904451,-1.27452185570567,-5.71232288441337));
#39632=CARTESIAN_POINT('Ctrl Pts',(94.8508481961557,0.134680497684516,-5.79132272026093));
#39633=CARTESIAN_POINT('Ctrl Pts',(95.6937824733625,1.42169964616808,-5.8703225561085));
#39634=CARTESIAN_POINT('Ctrl Pts',(97.2322716277157,1.41894171356061,-5.94932239195605));
#39635=CARTESIAN_POINT('Ctrl Pts',(98.070586219357,0.128908717976762,-6.02832222780363));
#39636=CARTESIAN_POINT('Ctrl Pts',(97.4482006689514,-1.27807127864728,-6.10732206365118));
#39637=CARTESIAN_POINT('Ctrl Pts',(95.9297480343168,-1.52557497685415,-6.18632189949874));
#39638=CARTESIAN_POINT('Ctrl Pts',(94.8927804673116,-0.389065078422743,
-6.26532173534631));
#39639=CARTESIAN_POINT('Ctrl Pts',(95.2780430861903,1.10040771379221,-6.34432157119387));
#39640=CARTESIAN_POINT('Ctrl Pts',(96.7360226183224,1.59158198850359,-6.42332140704143));
#39641=CARTESIAN_POINT('Ctrl Pts',(97.9440285852282,0.638860587372241,-6.50232124288899));
#39642=CARTESIAN_POINT('Ctrl Pts',(97.8061484894015,-0.893440154463006,
-6.58132107873655));
#39643=CARTESIAN_POINT('Ctrl Pts',(96.4474682363038,-1.61520497356751,-6.66032091458412));
#39644=CARTESIAN_POINT('Ctrl Pts',(95.1005932188536,-0.871643159309884,
-6.73932075043168));
#39645=CARTESIAN_POINT('Ctrl Pts',(94.9874190275034,0.6626801725424,-6.81832058627924));
#39646=CARTESIAN_POINT('Ctrl Pts',(96.2106181772027,1.59581484901143,-6.89732042212681));
#39647=CARTESIAN_POINT('Ctrl Pts',(97.6604947957295,1.08121376535188,-6.97632025797437));
#39648=CARTESIAN_POINT('Ctrl Pts',(98.0217094314449,-0.414272935090146,
-7.05532009382193));
#39649=CARTESIAN_POINT('Ctrl Pts',(96.9665653308501,-1.53392797626733,-7.1343199296695));
#39650=CARTESIAN_POINT('Ctrl Pts',(95.4522975061803,-1.2619915141573,-7.21331976551705));
#39651=CARTESIAN_POINT('Ctrl Pts',(94.8526616168382,0.154833557778703,-7.29231960136462));
#39652=CARTESIAN_POINT('Ctrl Pts',(95.7116520495115,1.43119241046437,-7.37131943721218));
#39653=CARTESIAN_POINT('Ctrl Pts',(97.2499859395508,1.40916227175958,-7.45031927305975));
#39654=CARTESIAN_POINT('Ctrl Pts',(98.0720747041024,0.108729056460906,-7.5293191089073));
#39655=CARTESIAN_POINT('Ctrl Pts',(97.4321129615595,-1.29034401251561,-7.60831894475487));
#39656=CARTESIAN_POINT('Ctrl Pts',(95.9106790292421,-1.51880686255369,-7.68731878060243));
#39657=CARTESIAN_POINT('Ctrl Pts',(94.8880297156727,-0.369396202384675,
-7.76631861644999));
#39658=CARTESIAN_POINT('Ctrl Pts',(95.2919205071734,1.11513359280096,-7.84531845229756));
#39659=CARTESIAN_POINT('Ctrl Pts',(96.7559385066569,1.58800543743075,-7.92431828814511));
#39660=CARTESIAN_POINT('Ctrl Pts',(97.9519150906526,0.620226281430028,-8.00331812399269));
#39661=CARTESIAN_POINT('Ctrl Pts',(97.7948509122765,-0.910227026618923,
-8.08231795984023));
#39662=CARTESIAN_POINT('Ctrl Pts',(96.427235827296,-1.61491522972511,-8.16131779568782));
#39663=CARTESIAN_POINT('Ctrl Pts',(95.0897809782665,-0.854539657347264,
-8.24031763153535));
#39664=CARTESIAN_POINT('Ctrl Pts',(94.9958359048817,0.681081001340498,-8.31931746738295));
#39665=CARTESIAN_POINT('Ctrl Pts',(96.2306283153171,1.59881962833109,-8.39831730323048));
#39666=CARTESIAN_POINT('Ctrl Pts',(97.6739448401565,1.06609653572288,-8.47731713907807));
#39667=CARTESIAN_POINT('Ctrl Pts',(98.0163973963242,-0.433797704101884,
-8.55631697492561));
#39668=CARTESIAN_POINT('Ctrl Pts',(96.9473103360644,-1.54014726123087,-8.63531681077318));
#39669=CARTESIAN_POINT('Ctrl Pts',(95.4365678343412,-1.24926313031556,-8.71431664662074));
#39670=CARTESIAN_POINT('Ctrl Pts',(94.8547273494079,0.174962319473753,-8.7933164824683));
#39671=CARTESIAN_POINT('Ctrl Pts',(95.7296391383274,1.44046058172089,-8.87231631831587));
#39672=CARTESIAN_POINT('Ctrl Pts',(97.2675763551547,1.39916169022134,-8.95131615416344));
#39673=CARTESIAN_POINT('Ctrl Pts',(98.0733102858353,0.088532337308607,-9.03031599001099));
#39674=CARTESIAN_POINT('Ctrl Pts',(97.4158727750917,-1.30241426496977,-9.10931582585856));
#39675=CARTESIAN_POINT('Ctrl Pts',(95.8916963088359,-1.51180038538851,-9.18831566170613));
#39676=CARTESIAN_POINT('Ctrl Pts',(94.8835257154617,-0.349669395741739,
-9.26731549755368));
#39677=CARTESIAN_POINT('Ctrl Pts',(95.3059813285748,1.12968455077475,-9.34631533340124));
#39678=CARTESIAN_POINT('Ctrl Pts',(96.775807989249,1.58417953665158,-9.42531516924881));
#39679=CARTESIAN_POINT('Ctrl Pts',(97.959567627023,0.601494933475199,-9.50431500509637));
#39680=CARTESIAN_POINT('Ctrl Pts',(97.7833437798875,-0.926871626477916,
-9.58331484094394));
#39681=CARTESIAN_POINT('Ctrl Pts',(96.4070089402296,-1.61437094397529,-9.66231467679148));
#39682=CARTESIAN_POINT('Ctrl Pts',(95.0791832398496,-0.837304248247735,
-9.74131451263906));
#39683=CARTESIAN_POINT('Ctrl Pts',(95.004483804035,0.699379262188282,-9.8203143484866));
#39684=CARTESIAN_POINT('Ctrl Pts',(96.2506722087523,1.6015650307077,-9.89931418433419));
#39685=CARTESIAN_POINT('Ctrl Pts',(97.6872090083356,1.05082866816156,-9.97831402018174));
#39686=CARTESIAN_POINT('Ctrl Pts',(98.0108322500603,-0.453287149796495,
-10.0573138560293));
#39687=CARTESIAN_POINT('Ctrl Pts',(96.9279965243397,-1.54606047688962,-10.1363136918769));
#39688=CARTESIAN_POINT('Ctrl Pts',(95.4209642885513,-1.23646524762692,-10.2153135277244));
#39689=CARTESIAN_POINT('Ctrl Pts',(94.85711298145,0.195312446641386,-10.294313363572));
#39690=CARTESIAN_POINT('Ctrl Pts',(95.747607526695,1.44901265609136,-10.3733131994195));
#39691=CARTESIAN_POINT('Ctrl Pts',(97.2853012271431,1.38991565181107,-10.4523130352671));
#39692=CARTESIAN_POINT('Ctrl Pts',(98.0738532170406,0.0661813918578819,
-10.5313190820979));
#39693=CARTESIAN_POINT('Ctrl Pts',(97.6246715686008,-0.850655682570031,
-10.583991850313));
#39694=CARTESIAN_POINT('Ctrl Pts',(97.2559581572523,-1.11394639328732,-10.6103313399122));
#39695=CARTESIAN_POINT('Ctrl Pts',(97.0952958617901,1.3207209276019,-0.00107659240832891));
#39696=CARTESIAN_POINT('Ctrl Pts',(97.5323405615611,1.1106519516964,-0.027409871024183));
#39697=CARTESIAN_POINT('Ctrl Pts',(98.1741742088046,0.226218253432855,-0.0800764282558911));
#39698=CARTESIAN_POINT('Ctrl Pts',(97.5855259575219,-1.31451810031743,-0.159076264103454));
#39699=CARTESIAN_POINT('Ctrl Pts',(95.9745983487262,-1.65909508611393,-0.238076099951017));
#39700=CARTESIAN_POINT('Ctrl Pts',(94.8052907688116,-0.500295431264796,
-0.317075935798579));
#39701=CARTESIAN_POINT('Ctrl Pts',(95.1371662312978,1.11326880122442,-0.396075771646142));
#39702=CARTESIAN_POINT('Ctrl Pts',(96.6697760590574,1.71641328822836,-0.475075607493704));
#39703=CARTESIAN_POINT('Ctrl Pts',(98.012403428816,0.762644857442132,-0.554075443341267));
#39704=CARTESIAN_POINT('Ctrl Pts',(97.9471696344331,-0.883118337516605,
-0.633075279188829));
#39705=CARTESIAN_POINT('Ctrl Pts',(96.5331721637222,-1.72764993507891,-0.712075115036392));
#39706=CARTESIAN_POINT('Ctrl Pts',(95.0532429127743,-1.00487432411502,-0.791074950883953));
#39707=CARTESIAN_POINT('Ctrl Pts',(94.8499638025334,0.629546617515179,-0.870074786731518));
#39708=CARTESIAN_POINT('Ctrl Pts',(96.1077621835587,1.69283006254727,-0.949074622579079));
#39709=CARTESIAN_POINT('Ctrl Pts',(97.6855479206097,1.22036878411891,-1.02807445842664));
#39710=CARTESIAN_POINT('Ctrl Pts',(98.1519442385918,-0.359222671715493,
-1.1070742942742));
#39711=CARTESIAN_POINT('Ctrl Pts',(97.0838312946866,-1.61292346408271,-1.18607413012177));
#39712=CARTESIAN_POINT('Ctrl Pts',(95.4502102709029,-1.40336795314393,-1.26507396596933));
#39713=CARTESIAN_POINT('Ctrl Pts',(94.7331146128772,0.0793342510293227,
-1.34407380181689));
#39714=CARTESIAN_POINT('Ctrl Pts',(95.5830993214529,1.49006366346062,-1.42307363766445));
#39715=CARTESIAN_POINT('Ctrl Pts',(97.2290514990247,1.54899569093378,-1.50207347351202));
#39716=CARTESIAN_POINT('Ctrl Pts',(98.1777504564805,0.202666630785906,-1.58107330935958));
#39717=CARTESIAN_POINT('Ctrl Pts',(97.5685290261725,-1.32752317003962,-1.66007314520714));
#39718=CARTESIAN_POINT('Ctrl Pts',(95.9540776855269,-1.65337353745256,-1.7390729810547));
#39719=CARTESIAN_POINT('Ctrl Pts',(94.7990393597335,-0.479270446029912,
-1.81807281690227));
#39720=CARTESIAN_POINT('Ctrl Pts',(95.1512738897119,1.12963055452827,-1.89707265274983));
#39721=CARTESIAN_POINT('Ctrl Pts',(96.6912313427176,1.71372184823468,-1.97607248859739));
#39722=CARTESIAN_POINT('Ctrl Pts',(98.0218502276797,0.743111225790608,-2.05507232444495));
#39723=CARTESIAN_POINT('Ctrl Pts',(97.9359826447353,-0.90165573471468,-2.13407216029252));
#39724=CARTESIAN_POINT('Ctrl Pts',(96.5115283395184,-1.7284335337409,-2.21307199614008));
#39725=CARTESIAN_POINT('Ctrl Pts',(95.0407634413237,-0.987162860551926,
-2.29207183198764));
#39726=CARTESIAN_POINT('Ctrl Pts',(94.8579774131613,0.649669710128945,-2.37107166783521));
#39727=CARTESIAN_POINT('Ctrl Pts',(96.1289951748448,1.69711681909701,-2.45007150368276));
#39728=CARTESIAN_POINT('Ctrl Pts',(97.7007394339408,1.20492622531942,-2.52907133953033));
#39729=CARTESIAN_POINT('Ctrl Pts',(98.147311458468,-0.38038290021245,-2.60807117537789));
#39730=CARTESIAN_POINT('Ctrl Pts',(97.0635776016403,-1.62060567220166,-2.68707101122545));
#39731=CARTESIAN_POINT('Ctrl Pts',(95.4327097270115,-1.39060225462431,-2.76607084707302));
#39732=CARTESIAN_POINT('Ctrl Pts',(94.7342439747597,0.100966446282139,-2.84507068292058));
#39733=CARTESIAN_POINT('Ctrl Pts',(95.6018339591418,1.50093759441126,-2.92407051876814));
#39734=CARTESIAN_POINT('Ctrl Pts',(97.248395234679,1.5392463726878,-3.0030703546157));
#39735=CARTESIAN_POINT('Ctrl Pts',(98.1801544846778,0.181138756688628,-3.08207019046326));
#39736=CARTESIAN_POINT('Ctrl Pts',(97.5518124020847,-1.34129936154011,-3.16107002631083));
#39737=CARTESIAN_POINT('Ctrl Pts',(95.9334058574854,-1.64690016813321,-3.24006986215839));
#39738=CARTESIAN_POINT('Ctrl Pts',(94.7931659746178,-0.458420212008008,
-3.31906969800596));
#39739=CARTESIAN_POINT('Ctrl Pts',(95.1655273275025,1.14594215961223,-3.39806953385351));
#39740=CARTESIAN_POINT('Ctrl Pts',(96.7126807733086,1.71069680697967,-3.47706936970108));
#39741=CARTESIAN_POINT('Ctrl Pts',(98.0310365589472,0.723493879985343,-3.55606920554864));
#39742=CARTESIAN_POINT('Ctrl Pts',(97.9245719649759,-0.920068375246725,
-3.63506904139621));
#39743=CARTESIAN_POINT('Ctrl Pts',(96.4898725069229,-1.72893737678884,-3.71406887724376));
#39744=CARTESIAN_POINT('Ctrl Pts',(95.028508797286,-0.969300815827463,-3.79306871309133));
#39745=CARTESIAN_POINT('Ctrl Pts',(94.8662414669465,0.6696930554538,-3.87206854893889));
#39746=CARTESIAN_POINT('Ctrl Pts',(96.1502807119863,1.70113612891485,-3.95106838478645));
#39747=CARTESIAN_POINT('Ctrl Pts',(97.715736048021,1.18929515021761,-4.03006822063402));
#39748=CARTESIAN_POINT('Ctrl Pts',(98.1424141034539,-0.401483726183824,
-4.10906805648158));
#39749=CARTESIAN_POINT('Ctrl Pts',(97.0432291964499,-1.62803341405123,-4.18806789232914));
#39750=CARTESIAN_POINT('Ctrl Pts',(95.4153705045938,-1.37761840663066,-4.26706772817671));
#39751=CARTESIAN_POINT('Ctrl Pts',(94.7356442138263,0.122582835280742,-4.34606756402426));
#39752=CARTESIAN_POINT('Ctrl Pts',(95.6207033518175,1.51157596659972,-4.42506739987183));
#39753=CARTESIAN_POINT('Ctrl Pts',(97.2676153197811,1.52925551329267,-4.50406723571939));
#39754=CARTESIAN_POINT('Ctrl Pts',(98.1822886501,0.159582451793565,-4.58306707156695));
#39755=CARTESIAN_POINT('Ctrl Pts',(97.5349245162006,-1.35486506289079,-4.66206690741451));
#39756=CARTESIAN_POINT('Ctrl Pts',(95.9128167429594,-1.64016835516679,-4.74106674326208));
#39757=CARTESIAN_POINT('Ctrl Pts',(94.7875542377978,-0.437498038300601,
-4.82006657910964));
#39758=CARTESIAN_POINT('Ctrl Pts',(95.1799839800908,1.16207393380852,-4.8990664149572));
#39759=CARTESIAN_POINT('Ctrl Pts',(96.7340906265743,1.70740330945973,-4.97806625080476));
#39760=CARTESIAN_POINT('Ctrl Pts',(98.0399764259145,0.703762997557278,-5.05706608665234));
#39761=CARTESIAN_POINT('Ctrl Pts',(97.9129315281424,-0.938336631132538,
-5.13606592249989));
#39762=CARTESIAN_POINT('Ctrl Pts',(96.4682120619765,-1.72916990096455,-5.21506575834745));
#39763=CARTESIAN_POINT('Ctrl Pts',(95.0164788699425,-0.951286660535266,
-5.29406559419502));
#39764=CARTESIAN_POINT('Ctrl Pts',(94.8747557017422,0.689611307099592,-5.37306543004258));
#39765=CARTESIAN_POINT('Ctrl Pts',(96.171614928267,1.70488848263846,-5.45206526589014));
#39766=CARTESIAN_POINT('Ctrl Pts',(97.7305356772772,1.17347744126039,-5.5310651017377));
#39767=CARTESIAN_POINT('Ctrl Pts',(98.1372528058293,-0.422521548067451,
-5.61006493758527));
#39768=CARTESIAN_POINT('Ctrl Pts',(97.0227893416717,-1.6352056716757,-5.68906477343282));
#39769=CARTESIAN_POINT('Ctrl Pts',(95.3981952893951,-1.36441837156804,-5.76806460928039));
#39770=CARTESIAN_POINT('Ctrl Pts',(94.7373151282815,0.144179987585173,-5.84706444512795));
#39771=CARTESIAN_POINT('Ctrl Pts',(95.6397045292144,1.52197713001124,-5.92606428097553));
#39772=CARTESIAN_POINT('Ctrl Pts',(97.2867087428023,1.51902467070241,-6.00506411682307));
#39773=CARTESIAN_POINT('Ctrl Pts',(98.1841526154742,0.138001103924106,-6.08406395267065));
#39774=CARTESIAN_POINT('Ctrl Pts',(97.5178680199056,-1.36821814781222,-6.1630637885182));
#39775=CARTESIAN_POINT('Ctrl Pts',(95.8923135723485,-1.63317915366136,-6.24206362436576));
#39776=CARTESIAN_POINT('Ctrl Pts',(94.7822050302246,-0.416507208847854,
-6.32106346021333));
#39777=CARTESIAN_POINT('Ctrl Pts',(95.1946415786631,1.17802334592527,-6.40006329606089));
#39778=CARTESIAN_POINT('Ctrl Pts',(96.7554575427877,1.70384187234572,-6.47906313190846));
#39779=CARTESIAN_POINT('Ctrl Pts',(98.0486684256232,0.683921674923979,-6.55806296775601));
#39780=CARTESIAN_POINT('Ctrl Pts',(97.9010631609685,-0.956457635613447,
-6.63706280360359));
#39781=CARTESIAN_POINT('Ctrl Pts',(96.4465504038007,-1.72913106975587,-6.71606263945113));
#39782=CARTESIAN_POINT('Ctrl Pts',(95.0046755471332,-0.933123221614384,
-6.79506247529871));
#39783=CARTESIAN_POINT('Ctrl Pts',(94.883518781422,0.709421339338357,-6.87406231114626));
#39784=CARTESIAN_POINT('Ctrl Pts',(96.1929944757499,1.70837329141502,-6.95306214699383));
#39785=CARTESIAN_POINT('Ctrl Pts',(97.7451359992307,1.15747558069262,-7.03206198284139));
#39786=CARTESIAN_POINT('Ctrl Pts',(98.1318283755469,-0.443493064438228,
-7.11106181868895));
#39787=CARTESIAN_POINT('Ctrl Pts',(97.0022612448941,-1.64212131954578,-7.19006165453652));
#39788=CARTESIAN_POINT('Ctrl Pts',(95.3811867766894,-1.35100422089335,-7.26906149038407));
#39789=CARTESIAN_POINT('Ctrl Pts',(94.7392564559124,0.165754513994999,-7.34806132623165));
#39790=CARTESIAN_POINT('Ctrl Pts',(95.658834509513,1.53213945241069,-7.4270611620792));
#39791=CARTESIAN_POINT('Ctrl Pts',(97.3056725074482,1.50855545042403,-7.50606099792676));
#39792=CARTESIAN_POINT('Ctrl Pts',(98.1857460882916,0.116398099800639,-7.58506083377433));
#39793=CARTESIAN_POINT('Ctrl Pts',(97.500645589844,-1.3813565208298,-7.66406066962188));
#39794=CARTESIAN_POINT('Ctrl Pts',(95.871899563177,-1.62593366041925,-7.74306050546945));
#39795=CARTESIAN_POINT('Ctrl Pts',(94.7771191913385,-0.395451017701117,
-7.82206034131702));
#39796=CARTESIAN_POINT('Ctrl Pts',(95.2094978230301,1.19378789305098,-7.90106017716457));
#39797=CARTESIAN_POINT('Ctrl Pts',(96.7767781688782,1.70001305452767,-7.98006001301215));
#39798=CARTESIAN_POINT('Ctrl Pts',(98.0571111940546,0.663973025746128,-8.05905984885969));
#39799=CARTESIAN_POINT('Ctrl Pts',(97.8889687259342,-0.974428544992647,
-8.13805968470727));
#39800=CARTESIAN_POINT('Ctrl Pts',(96.4248909317188,-1.72882088925967,-8.21705952055483));
#39801=CARTESIAN_POINT('Ctrl Pts',(94.9931006811322,-0.914813349412916,
-8.29605935640239));
#39802=CARTESIAN_POINT('Ctrl Pts',(94.8925293308096,0.729120043406717,-8.37505919224995));
#39803=CARTESIAN_POINT('Ctrl Pts',(96.2144159993889,1.71159000840414,-8.45405902809752));
#39804=CARTESIAN_POINT('Ctrl Pts',(97.7595347226678,1.14129207960892,-8.53305886394508));
#39805=CARTESIAN_POINT('Ctrl Pts',(98.1261416638778,-0.464394984182465,
-8.61205869979263));
#39806=CARTESIAN_POINT('Ctrl Pts',(96.9816481275025,-1.64877927258462,-8.69105853564022));
#39807=CARTESIAN_POINT('Ctrl Pts',(95.3643476356891,-1.33737805930476,-8.77005837148776));
#39808=CARTESIAN_POINT('Ctrl Pts',(94.741467891877,0.187303028154009,-8.84905820733534));
#39809=CARTESIAN_POINT('Ctrl Pts',(95.6780902910606,1.54206134043216,-8.92805804318289));
#39810=CARTESIAN_POINT('Ctrl Pts',(97.3245036370254,1.49784949264381,-9.00705787903045));
#39811=CARTESIAN_POINT('Ctrl Pts',(98.187068819956,0.0947768349055472,-9.08605771487802));
#39812=CARTESIAN_POINT('Ctrl Pts',(97.4832599258204,-1.39427813070584,-9.16505755072557));
#39813=CARTESIAN_POINT('Ctrl Pts',(95.8515779246356,-1.61843299173998,-9.24405738657315));
#39814=CARTESIAN_POINT('Ctrl Pts',(94.7722975081282,-0.374332809899895,
-9.32305722242069));
#39815=CARTESIAN_POINT('Ctrl Pts',(95.2245504036924,1.209365181345,-9.40205705826827));
#39816=CARTESIAN_POINT('Ctrl Pts',(96.7980491160662,1.69591729949016,-9.48105689411583));
#39817=CARTESIAN_POINT('Ctrl Pts',(98.0653034907704,0.643920489840692,-9.56005672996339));
#39818=CARTESIAN_POINT('Ctrl Pts',(97.8766499549651,-0.992247147108681,
-9.63905656581095));
#39819=CARTESIAN_POINT('Ctrl Pts',(96.4032373710603,-1.72823821311873,-9.71805640165851));
#39820=CARTESIAN_POINT('Ctrl Pts',(94.9817554468956,-0.896362266199541,
-9.79705623750608));
#39821=CARTESIAN_POINT('Ctrl Pts',(94.9017871967514,0.748708945045941,-9.87605607335364));
#39822=CARTESIAN_POINT('Ctrl Pts',(96.2358736592311,1.71452905368079,-9.9550559092012));
#39823=CARTESIAN_POINT('Ctrl Pts',(97.7737344593502,1.12494731556893,-10.0340557450487));
#39824=CARTESIAN_POINT('Ctrl Pts',(98.1201839882452,-0.485259089131598,
-10.1130555808963));
#39825=CARTESIAN_POINT('Ctrl Pts',(96.9609720446059,-1.65510956817251,-10.1920554167438));
#39826=CARTESIAN_POINT('Ctrl Pts',(95.3476435168528,-1.32367749687079,-10.2710552525914));
#39827=CARTESIAN_POINT('Ctrl Pts',(94.74402179095,0.209088521472124,-10.350055088439));
#39828=CARTESIAN_POINT('Ctrl Pts',(95.6973260531519,1.55121662273183,-10.4290549242865));
#39829=CARTESIAN_POINT('Ctrl Pts',(97.343478706669,1.48795129857621,-10.5080547601341));
#39830=CARTESIAN_POINT('Ctrl Pts',(98.187650046012,0.0708493985431469,-10.587060806965));
#39831=CARTESIAN_POINT('Ctrl Pts',(97.706786033709,-0.910655424213715,-10.6397335751801));
#39832=CARTESIAN_POINT('Ctrl Pts',(97.3120659667008,-1.19251695617385,-10.6660730647792));
#39833=CARTESIAN_POINT('Ctrl Pts',(97.0960530345221,1.32073705981523,-10.5));
#39834=CARTESIAN_POINT('Ctrl Pts',(97.1327523794304,1.29890511060011,-10.5));
#39835=CARTESIAN_POINT('Ctrl Pts',(97.1683327868718,1.27542981429671,-10.5));
#39836=CARTESIAN_POINT('Ctrl Pts',(97.2026700353434,1.25031220514833,-10.5));
#39837=CARTESIAN_POINT('Ctrl Pts',(97.2492821414819,1.2162155691137,-10.5));
#39838=CARTESIAN_POINT('Ctrl Pts',(97.2936053051564,1.17909352994033,-10.5));
#39839=CARTESIAN_POINT('Ctrl Pts',(97.3355049529323,1.1392708471789,-10.5));
#39840=CARTESIAN_POINT('Ctrl Pts',(97.3718456384346,1.10473156900102,-10.5));
#39841=CARTESIAN_POINT('Ctrl Pts',(97.406362784151,1.06815959411897,-10.5));
#39842=CARTESIAN_POINT('Ctrl Pts',(97.4389410516463,1.0297508894014,-10.5));
#39843=CARTESIAN_POINT('Ctrl Pts',(97.4537854365593,1.01224984834946,-10.5));
#39844=CARTESIAN_POINT('Ctrl Pts',(97.4682268999763,0.99436732143761,-10.5));
#39845=CARTESIAN_POINT('Ctrl Pts',(97.482252575178,0.976121347465687,-10.5));
#39846=CARTESIAN_POINT('Ctrl Pts',(97.4887615062686,0.967653891492528,-10.5));
#39847=CARTESIAN_POINT('Ctrl Pts',(97.4951808738737,0.959108159795724,-10.5));
#39848=CARTESIAN_POINT('Ctrl Pts',(97.5015092969713,0.950485946835754,-10.5));
#39849=CARTESIAN_POINT('Ctrl Pts',(97.5079891070103,0.941657475471821,-10.5));
#39850=CARTESIAN_POINT('Ctrl Pts',(97.514369012319,0.932754939898317,-10.5));
#39851=CARTESIAN_POINT('Ctrl Pts',(97.5206439889312,0.923786412192149,-10.5));
#39852=CARTESIAN_POINT('Ctrl Pts',(97.5532336246143,0.877207585110972,-10.5));
#39853=CARTESIAN_POINT('Ctrl Pts',(97.5830328074137,0.828801651694975,-10.5));
#39854=CARTESIAN_POINT('Ctrl Pts',(97.6099076639557,0.778871925525369,-10.5));
#39855=CARTESIAN_POINT('Ctrl Pts',(97.6363426534309,0.729759410869599,-10.5));
#39856=CARTESIAN_POINT('Ctrl Pts',(97.6599484872081,0.679171459866346,-10.5));
#39857=CARTESIAN_POINT('Ctrl Pts',(97.6805502395513,0.627383924127521,-10.5));
#39858=CARTESIAN_POINT('Ctrl Pts',(97.6987863703601,0.58154295583198,-10.5));
#39859=CARTESIAN_POINT('Ctrl Pts',(97.7146681957523,0.534761436162482,-10.5));
#39860=CARTESIAN_POINT('Ctrl Pts',(97.728040262327,0.487232253208875,-10.5));
#39861=CARTESIAN_POINT('Ctrl Pts',(97.7323205078086,0.472018705665731,-10.5));
#39862=CARTESIAN_POINT('Ctrl Pts',(97.7363446754649,0.456722195966646,-10.5));
#39863=CARTESIAN_POINT('Ctrl Pts',(97.7400979971882,0.441388713975437,-10.5));
#39864=CARTESIAN_POINT('Ctrl Pts',(97.7528828129849,0.389158780803246,-10.5));
#39865=CARTESIAN_POINT('Ctrl Pts',(97.7625536024157,0.336421827194652,-10.5));
#39866=CARTESIAN_POINT('Ctrl Pts',(97.7689618062189,0.283432905893329,-10.5));
#39867=CARTESIAN_POINT('Ctrl Pts',(97.7751646173992,0.232142359654773,-10.5));
#39868=CARTESIAN_POINT('Ctrl Pts',(97.7783106242714,0.180614917104041,-10.5));
#39869=CARTESIAN_POINT('Ctrl Pts',(97.7782188386079,0.129087102186097,-10.5));
#39870=CARTESIAN_POINT('Ctrl Pts',(97.7781750834699,0.104523280682375,-10.5));
#39871=CARTESIAN_POINT('Ctrl Pts',(97.7773948438647,0.0799595271486894,
-10.5));
#39872=CARTESIAN_POINT('Ctrl Pts',(97.7758546340163,0.0554226938714613,
-10.5));
#39873=CARTESIAN_POINT('Ctrl Pts',(97.7740586174852,0.0268106458234052,
-10.5));
#39874=CARTESIAN_POINT('Ctrl Pts',(97.7712292013864,-0.00176488002858206,
-10.5));
#39875=CARTESIAN_POINT('Ctrl Pts',(97.7673856184957,-0.0302588563087463,
-10.5));
#39876=CARTESIAN_POINT('Ctrl Pts',(97.7658297121615,-0.0417933956804935,
-10.5));
#39877=CARTESIAN_POINT('Ctrl Pts',(97.764107082079,-0.0533166512022675,
-10.5));
#39878=CARTESIAN_POINT('Ctrl Pts',(97.762222928785,-0.0648035136284369,
-10.5));
#39879=CARTESIAN_POINT('Ctrl Pts',(97.7537235936656,-0.1166202599317,-10.5));
#39880=CARTESIAN_POINT('Ctrl Pts',(97.7419297521137,-0.167796425585881,
-10.5));
#39881=CARTESIAN_POINT('Ctrl Pts',(97.7270294698183,-0.218079862035151,
-10.5));
#39882=CARTESIAN_POINT('Ctrl Pts',(97.7120073204257,-0.268774558910008,
-10.5));
#39883=CARTESIAN_POINT('Ctrl Pts',(97.6938269971693,-0.318562860100363,
-10.5));
#39884=CARTESIAN_POINT('Ctrl Pts',(97.6726356487453,-0.367160875033588,
-10.5));
#39885=CARTESIAN_POINT('Ctrl Pts',(97.6591336259524,-0.398124997381542,
-10.5));
#39886=CARTESIAN_POINT('Ctrl Pts',(97.644408373247,-0.428605353314649,-10.5));
#39887=CARTESIAN_POINT('Ctrl Pts',(97.6284904320524,-0.458520380816364,
-10.5));
#39888=CARTESIAN_POINT('Ctrl Pts',(97.6201510508066,-0.474192810828878,
-10.5));
#39889=CARTESIAN_POINT('Ctrl Pts',(97.6114842266502,-0.489709957087109,
-10.5));
#39890=CARTESIAN_POINT('Ctrl Pts',(97.6024938431448,-0.505059230819634,
-10.5));
#39891=CARTESIAN_POINT('Ctrl Pts',(97.5966859477238,-0.514975045486983,
-10.5));
#39892=CARTESIAN_POINT('Ctrl Pts',(97.5907474448757,-0.524813128712183,
-10.5));
#39893=CARTESIAN_POINT('Ctrl Pts',(97.5846829146721,-0.534565759424631,
-10.5));
#39894=CARTESIAN_POINT('Ctrl Pts',(97.557451153234,-0.578358321097343,-10.5));
#39895=CARTESIAN_POINT('Ctrl Pts',(97.5276624401207,-0.620462600956481,
-10.5));
#39896=CARTESIAN_POINT('Ctrl Pts',(97.4954500652803,-0.660602101447504,
-10.5));
#39897=CARTESIAN_POINT('Ctrl Pts',(97.4703422909784,-0.691888634151548,
-10.5));
#39898=CARTESIAN_POINT('Ctrl Pts',(97.4437612066321,-0.721980945035717,
-10.5));
#39899=CARTESIAN_POINT('Ctrl Pts',(97.4157584644867,-0.75072877166702,-10.5));
#39900=CARTESIAN_POINT('Ctrl Pts',(97.4049420135528,-0.761833021907868,
-10.5));
#39901=CARTESIAN_POINT('Ctrl Pts',(97.3939097361129,-0.772739659318788,
-10.5));
#39902=CARTESIAN_POINT('Ctrl Pts',(97.3826861942266,-0.783419204631785,
-10.5));
#39903=CARTESIAN_POINT('Ctrl Pts',(97.346908313003,-0.81746295905454,-10.5));
#39904=CARTESIAN_POINT('Ctrl Pts',(97.3091533165845,-0.849241353705008,
-10.5));
#39905=CARTESIAN_POINT('Ctrl Pts',(97.2695300366762,-0.878485320260425,
-10.5));
#39906=CARTESIAN_POINT('Ctrl Pts',(97.2299067567679,-0.907729286815843,
-10.5));
#39907=CARTESIAN_POINT('Ctrl Pts',(97.1884145438752,-0.93443952153388,-10.5));
#39908=CARTESIAN_POINT('Ctrl Pts',(97.1451453741165,-0.958295198918411,
-10.5));
#39909=CARTESIAN_POINT('',(97.1458324630994,-0.958883592186423,0.000494446711454889));
#39910=CARTESIAN_POINT('Ctrl Pts',(97.1466202729343,-0.959424520989747,
9.31828399164392E-15));
#39911=CARTESIAN_POINT('Ctrl Pts',(97.1772000435651,-0.942816385269717,
2.8509622347868E-15));
#39912=CARTESIAN_POINT('Ctrl Pts',(97.206909689724,-0.924824757093772,9.99012851391334E-15));
#39913=CARTESIAN_POINT('Ctrl Pts',(97.2356432203996,-0.905478322627354,
6.69603261727048E-15));
#39914=CARTESIAN_POINT('Ctrl Pts',(97.2754551973134,-0.8786727131449,1.91303236758859E-15));
#39915=CARTESIAN_POINT('Ctrl Pts',(97.3133946513639,-0.849268561702089,
2.31792913122294E-14));
#39916=CARTESIAN_POINT('Ctrl Pts',(97.3494001049585,-0.817569258176344,
2.5954932647565E-14));
#39917=CARTESIAN_POINT('Ctrl Pts',(97.3839689672423,-0.787134733717629,
2.87388746824356E-14));
#39918=CARTESIAN_POINT('Ctrl Pts',(97.4167554059431,-0.754583690540391,
5.09432319230377E-15));
#39919=CARTESIAN_POINT('Ctrl Pts',(97.447687563878,-0.720145741968749,1.92866556059101E-14));
#39920=CARTESIAN_POINT('Ctrl Pts',(97.4644376227941,-0.701497263943401,
2.70598459029195E-14));
#39921=CARTESIAN_POINT('Ctrl Pts',(97.4806436126852,-0.682294876652444,
1.24190508234713E-14));
#39922=CARTESIAN_POINT('Ctrl Pts',(97.4962913478694,-0.662571287839571,
1.84921522539128E-14));
#39923=CARTESIAN_POINT('Ctrl Pts',(97.5025355811585,-0.654700583971173,
2.10484807325984E-14));
#39924=CARTESIAN_POINT('Ctrl Pts',(97.5086857564786,-0.646753256969243,
2.79135666469497E-14));
#39925=CARTESIAN_POINT('Ctrl Pts',(97.5147378717323,-0.638736474398883,
2.78388423424758E-14));
#39926=CARTESIAN_POINT('Ctrl Pts',(97.5456685520257,-0.597764925068949,
2.75219226050856E-14));
#39927=CARTESIAN_POINT('Ctrl Pts',(97.574069340512,-0.554946070203035,1.1374087770192E-14));
#39928=CARTESIAN_POINT('Ctrl Pts',(97.5998669969729,-0.510609758068244,
9.35362898246694E-15));
#39929=CARTESIAN_POINT('Ctrl Pts',(97.6262338873721,-0.465295150342756,
7.24263366321213E-15));
#39930=CARTESIAN_POINT('Ctrl Pts',(97.6498822495387,-0.41839459509935,2.45765135840765E-14));
#39931=CARTESIAN_POINT('Ctrl Pts',(97.6707026342043,-0.370215921141815,
9.78384040450919E-15));
#39932=CARTESIAN_POINT('Ctrl Pts',(97.6902204920045,-0.325051313359365,
-4.4286697064792E-15));
#39933=CARTESIAN_POINT('Ctrl Pts',(97.7072533202619,-0.278762428188124,
2.28542419073914E-14));
#39934=CARTESIAN_POINT('Ctrl Pts',(97.7216779303715,-0.231578653933733,
1.02001740387436E-15));
#39935=CARTESIAN_POINT('Ctrl Pts',(97.7245628026305,-0.222142061860196,
-3.40706245095146E-15));
#39936=CARTESIAN_POINT('Ctrl Pts',(97.7273405894162,-0.212678180277356,
1.20348809539547E-14));
#39937=CARTESIAN_POINT('Ctrl Pts',(97.7300098441781,-0.203192277103622,
1.16434639707563E-14));
#39938=CARTESIAN_POINT('Ctrl Pts',(97.7447154730192,-0.150931933398112,
9.82772154440629E-15));
#39939=CARTESIAN_POINT('Ctrl Pts',(97.7561395027148,-0.09797517174401,4.93265201506828E-16));
#39940=CARTESIAN_POINT('Ctrl Pts',(97.7641794825515,-0.0446542022561014,
-2.91433543964104E-16));
#39941=CARTESIAN_POINT('Ctrl Pts',(97.7721731219472,0.00835943844565992,
-1.07340161594935E-15));
#39942=CARTESIAN_POINT('Ctrl Pts',(97.7768222245354,0.0617341894820306,
1.98200327771534E-14));
#39943=CARTESIAN_POINT('Ctrl Pts',(97.777982886155,0.115169799540912,2.12746487093796E-14));
#39944=CARTESIAN_POINT('Ctrl Pts',(97.7783979164878,0.134277348761075,2.1813788991162E-14));
#39945=CARTESIAN_POINT('Ctrl Pts',(97.7783664526014,0.153392845938293,9.27618377225713E-15));
#39946=CARTESIAN_POINT('Ctrl Pts',(97.7778803285128,0.172502974242189,1.77219350305791E-14));
#39947=CARTESIAN_POINT('Ctrl Pts',(97.7774094242059,0.191014794440757,2.59186172024163E-14));
#39948=CARTESIAN_POINT('Ctrl Pts',(97.7765118801322,0.209521582396939,1.00647601749991E-14));
#39949=CARTESIAN_POINT('Ctrl Pts',(97.7751951538298,0.228013923914682,1.25871535416877E-14));
#39950=CARTESIAN_POINT('Ctrl Pts',(97.7742947580553,0.24065924445855,1.426827868324E-14));
#39951=CARTESIAN_POINT('Ctrl Pts',(97.7731983350769,0.25329781108981,1.89882289688263E-14));
#39952=CARTESIAN_POINT('Ctrl Pts',(97.7719080551977,0.265926612846937,7.67441665772139E-15));
#39953=CARTESIAN_POINT('Ctrl Pts',(97.770904685478,0.275747239738408,-1.27219627523598E-15));
#39954=CARTESIAN_POINT('Ctrl Pts',(97.7697845744754,0.285556547529046,1.18323679014023E-14));
#39955=CARTESIAN_POINT('Ctrl Pts',(97.7685502311383,0.2953453042908,1.36418654150816E-14));
#39956=CARTESIAN_POINT('Ctrl Pts',(97.76175934138,0.349199338287771,2.41200680770917E-14));
#39957=CARTESIAN_POINT('Ctrl Pts',(97.7515083176503,0.402502016329768,3.80654692591887E-14));
#39958=CARTESIAN_POINT('Ctrl Pts',(97.7380513471759,0.455014629129198,2.81302758864399E-14));
#39959=CARTESIAN_POINT('Ctrl Pts',(97.7245943767015,0.507527241928628,1.81950825136911E-14));
#39960=CARTESIAN_POINT('Ctrl Pts',(97.7079310928974,0.559250673400171,1.81745979355416E-14));
#39961=CARTESIAN_POINT('Ctrl Pts',(97.6882615948245,0.609952423015609,8.90953977261688E-15));
#39962=CARTESIAN_POINT('Ctrl Pts',(97.6741507870948,0.646325625714142,2.17032712502928E-15));
#39963=CARTESIAN_POINT('Ctrl Pts',(97.6584916710932,0.682173182980464,3.58040368876852E-14));
#39964=CARTESIAN_POINT('Ctrl Pts',(97.6413425828207,0.71740732801415,2.72143418911241E-14));
#39965=CARTESIAN_POINT('Ctrl Pts',(97.6343564201633,0.731760946374833,2.37222638421511E-14));
#39966=CARTESIAN_POINT('Ctrl Pts',(97.6271228439595,0.746012728042026,7.49441688733765E-15));
#39967=CARTESIAN_POINT('Ctrl Pts',(97.6196452280311,0.760156545554777,1.99978922310606E-14));
#39968=CARTESIAN_POINT('Ctrl Pts',(97.6146240899864,0.769653965707259,2.81848743562857E-14));
#39969=CARTESIAN_POINT('Ctrl Pts',(97.6094929748939,0.779102355169158,3.56241109591605E-14));
#39970=CARTESIAN_POINT('Ctrl Pts',(97.6042599031689,0.788487808932253,3.17662562920873E-14));
#39971=CARTESIAN_POINT('Ctrl Pts',(97.5764823540215,0.838306522849914,1.14908850691008E-14));
#39972=CARTESIAN_POINT('Ctrl Pts',(97.5457904930518,0.88644061665542,2.43775865153609E-14));
#39973=CARTESIAN_POINT('Ctrl Pts',(97.5123991020691,0.93263343166495,2.61735078055381E-14));
#39974=CARTESIAN_POINT('Ctrl Pts',(97.4844179100545,0.971341912756621,2.76234915115376E-14));
#39975=CARTESIAN_POINT('Ctrl Pts',(97.4545399996545,1.00868751676431,1.11804510128399E-14));
#39976=CARTESIAN_POINT('Ctrl Pts',(97.4228654712748,1.04451118656265,2.90045765183322E-14));
#39977=CARTESIAN_POINT('Ctrl Pts',(97.4142291322117,1.0542788255675,3.37850636592315E-14));
#39978=CARTESIAN_POINT('Ctrl Pts',(97.4054591001408,1.06393325519369,3.00163047873623E-14));
#39979=CARTESIAN_POINT('Ctrl Pts',(97.396557125927,1.07347108761765,2.89213097914853E-14));
#39980=CARTESIAN_POINT('Ctrl Pts',(97.3879421590792,1.08270141205566,2.79854433512853E-14));
#39981=CARTESIAN_POINT('Ctrl Pts',(97.3792090872826,1.09181661488917,2.79116941233197E-14));
#39982=CARTESIAN_POINT('Ctrl Pts',(97.3703634096788,1.10081055725528,2.57571741713036E-14));
#39983=CARTESIAN_POINT('Ctrl Pts',(97.3290717691756,1.14279429796123,1.54378006085243E-14));
#39984=CARTESIAN_POINT('Ctrl Pts',(97.285307623798,1.18216180934031,1.40986011756825E-14));
#39985=CARTESIAN_POINT('Ctrl Pts',(97.2392696854532,1.21863191240908,1.55708779203678E-14));
#39986=CARTESIAN_POINT('Ctrl Pts',(97.1932317471084,1.25510201547784,1.69060522755085E-14));
#39987=CARTESIAN_POINT('Ctrl Pts',(97.1449194813229,1.28867583838664,2.09837577252251E-15));
#39988=CARTESIAN_POINT('Ctrl Pts',(97.0944880441522,1.31904027763685,1.16850973341798E-14));
#39989=CARTESIAN_POINT('Ctrl Pts',(97.1453218036553,-0.958169122381499,
0.000494446711454821));
#39990=CARTESIAN_POINT('Ctrl Pts',(97.1415381744624,-0.960873429781328,
0.00032963114095207));
#39991=CARTESIAN_POINT('Ctrl Pts',(97.1377385268835,-0.963555325660809,
0.000164815570449321));
#39992=CARTESIAN_POINT('Ctrl Pts',(97.1339231275304,-0.966214621837944,
-5.34294830600857E-14));
#39993=CARTESIAN_POINT('Ctrl Pts',(95.6089494686613,-1.19245765552795,0.166027734467303));
#39994=CARTESIAN_POINT('Ctrl Pts',(95.2142463808146,-0.910612241588899,
0.139688080028275));
#39995=CARTESIAN_POINT('Ctrl Pts',(94.7334030913231,0.0708416381760633,
0.0870151469733932));
#39996=CARTESIAN_POINT('Ctrl Pts',(95.5775313502033,1.48787114334542,0.00800893530265735));
#39997=CARTESIAN_POINT('Ctrl Pts',(97.2235943441107,1.55113222293223,-0.070990900544905));
#39998=CARTESIAN_POINT('Ctrl Pts',(98.1768471138565,0.209077371665153,-0.149990736392467));
#39999=CARTESIAN_POINT('Ctrl Pts',(97.5732580287732,-1.32360584827862,-0.228990572240029));
#40000=CARTESIAN_POINT('Ctrl Pts',(95.960016997387,-1.65501977806249,-0.307990408087592));
#40001=CARTESIAN_POINT('Ctrl Pts',(94.8008678817747,-0.485232819228974,
-0.386990243935154));
#40002=CARTESIAN_POINT('Ctrl Pts',(95.1472986348494,1.12488635124402,-0.465990079782718));
#40003=CARTESIAN_POINT('Ctrl Pts',(96.6850760631179,1.71443609477336,-0.544989915630279));
#40004=CARTESIAN_POINT('Ctrl Pts',(98.0190902033242,0.748668362857634,-0.623989751477842));
#40005=CARTESIAN_POINT('Ctrl Pts',(97.9391262882993,-0.89631367659507,-0.702989587325403));
#40006=CARTESIAN_POINT('Ctrl Pts',(96.5177214247813,-1.72814452071155,-0.781989423172969));
#40007=CARTESIAN_POINT('Ctrl Pts',(95.0443887169318,-0.992193356934267,
-0.860989259020528));
#40008=CARTESIAN_POINT('Ctrl Pts',(94.8557454082464,0.64388558250149,-0.939989094868094));
#40009=CARTESIAN_POINT('Ctrl Pts',(96.1229310831989,1.69582536089387,-1.01898893071566));
#40010=CARTESIAN_POINT('Ctrl Pts',(97.6963444937537,1.20929961996931,-1.09798876656322));
#40011=CARTESIAN_POINT('Ctrl Pts',(98.1485728720161,-0.374312516833932,
-1.17698860241079));
#40012=CARTESIAN_POINT('Ctrl Pts',(97.0693509649446,-1.61834525395207,-1.25598843825835));
#40013=CARTESIAN_POINT('Ctrl Pts',(95.4377574197567,-1.394202544772,-1.33498827410591));
#40014=CARTESIAN_POINT('Ctrl Pts',(94.7339866801775,0.0947716969215828,
-1.41398810995347));
#40015=CARTESIAN_POINT('Ctrl Pts',(95.5965051021273,1.49776829191394,-1.49298794580103));
#40016=CARTESIAN_POINT('Ctrl Pts',(97.2428291934931,1.54197774292137,-1.5719877816486));
#40017=CARTESIAN_POINT('Ctrl Pts',(98.1794008169382,0.187292874166953,-1.65098761749616));
#40018=CARTESIAN_POINT('Ctrl Pts',(97.5565548403935,-1.33730555798415,-1.72998745334372));
#40019=CARTESIAN_POINT('Ctrl Pts',(95.9393420249252,-1.64868988972742,-1.80898728919129));
#40020=CARTESIAN_POINT('Ctrl Pts',(94.7949105333028,-0.46436980861648,-1.88798712503885));
#40021=CARTESIAN_POINT('Ctrl Pts',(95.1614976001875,1.14123020841151,-1.96698696088641));
#40022=CARTESIAN_POINT('Ctrl Pts',(96.7065325602059,1.71149722047994,-2.04598679673397));
#40023=CARTESIAN_POINT('Ctrl Pts',(98.0283475672782,0.729080516688774,-2.12498663258154));
#40024=CARTESIAN_POINT('Ctrl Pts',(97.9277816690826,-0.914763755975596,
-2.20398646842909));
#40025=CARTESIAN_POINT('Ctrl Pts',(96.4960690380457,-1.72872716722286,-2.28298630427666));
#40026=CARTESIAN_POINT('Ctrl Pts',(95.032070613737,-0.974375719723946,-2.36198614012422));
#40027=CARTESIAN_POINT('Ctrl Pts',(94.8639372608783,0.663937030748207,-2.44098597597178));
#40028=CARTESIAN_POINT('Ctrl Pts',(96.1442008772341,1.69992089420785,-2.51998581181935));
#40029=CARTESIAN_POINT('Ctrl Pts',(97.7113962584065,1.19372317597498,-2.5989856476669));
#40030=CARTESIAN_POINT('Ctrl Pts',(98.1437514501881,-0.395429579693847,
-2.67798548351448));
#40031=CARTESIAN_POINT('Ctrl Pts',(97.0490304280756,-1.62584551605722,-2.75698531936203));
#40032=CARTESIAN_POINT('Ctrl Pts',(95.4203726982335,-1.38128163537028,-2.8359851552096));
#40033=CARTESIAN_POINT('Ctrl Pts',(94.7353093401365,0.116391789680825,-2.91498499105715));
#40034=CARTESIAN_POINT('Ctrl Pts',(95.615335210839,1.50847366931512,-2.99398482690473));
#40035=CARTESIAN_POINT('Ctrl Pts',(97.2620839311558,1.53205639277676,-3.07298466275228));
#40036=CARTESIAN_POINT('Ctrl Pts',(98.181612133017,0.16574552818808,-3.15198449859985));
#40037=CARTESIAN_POINT('Ctrl Pts',(97.5397166122691,-1.35093098087869,-3.23098433444741));
#40038=CARTESIAN_POINT('Ctrl Pts',(95.918730025002,-1.64203229762585,-3.30998417029497));
#40039=CARTESIAN_POINT('Ctrl Pts',(94.7892241299194,-0.443469021997726,
-3.38898400614253));
#40040=CARTESIAN_POINT('Ctrl Pts',(95.1758955430473,1.15741283216291,-3.4679838419901));
#40041=CARTESIAN_POINT('Ctrl Pts',(96.7279529225517,1.7082806778739,-3.54698367783766));
#40042=CARTESIAN_POINT('Ctrl Pts',(98.0373576281896,0.709382880517475,-3.62598351368522));
#40043=CARTESIAN_POINT('Ctrl Pts',(97.9162074305732,-0.933072635570782,
-3.70498334953278));
#40044=CARTESIAN_POINT('Ctrl Pts',(96.4744107401569,-1.7290373309037,-3.78398318538035));
#40045=CARTESIAN_POINT('Ctrl Pts',(95.0199768343608,-0.956405784575361,
-3.86298302122791));
#40046=CARTESIAN_POINT('Ctrl Pts',(94.8723795716142,0.683884598479127,-3.94198285707547));
#40047=CARTESIAN_POINT('Ctrl Pts',(96.1655203475008,1.7037495044598,-4.02098269292304));
#40048=CARTESIAN_POINT('Ctrl Pts',(97.7262516973936,1.1779594834696,-4.0999825287706));
#40049=CARTESIAN_POINT('Ctrl Pts',(98.1386658870132,-0.416484629352105,
-4.17898236461816));
#40050=CARTESIAN_POINT('Ctrl Pts',(97.028617525579,-1.63309061651,-4.25798220046572));
#40051=CARTESIAN_POINT('Ctrl Pts',(95.4031512018262,-1.36814397460409,-4.33698203631329));
#40052=CARTESIAN_POINT('Ctrl Pts',(94.7369027265695,0.137993622672245,-4.41598187216085));
#40053=CARTESIAN_POINT('Ctrl Pts',(95.6342979474299,1.51894232204099,-4.49498170800841));
#40054=CARTESIAN_POINT('Ctrl Pts',(97.2812128743889,1.52189462129242,-4.57398154385597));
#40055=CARTESIAN_POINT('Ctrl Pts',(98.1835533554055,0.144172171366491,-4.65298137970354));
#40056=CARTESIAN_POINT('Ctrl Pts',(97.5227090216212,-1.36434440435165,-4.7319812155511));
#40057=CARTESIAN_POINT('Ctrl Pts',(95.898203041084,-1.63511702466368,-4.81098105139866));
#40058=CARTESIAN_POINT('Ctrl Pts',(94.7837999937036,-0.422498642525088,
-4.88998088724622));
#40059=CARTESIAN_POINT('Ctrl Pts',(95.1904950734952,1.17341382524522,-4.96898072309378));
#40060=CARTESIAN_POINT('Ctrl Pts',(96.7493313110161,1.70479605801417,-5.04798055894135));
#40061=CARTESIAN_POINT('Ctrl Pts',(98.0461202328097,0.689573922210988,-5.12698039478891));
#40062=CARTESIAN_POINT('Ctrl Pts',(97.9044047476399,-0.951235089823737,
-5.20598023063647));
#40063=CARTESIAN_POINT('Ctrl Pts',(96.4527502562932,-1.72907616000729,-5.28498006648404));
#40064=CARTESIAN_POINT('Ctrl Pts',(95.0081091105889,-0.938285762461949,
-5.36397990233159));
#40065=CARTESIAN_POINT('Ctrl Pts',(94.8810711001165,0.703724845483841,-5.44297973817916));
#40066=CARTESIAN_POINT('Ctrl Pts',(96.1868861053805,1.70731074850284,-5.52197957402672));
#40067=CARTESIAN_POINT('Ctrl Pts',(97.7409085013552,1.16201093599497,-5.60097940987428));
#40068=CARTESIAN_POINT('Ctrl Pts',(98.1333169694285,-0.437474320859729,
-5.67997924572183));
#40069=CARTESIAN_POINT('Ctrl Pts',(97.0081154664765,-1.64007943912008,-5.7589790815694));
#40070=CARTESIAN_POINT('Ctrl Pts',(95.3860956301902,-1.35479161357392,-5.83797891741698));
#40071=CARTESIAN_POINT('Ctrl Pts',(94.738766590895,0.159573800583674,-5.91697875326452));
#40072=CARTESIAN_POINT('Ctrl Pts',(95.6533903353675,1.52917261000153,-5.9959785891121));
#40073=CARTESIAN_POINT('Ctrl Pts',(97.3002130217027,1.51149402174397,-6.07497842495966));
#40074=CARTESIAN_POINT('Ctrl Pts',(98.185224179278,0.122576189876859,-6.15397826080722));
#40075=CARTESIAN_POINT('Ctrl Pts',(97.5055347375172,-1.37754372382008,-6.23297809665479));
#40076=CARTESIAN_POINT('Ctrl Pts',(95.877764294382,-1.6279451558583,-6.31197793250235));
#40077=CARTESIAN_POINT('Ctrl Pts',(94.7786389758806,-0.401461961134109,
-6.39097776834991));
#40078=CARTESIAN_POINT('Ctrl Pts',(95.2052939004409,1.18923067670014,-6.46997760419747));
#40079=CARTESIAN_POINT('Ctrl Pts',(96.770664370736,1.70104390771143,-6.54897744004503));
#40080=CARTESIAN_POINT('Ctrl Pts',(98.0546340060357,0.669656750364228,-6.62797727589259));
#40081=CARTESIAN_POINT('Ctrl Pts',(97.8923754724572,-0.969248268540891,
-6.70697711174016));
#40082=CARTESIAN_POINT('Ctrl Pts',(96.4310909855927,-1.72884364843707,-6.78597694758772));
#40083=CARTESIAN_POINT('Ctrl Pts',(94.9964693048017,-0.920018496926357,
-6.86497678343529));
#40084=CARTESIAN_POINT('Ctrl Pts',(94.8900104824397,0.723454658270465,-6.94397661928285));
#40085=CARTESIAN_POINT('Ctrl Pts',(96.2082947979853,1.71060406747721,-7.02297645513041));
#40086=CARTESIAN_POINT('Ctrl Pts',(97.7553643702261,1.14588003632696,-7.10197629097797));
#40087=CARTESIAN_POINT('Ctrl Pts',(98.1277055368295,-0.458395360343963,
-7.18097612682554));
#40088=CARTESIAN_POINT('Ctrl Pts',(96.9875274681182,-1.64681088714457,-7.25997596267309));
#40089=CARTESIAN_POINT('Ctrl Pts',(95.3692086598241,-1.34122664764074,-7.33897579852067));
#40090=CARTESIAN_POINT('Ctrl Pts',(94.7409006406209,0.181128936878324,-7.41797563436821));
#40091=CARTESIAN_POINT('Ctrl Pts',(95.672609378519,1.53916292777684,-7.4969754702158));
#40092=CARTESIAN_POINT('Ctrl Pts',(97.3190813914398,1.50085622627801,-7.57597530606333));
#40093=CARTESIAN_POINT('Ctrl Pts',(98.1866243424353,0.100960972735917,-7.65497514191093));
#40094=CARTESIAN_POINT('Ctrl Pts',(97.4881964550856,-1.39052686793939,-7.73397497775846));
#40095=CARTESIAN_POINT('Ctrl Pts',(95.8574169923098,-1.62051781667803,-7.81297481360604));
#40096=CARTESIAN_POINT('Ctrl Pts',(94.7737418863601,-0.380362279070926,
-7.8919746494536));
#40097=CARTESIAN_POINT('Ctrl Pts',(95.2202897015312,1.20486090441735,-7.97097448530115));
#40098=CARTESIAN_POINT('Ctrl Pts',(96.7919487539561,1.69702481578656,-8.04997432114873));
#40099=CARTESIAN_POINT('Ctrl Pts',(98.0628976118138,0.64963449053567,-8.12897415699628));
#40100=CARTESIAN_POINT('Ctrl Pts',(97.8801214927624,-0.987109344936422,
-8.20797399284384));
#40101=CARTESIAN_POINT('Ctrl Pts',(96.4094363269932,-1.72833983270331,-8.28697382869141));
#40102=CARTESIAN_POINT('Ctrl Pts',(94.9850592436326,-0.901606854571692,
-8.36597366453896));
#40103=CARTESIAN_POINT('Ctrl Pts',(94.899196315702,0.743070940588966,-8.44497350038655));
#40104=CARTESIAN_POINT('Ctrl Pts',(96.2297430657699,1.71362894474065,-8.52397333623409));
#40105=CARTESIAN_POINT('Ctrl Pts',(97.7696170353154,1.1295693155191,-8.60297317208167));
#40106=CARTESIAN_POINT('Ctrl Pts',(98.1218324701197,-0.479244464040642,
-8.6819730079292));
#40107=CARTESIAN_POINT('Ctrl Pts',(96.9668567607269,-1.6532839055364,-8.76097284377679));
#40108=CARTESIAN_POINT('Ctrl Pts',(95.3524929419726,-1.32745120296166,-8.83997267962433));
#40109=CARTESIAN_POINT('Ctrl Pts',(94.743304538488,0.202655643903087,-8.91897251547192));
#40110=CARTESIAN_POINT('Ctrl Pts',(95.6919520655271,1.54891171752243,-8.99797235131946));
#40111=CARTESIAN_POINT('Ctrl Pts',(97.3378150134816,1.48998288477276,-9.07697218716705));
#40112=CARTESIAN_POINT('Ctrl Pts',(98.1877536431172,0.0793299502857095,
-9.15597202301459));
#40113=CARTESIAN_POINT('Ctrl Pts',(97.4706968598829,-1.40329187457507,-9.23497185886216));
#40114=CARTESIAN_POINT('Ctrl Pts',(95.8371643973225,-1.61283602471812,-9.31397169470972));
#40115=CARTESIAN_POINT('Ctrl Pts',(94.7691093572545,-0.359203198268218,
-9.39297153055729));
#40116=CARTESIAN_POINT('Ctrl Pts',(95.2354803915345,1.22030262709654,-9.47197136640485));
#40117=CARTESIAN_POINT('Ctrl Pts',(96.8131805937843,1.69273828970788,-9.55097120225241));
#40118=CARTESIAN_POINT('Ctrl Pts',(98.0709107886458,0.62951249234026,-9.62997103809997));
#40119=CARTESIAN_POINT('Ctrl Pts',(97.8676426968368,-1.00481985473004,-9.70897087394753));
#40120=CARTESIAN_POINT('Ctrl Pts',(96.3877936776409,-1.72755626495539,-9.78797070979509));
#40121=CARTESIAN_POINT('Ctrl Pts',(94.9738728583651,-0.883070483070808,
-9.86697054564266));
#40122=CARTESIAN_POINT('Ctrl Pts',(94.9086426046154,0.762603550204478,-9.94597038149023));
#40123=CARTESIAN_POINT('Ctrl Pts',(96.2511971856125,1.71632017390702,-10.0249702173378));
#40124=CARTESIAN_POINT('Ctrl Pts',(97.78372392326,1.11320856185152,-10.1039700531854));
#40125=CARTESIAN_POINT('Ctrl Pts',(98.1155814248733,-0.500268501807092,
-10.1829698890329));
#40126=CARTESIAN_POINT('Ctrl Pts',(96.9463371342804,-1.65900482028253,-10.2619697248805));
#40127=CARTESIAN_POINT('Ctrl Pts',(95.3354971295683,-1.31444738919156,-10.3409695607281));
#40128=CARTESIAN_POINT('Ctrl Pts',(94.7468801337304,0.226207046957059,-10.4199693965756));
#40129=CARTESIAN_POINT('Ctrl Pts',(95.3886793944715,1.11059179364519,-10.4726359538073));
#40130=CARTESIAN_POINT('Ctrl Pts',(95.8257004218783,1.32064939124249,-10.4989692324232));
#40131=CARTESIAN_POINT('Ctrl Pts',(95.6650518398339,-1.11389367580726,0.110290927349878));
#40132=CARTESIAN_POINT('Ctrl Pts',(95.296353403176,-0.850617388648033,0.0839512729108505));
#40133=CARTESIAN_POINT('Ctrl Pts',(94.8471900331093,0.0661743017727613,
0.0312783398559688));
#40134=CARTESIAN_POINT('Ctrl Pts',(95.6357036753152,1.38984411673286,-0.047727871814767));
#40135=CARTESIAN_POINT('Ctrl Pts',(97.1733173175222,1.44893729807126,-0.12672770766233));
#40136=CARTESIAN_POINT('Ctrl Pts',(98.0637659022104,0.195302500657018,-0.205727543509892));
#40137=CARTESIAN_POINT('Ctrl Pts',(97.4999437307949,-1.23640129007877,-0.284727379357454));
#40138=CARTESIAN_POINT('Ctrl Pts',(95.9929896061911,-1.545980316847,-0.363727215205017));
#40139=CARTESIAN_POINT('Ctrl Pts',(94.9102099676746,-0.453263699660661,
-0.442727051052579));
#40140=CARTESIAN_POINT('Ctrl Pts',(95.2338164480949,1.05077424497549,-0.521726886900142));
#40141=CARTESIAN_POINT('Ctrl Pts',(96.6702788199085,1.60148204398775,-0.600726722747705));
#40142=CARTESIAN_POINT('Ctrl Pts',(97.916402661141,0.699343033941837,-0.679726558595267));
#40143=CARTESIAN_POINT('Ctrl Pts',(97.8417070953685,-0.837260871503877,
-0.758726394442829));
#40144=CARTESIAN_POINT('Ctrl Pts',(96.5139501885348,-1.61428730284708,-0.837726230290392));
#40145=CARTESIAN_POINT('Ctrl Pts',(95.1376866557998,-0.926823606979764,
-0.916726066137954));
#40146=CARTESIAN_POINT('Ctrl Pts',(94.9614719386115,0.601463771033733,-0.995725901985518));
#40147=CARTESIAN_POINT('Ctrl Pts',(96.1451702467733,1.58409746125275,-1.07472573783308));
#40148=CARTESIAN_POINT('Ctrl Pts',(97.614920756842,1.12962602285743,-1.15372557368064));
#40149=CARTESIAN_POINT('Ctrl Pts',(98.0373544828796,-0.349651279728017,
-1.23272540952821));
#40150=CARTESIAN_POINT('Ctrl Pts',(97.0292361220251,-1.51172206014459,-1.31172524537577));
#40151=CARTESIAN_POINT('Ctrl Pts',(95.5051386221701,-1.30234678792709,-1.39072508122333));
#40152=CARTESIAN_POINT('Ctrl Pts',(94.8477351727468,0.088527750530259,-1.46972491707089));
#40153=CARTESIAN_POINT('Ctrl Pts',(95.6534273589836,1.39908920073889,-1.54872475291846));
#40154=CARTESIAN_POINT('Ctrl Pts',(97.1912848964821,1.44038595258563,-1.62772458876602));
#40155=CARTESIAN_POINT('Ctrl Pts',(98.0661513569051,0.174953254810515,-1.70672442461358));
#40156=CARTESIAN_POINT('Ctrl Pts',(97.4843410166729,-1.24919840696643,-1.78572426046114));
#40157=CARTESIAN_POINT('Ctrl Pts',(95.9736767853404,-1.5400674674034,-1.86472409630871));
#40158=CARTESIAN_POINT('Ctrl Pts',(94.9046451136471,-0.433775229380962,
-1.94372393215627));
#40159=CARTESIAN_POINT('Ctrl Pts',(95.247079927615,1.066041302093,-2.02272376800383));
#40160=CARTESIAN_POINT('Ctrl Pts',(96.6903216753514,1.59873679473359,-2.1017236038514));
#40161=CARTESIAN_POINT('Ctrl Pts',(97.9250501121554,0.681045715065119,-2.18072343969896));
#40162=CARTESIAN_POINT('Ctrl Pts',(97.8311099059914,-0.854495384314323,
-2.25972327554652));
#40163=CARTESIAN_POINT('Ctrl Pts',(96.4937243494543,-1.614831562227,-2.33872311139408));
#40164=CARTESIAN_POINT('Ctrl Pts',(95.1261801195442,-0.910179868466786,
-2.41772294724165));
#40165=CARTESIAN_POINT('Ctrl Pts',(94.9691240785406,0.620194147990309,-2.4967227830892));
#40166=CARTESIAN_POINT('Ctrl Pts',(96.1650386999228,1.58792316410799,-2.57572261893677));
#40167=CARTESIAN_POINT('Ctrl Pts',(97.6289808497757,1.11507581859951,-2.65472245478433));
#40168=CARTESIAN_POINT('Ctrl Pts',(98.03285071601,-0.36937706425566,-2.73372229063189));
#40169=CARTESIAN_POINT('Ctrl Pts',(97.0102543851032,-1.51872817435509,-2.81272212647946));
#40170=CARTESIAN_POINT('Ctrl Pts',(95.4888992770912,-1.29027716079902,-2.89172196232702));
#40171=CARTESIAN_POINT('Ctrl Pts',(94.8489706904667,0.108723423293354,-2.97072179817458));
#40172=CARTESIAN_POINT('Ctrl Pts',(95.671016863241,1.4090892641617,-3.04972163402214));
#40173=CARTESIAN_POINT('Ctrl Pts',(97.2092710534012,1.43111826150216,-3.12872146986971));
#40174=CARTESIAN_POINT('Ctrl Pts',(98.068216982451,0.154825535972839,-3.20772130571727));
#40175=CARTESIAN_POINT('Ctrl Pts',(97.4686121597758,-1.26192613136156,-3.28672114156483));
#40176=CARTESIAN_POINT('Ctrl Pts',(95.9544227881412,-1.53384850465562,-3.3657209774124));
#40177=CARTESIAN_POINT('Ctrl Pts',(94.8993333537387,-0.41425147193255,-3.44472081325996));
#40178=CARTESIAN_POINT('Ctrl Pts',(95.2605292752057,1.08115774851027,-3.52372064910751));
#40179=CARTESIAN_POINT('Ctrl Pts',(96.7103307767561,1.59573217108913,-3.60272048495509));
#40180=CARTESIAN_POINT('Ctrl Pts',(97.9334665534616,0.662645839599646,-3.68172032080264));
#40181=CARTESIAN_POINT('Ctrl Pts',(97.8202982255782,-0.871598000157872,
-3.76072015665021));
#40182=CARTESIAN_POINT('Ctrl Pts',(96.4734929886715,-1.61512129105799,-3.83971999249776));
#40183=CARTESIAN_POINT('Ctrl Pts',(95.114883127738,-0.893393866025624,-3.91871982834534));
#40184=CARTESIAN_POINT('Ctrl Pts',(94.9770101753713,0.638827488503664,-3.99771966419289));
#40185=CARTESIAN_POINT('Ctrl Pts',(96.1849535564308,1.5914995298825,-4.07671950004046));
#40186=CARTESIAN_POINT('Ctrl Pts',(97.6428575517804,1.10035070252706,-4.15571933588801));
#40187=CARTESIAN_POINT('Ctrl Pts',(98.0281002105038,-0.389044921264601,
-4.23471917173559));
#40188=CARTESIAN_POINT('Ctrl Pts',(96.9911863679787,-1.52549593800485,-4.31371900758313));
#40189=CARTESIAN_POINT('Ctrl Pts',(95.4728124031908,-1.27800506277145,-4.39271884343072));
#40190=CARTESIAN_POINT('Ctrl Pts',(94.8504590980947,0.128902039316688,-4.47171867927826));
#40191=CARTESIAN_POINT('Ctrl Pts',(95.6887302573114,1.41886819929748,-4.55071851512584));
#40192=CARTESIAN_POINT('Ctrl Pts',(97.2271397037416,1.42162598901859,-4.62971835097339));
#40193=CARTESIAN_POINT('Ctrl Pts',(98.0700303091814,0.134673519992983,-4.70871818682096));
#40194=CARTESIAN_POINT('Ctrl Pts',(97.4527250986499,-1.27445582372271,-4.78771802266851));
#40195=CARTESIAN_POINT('Ctrl Pts',(95.935248205745,-1.52738883811455,-4.86671785851608));
#40196=CARTESIAN_POINT('Ctrl Pts',(94.8942665817662,-0.394662706691651,
-4.94571769436365));
#40197=CARTESIAN_POINT('Ctrl Pts',(95.2741669289706,1.09610453082861,-5.02471753021121));
#40198=CARTESIAN_POINT('Ctrl Pts',(96.7303006696905,1.59247713221513,-5.10371736605877));
#40199=CARTESIAN_POINT('Ctrl Pts',(97.9416518419073,0.644141976355837,-5.18271720190633));
#40200=CARTESIAN_POINT('Ctrl Pts',(97.8092731515925,-0.888563837758662,
-5.26171703775389));
#40201=CARTESIAN_POINT('Ctrl Pts',(96.4532595859348,-1.61515756194168,-5.34071687360145));
#40202=CARTESIAN_POINT('Ctrl Pts',(95.1037972980699,-0.876467664961753,
-5.41971670944902));
#40203=CARTESIAN_POINT('Ctrl Pts',(94.9851290704841,0.657360579018497,-5.49871654529658));
#40204=CARTESIAN_POINT('Ctrl Pts',(96.2049116509347,1.59482614462572,-5.57771638114415));
#40205=CARTESIAN_POINT('Ctrl Pts',(97.6565487056463,1.08545291048562,-5.65671621699171));
#40206=CARTESIAN_POINT('Ctrl Pts',(98.0231037014517,-0.408651726184762,
-5.73571605283926));
#40207=CARTESIAN_POINT('Ctrl Pts',(96.9720350682498,-1.53202430844267,-5.81471588868683));
#40208=CARTESIAN_POINT('Ctrl Pts',(95.4568805222601,-1.26553240981001,-5.89371572453439));
#40209=CARTESIAN_POINT('Ctrl Pts',(94.8522001634278,0.149060426985132,-5.97271556038196));
#40210=CARTESIAN_POINT('Ctrl Pts',(95.7065647607682,1.42842447411204,-6.05171539622952));
#40211=CARTESIAN_POINT('Ctrl Pts',(97.2448880437637,1.411910623439,-6.13071523207708));
#40212=CARTESIAN_POINT('Ctrl Pts',(98.0715910523545,0.114500369950604,-6.20971506792465));
#40213=CARTESIAN_POINT('Ctrl Pts',(97.4366823265136,-1.28678551812544,-6.2887149037722));
#40214=CARTESIAN_POINT('Ctrl Pts',(95.9161560471369,-1.52068948131225,-6.36771473961977));
#40215=CARTESIAN_POINT('Ctrl Pts',(94.8894455928724,-0.375012007773534,
-6.44671457546733));
#40216=CARTESIAN_POINT('Ctrl Pts',(95.2879907487666,1.11087930352192,-6.5257144113149));
#40217=CARTESIAN_POINT('Ctrl Pts',(96.7502282203229,1.58897218889616,-6.60471424716245));
#40218=CARTESIAN_POINT('Ctrl Pts',(97.9496046929873,0.625537029121671,-6.68371408301002));
#40219=CARTESIAN_POINT('Ctrl Pts',(97.7980364141802,-0.90539023470551,-6.76271391885758));
#40220=CARTESIAN_POINT('Ctrl Pts',(96.4330273164332,-1.61494036918316,-6.84171375470514));
#40221=CARTESIAN_POINT('Ctrl Pts',(95.0929243702188,-0.859403921473622,
-6.92071359055271));
#40222=CARTESIAN_POINT('Ctrl Pts',(94.9934794897961,0.675790511172483,-6.99971342640027));
#40223=CARTESIAN_POINT('Ctrl Pts',(96.2249098514488,1.59790248629786,-7.07871326224784));
#40224=CARTESIAN_POINT('Ctrl Pts',(97.6700521628457,1.0703847803579,-7.15771309809539));
#40225=CARTESIAN_POINT('Ctrl Pts',(98.0178619729467,-0.428194402157172,
-7.23671293394296));
#40226=CARTESIAN_POINT('Ctrl Pts',(96.9528034912937,-1.53831226118359,-7.31571276979052));
#40227=CARTESIAN_POINT('Ctrl Pts',(95.4411061344594,-1.25286115922476,-7.39471260563808));
#40228=CARTESIAN_POINT('Ctrl Pts',(94.8541936132431,0.169195422880768,-7.47371244148564));
#40229=CARTESIAN_POINT('Ctrl Pts',(95.7245175748764,1.43775658895706,-7.55271227733321));
#40230=CARTESIAN_POINT('Ctrl Pts',(97.2625132882538,1.40197368937753,-7.63171211318077));
#40231=CARTESIAN_POINT('Ctrl Pts',(98.0728989670454,0.0943092515801678,
-7.71071194902833));
#40232=CARTESIAN_POINT('Ctrl Pts',(97.4204863609289,-1.29891327969378,-7.78971178487589));
#40233=CARTESIAN_POINT('Ctrl Pts',(95.8971493084129,-1.51375148556655,-7.86871162072345));
#40234=CARTESIAN_POINT('Ctrl Pts',(94.8848711436064,-0.355302458924759,
-7.94771145657102));
#40235=CARTESIAN_POINT('Ctrl Pts',(95.3019985652462,1.12547974801143,-8.02671129241858));
#40236=CARTESIAN_POINT('Ctrl Pts',(96.7701103014622,1.58521789115917,-8.10571112826615));
#40237=CARTESIAN_POINT('Ctrl Pts',(97.9573238586725,0.606833917531075,-8.1847109641137));
#40238=CARTESIAN_POINT('Ctrl Pts',(97.7865897767067,-0.922074550452794,
-8.26371079996127));
#40239=CARTESIAN_POINT('Ctrl Pts',(96.4127993551685,-1.61446974688726,-8.34271063580883));
#40240=CARTESIAN_POINT('Ctrl Pts',(95.0822660504723,-0.842205313300818,
-8.4217104716564));
#40241=CARTESIAN_POINT('Ctrl Pts',(95.0020601228529,0.694114392709185,-8.50071030750395));
#40242=CARTESIAN_POINT('Ctrl Pts',(96.2449450197681,1.60072807229517,-8.57971014335152));
#40243=CARTESIAN_POINT('Ctrl Pts',(97.6833658041586,1.05514867644134,-8.65870997919908));
#40244=CARTESIAN_POINT('Ctrl Pts',(98.0123758478541,-0.447669881765458,
-8.73770981504665));
#40245=CARTESIAN_POINT('Ctrl Pts',(96.9334946545137,-1.54435881069132,-8.8167096508942));
#40246=CARTESIAN_POINT('Ctrl Pts',(95.4254917163583,-1.23999329709286,-8.89570948674177));
#40247=CARTESIAN_POINT('Ctrl Pts',(94.8564391325024,0.189303862542906,-8.97470932258933));
#40248=CARTESIAN_POINT('Ctrl Pts',(95.7425858866791,1.44686308862524,-9.0537091584369));
#40249=CARTESIAN_POINT('Ctrl Pts',(97.2800126627773,1.39181672801171,-9.13270899428446));
#40250=CARTESIAN_POINT('Ctrl Pts',(98.073953864787,0.0741033692187827,-9.21170883013202));
#40251=CARTESIAN_POINT('Ctrl Pts',(97.4041397105173,-1.31083727556667,-9.29070866597957));
#40252=CARTESIAN_POINT('Ctrl Pts',(95.8782310370846,-1.50657580142939,-9.36970850182715));
#40253=CARTESIAN_POINT('Ctrl Pts',(94.8805438244351,-0.335537424767974,
-9.44870833767471));
#40254=CARTESIAN_POINT('Ctrl Pts',(95.3161884305613,1.13990410694458,-9.52770817352227));
#40255=CARTESIAN_POINT('Ctrl Pts',(96.7899433009825,1.58121377892249,-9.60670800936984));
#40256=CARTESIAN_POINT('Ctrl Pts',(97.9648090946936,0.588037638744514,-9.68570784521739));
#40257=CARTESIAN_POINT('Ctrl Pts',(97.7749331348131,-0.938618219540738,
-9.76470768106496));
#40258=CARTESIAN_POINT('Ctrl Pts',(96.3925826119331,-1.61373780378226,-9.84370751691252));
#40259=CARTESIAN_POINT('Ctrl Pts',(95.0718166699452,-0.824890193647276,
-9.92270735276009));
#40260=CARTESIAN_POINT('Ctrl Pts',(95.0108840516792,0.712360114242248,-10.0017071886077));
#40261=CARTESIAN_POINT('Ctrl Pts',(96.264985654588,1.60324199229448,-10.0807070244552));
#40262=CARTESIAN_POINT('Ctrl Pts',(97.6965432727204,1.03986583603414,-10.1597068603028));
#40263=CARTESIAN_POINT('Ctrl Pts',(98.0065366469945,-0.467308770072661,
-10.2387066961504));
#40264=CARTESIAN_POINT('Ctrl Pts',(96.9143269448493,-1.54970280821276,-10.3177065319979));
#40265=CARTESIAN_POINT('Ctrl Pts',(95.409615657477,-1.22784622767471,-10.3967063678455));
#40266=CARTESIAN_POINT('Ctrl Pts',(94.8597791529295,0.211303602992048,-10.475706203693));
#40267=CARTESIAN_POINT('Ctrl Pts',(95.4592940575998,1.03742147120277,-10.5283727609247));
#40268=CARTESIAN_POINT('Ctrl Pts',(95.8675223551553,1.2336396165048,-10.5547060395406));
#40269=CARTESIAN_POINT('Ctrl Pts',(95.7211542110066,-1.03532969608655,0.0545541202324537));
#40270=CARTESIAN_POINT('Ctrl Pts',(95.3784604255374,-0.790622535707167,
0.0282144657934261));
#40271=CARTESIAN_POINT('Ctrl Pts',(94.9609769748953,0.0615069653694607,
-0.0244584672614556));
#40272=CARTESIAN_POINT('Ctrl Pts',(95.6938760004271,1.2918170901203,-0.103464678932191));
#40273=CARTESIAN_POINT('Ctrl Pts',(97.1230402909337,1.34674237321029,-0.182464514779754));
#40274=CARTESIAN_POINT('Ctrl Pts',(97.9506846905642,0.181527629648881,-0.261464350627316));
#40275=CARTESIAN_POINT('Ctrl Pts',(97.426629432817,-1.1491967318789,-0.340464186474878));
#40276=CARTESIAN_POINT('Ctrl Pts',(96.0259622149947,-1.43694085563152,-0.419464022322441));
#40277=CARTESIAN_POINT('Ctrl Pts',(95.0195520535749,-0.421294580092347,
-0.498463858170003));
#40278=CARTESIAN_POINT('Ctrl Pts',(95.32033426134,0.976662138706952,-0.577463694017566));
#40279=CARTESIAN_POINT('Ctrl Pts',(96.6554815766994,1.48852799320213,-0.656463529865129));
#40280=CARTESIAN_POINT('Ctrl Pts',(97.8137151189575,0.65001770502604,-0.73546336571269));
#40281=CARTESIAN_POINT('Ctrl Pts',(97.7442879024379,-0.778208066412684,
-0.814463201560254));
#40282=CARTESIAN_POINT('Ctrl Pts',(96.5101789522881,-1.5004300849826,-0.893463037407817));
#40283=CARTESIAN_POINT('Ctrl Pts',(95.2309845946679,-0.86145385702526,-0.972462873255379));
#40284=CARTESIAN_POINT('Ctrl Pts',(95.0671984689766,0.559041959565974,-1.05146270910294));
#40285=CARTESIAN_POINT('Ctrl Pts',(96.1674094103476,1.47236956161164,-1.1304625449505));
#40286=CARTESIAN_POINT('Ctrl Pts',(97.5334970199301,1.04995242574554,-1.20946238079807));
#40287=CARTESIAN_POINT('Ctrl Pts',(97.9261360937432,-0.324990042622103,
-1.28846221664563));
#40288=CARTESIAN_POINT('Ctrl Pts',(96.9891212791054,-1.4050988663371,-1.36746205249319));
#40289=CARTESIAN_POINT('Ctrl Pts',(95.5725198245835,-1.2104910310822,-1.44646188834075));
#40290=CARTESIAN_POINT('Ctrl Pts',(94.9614836653162,0.0822838041389368,
-1.52546172418832));
#40291=CARTESIAN_POINT('Ctrl Pts',(95.7103496158398,1.30041010956386,-1.60446156003588));
#40292=CARTESIAN_POINT('Ctrl Pts',(97.1397405994712,1.3387941622499,-1.68346139588344));
#40293=CARTESIAN_POINT('Ctrl Pts',(97.9529018968721,0.162613635454076,-1.762461231731));
#40294=CARTESIAN_POINT('Ctrl Pts',(97.4121271929523,-1.16109125594871,-1.84146106757857));
#40295=CARTESIAN_POINT('Ctrl Pts',(96.0080115457559,-1.43144504507938,-1.92046090342613));
#40296=CARTESIAN_POINT('Ctrl Pts',(95.0143796939912,-0.403180650145441,
-1.99946073927369));
#40297=CARTESIAN_POINT('Ctrl Pts',(95.3326622550427,0.990852395774487,-2.07846057512125));
#40298=CARTESIAN_POINT('Ctrl Pts',(96.6741107904969,1.48597636898726,-2.15746041096882));
#40299=CARTESIAN_POINT('Ctrl Pts',(97.8217526570323,0.633010913441462,-2.23646024681638));
#40300=CARTESIAN_POINT('Ctrl Pts',(97.7344381429004,-0.794227012653048,
-2.31546008266394));
#40301=CARTESIAN_POINT('Ctrl Pts',(96.4913796608627,-1.50093595723113,-2.3944599185115));
#40302=CARTESIAN_POINT('Ctrl Pts',(95.2202896253514,-0.845984017209627,
-2.47345975435907));
#40303=CARTESIAN_POINT('Ctrl Pts',(95.074310896203,0.576451265232411,-2.55245959020663));
#40304=CARTESIAN_POINT('Ctrl Pts',(96.1858765226113,1.47592543400813,-2.63145942605419));
#40305=CARTESIAN_POINT('Ctrl Pts',(97.5465654411451,1.03642846122403,-2.71045926190175));
#40306=CARTESIAN_POINT('Ctrl Pts',(97.9219499818317,-0.343324548817473,
-2.78945909774932));
#40307=CARTESIAN_POINT('Ctrl Pts',(96.971478342131,-1.41161083265297,-2.86845893359688));
#40308=CARTESIAN_POINT('Ctrl Pts',(95.5574258559488,-1.19927268622775,-2.94745876944444));
#40309=CARTESIAN_POINT('Ctrl Pts',(94.9626320407967,0.101055056905879,-3.026458605292));
#40310=CARTESIAN_POINT('Ctrl Pts',(95.7266985156432,1.3097048590083,-3.10545844113957));
#40311=CARTESIAN_POINT('Ctrl Pts',(97.1564581756467,1.33018013022757,-3.18445827698713));
#40312=CARTESIAN_POINT('Ctrl Pts',(97.9548218318848,0.143905543757601,-3.26345811283469));
#40313=CARTESIAN_POINT('Ctrl Pts',(97.3975077072827,-1.17292128184443,-3.34245794868225));
#40314=CARTESIAN_POINT('Ctrl Pts',(95.9901155512801,-1.42566471168538,-3.42145778452982));
#40315=CARTESIAN_POINT('Ctrl Pts',(95.0094425775579,-0.385033921867376,
-3.50045762037738));
#40316=CARTESIAN_POINT('Ctrl Pts',(95.3451630073641,1.00490266485763,-3.57945745622494));
#40317=CARTESIAN_POINT('Ctrl Pts',(96.6927086309606,1.48318366430436,-3.65845729207251));
#40318=CARTESIAN_POINT('Ctrl Pts',(97.8295754787336,0.615908798681818,-3.73745712792006));
#40319=CARTESIAN_POINT('Ctrl Pts',(97.724389020583,-0.810123364744962,-3.81645696376764));
#40320=CARTESIAN_POINT('Ctrl Pts',(96.4725752371862,-1.50120525121228,-3.89545679961518));
#40321=CARTESIAN_POINT('Ctrl Pts',(95.2097894211152,-0.830381947475887,
-3.97445663546276));
#40322=CARTESIAN_POINT('Ctrl Pts',(95.0816407791284,0.593770378528202,-4.05345647131031));
#40323=CARTESIAN_POINT('Ctrl Pts',(96.2043867653607,1.47924955530519,-4.13245630715788));
#40324=CARTESIAN_POINT('Ctrl Pts',(97.5594634061673,1.02274192158454,-4.21145614300544));
#40325=CARTESIAN_POINT('Ctrl Pts',(97.9175345339944,-0.361605213177098,
-4.29045597885301));
#40326=CARTESIAN_POINT('Ctrl Pts',(96.9537552103785,-1.41790125949968,-4.36945581470056));
#40327=CARTESIAN_POINT('Ctrl Pts',(95.5424736045553,-1.18786615093881,-4.44845565054813));
#40328=CARTESIAN_POINT('Ctrl Pts',(94.9640154696202,0.119810455961133,-4.52745548639569));
#40329=CARTESIAN_POINT('Ctrl Pts',(95.7431625671928,1.31879407655398,-4.60645532224326));
#40330=CARTESIAN_POINT('Ctrl Pts',(97.1730665330944,1.32135735674475,-4.68545515809081));
#40331=CARTESIAN_POINT('Ctrl Pts',(97.9565072629573,0.125174868619475,-4.76445499393838));
#40332=CARTESIAN_POINT('Ctrl Pts',(97.3827411756789,-1.18456724309377,-4.84345482978594));
#40333=CARTESIAN_POINT('Ctrl Pts',(95.9722933704059,-1.41966065156544,-4.92245466563351));
#40334=CARTESIAN_POINT('Ctrl Pts',(95.0047331698288,-0.366826770858215,
-5.00145450148106));
#40335=CARTESIAN_POINT('Ctrl Pts',(95.3578387844463,1.01879523641201,-5.08045433732863));
#40336=CARTESIAN_POINT('Ctrl Pts',(96.7112700283648,1.48015820641608,-5.15945417317619));
#40337=CARTESIAN_POINT('Ctrl Pts',(97.8371834510051,0.598710030500683,-5.23845400902375));
#40338=CARTESIAN_POINT('Ctrl Pts',(97.7141415555451,-0.825892585693585,
-5.31745384487131));
#40339=CARTESIAN_POINT('Ctrl Pts',(96.4537689155765,-1.50123896387606,-5.39645368071888));
#40340=CARTESIAN_POINT('Ctrl Pts',(95.1994854855508,-0.814649567461558,
-5.47545351656644));
#40341=CARTESIAN_POINT('Ctrl Pts',(95.0891870408519,0.610996312553152,-5.554453352414));
#40342=CARTESIAN_POINT('Ctrl Pts',(96.2229371964889,1.48234154074859,-5.63345318826156));
#40343=CARTESIAN_POINT('Ctrl Pts',(97.5721889099376,1.00889488497626,-5.71245302410913));
#40344=CARTESIAN_POINT('Ctrl Pts',(97.9128904334748,-0.379829131509795,
-5.79145285995669));
#40345=CARTESIAN_POINT('Ctrl Pts',(96.935954670023,-1.42396917776525,-5.87045269580425));
#40346=CARTESIAN_POINT('Ctrl Pts',(95.5276654143301,-1.17627320604611,-5.94945253165182));
#40347=CARTESIAN_POINT('Ctrl Pts',(94.9656337359601,0.138547053386591,-6.02845236749938));
#40348=CARTESIAN_POINT('Ctrl Pts',(95.7597391861691,1.32767633822254,-6.10745220334694));
#40349=CARTESIAN_POINT('Ctrl Pts',(97.1895630658246,1.31232722513404,-6.18645203919449));
#40350=CARTESIAN_POINT('Ctrl Pts',(97.9579579254309,0.106424550024346,-6.26545187504207));
#40351=CARTESIAN_POINT('Ctrl Pts',(97.36782991551,-1.19602731243079,-6.34445171088962));
#40352=CARTESIAN_POINT('Ctrl Pts',(95.9545477998918,-1.41343380676619,-6.4234515467372));
#40353=CARTESIAN_POINT('Ctrl Pts',(95.000252209864,-0.348562054412959,-6.50245138258475));
#40354=CARTESIAN_POINT('Ctrl Pts',(95.3706875970921,1.03252793034369,-6.58145121843232));
#40355=CARTESIAN_POINT('Ctrl Pts',(96.72979206991,1.47690047008088,-6.66045105427987));
#40356=CARTESIAN_POINT('Ctrl Pts',(97.8445753799389,0.581417307879113,-6.73945089012744));
#40357=CARTESIAN_POINT('Ctrl Pts',(97.7036973559032,-0.841532200870129,
-6.818450725975));
#40358=CARTESIAN_POINT('Ctrl Pts',(96.4349636472737,-1.50103708992925,-6.89745056182257));
#40359=CARTESIAN_POINT('Ctrl Pts',(95.1893794356358,-0.798789346020887,
-6.97645039767013));
#40360=CARTESIAN_POINT('Ctrl Pts',(95.0969484971525,0.6281263640745,-7.0554502335177));
#40361=CARTESIAN_POINT('Ctrl Pts',(96.2415249049123,1.48520090511852,-7.13445006936525));
#40362=CARTESIAN_POINT('Ctrl Pts',(97.5847399554654,0.994889524388842,-7.21344990521282));
#40363=CARTESIAN_POINT('Ctrl Pts',(97.9080184090637,-0.39799344397038,-7.29244974106037));
#40364=CARTESIAN_POINT('Ctrl Pts',(96.9180795144695,-1.4298136352226,-7.37144957690794));
#40365=CARTESIAN_POINT('Ctrl Pts',(95.5130036090947,-1.16449567080877,-7.45044941275551));
#40366=CARTESIAN_POINT('Ctrl Pts',(94.9674865858653,0.157261908883212,-7.52944924860306));
#40367=CARTESIAN_POINT('Ctrl Pts',(95.7764257712339,1.33635025013728,-7.60844908445063));
#40368=CARTESIAN_POINT('Ctrl Pts',(97.2059451850679,1.30309115247707,-7.68744892029819));
#40369=CARTESIAN_POINT('Ctrl Pts',(97.9591735916556,0.0876575304244177,
-7.76644875614576));
#40370=CARTESIAN_POINT('Ctrl Pts',(97.3527762667723,-1.20729969144816,-7.84544859199331));
#40371=CARTESIAN_POINT('Ctrl Pts',(95.9368816245161,-1.40698515445507,-7.92444842784087));
#40372=CARTESIAN_POINT('Ctrl Pts',(94.9960004008529,-0.330242638778592,
-8.00344826368845));
#40373=CARTESIAN_POINT('Ctrl Pts',(95.3837074289611,1.04609859160552,-8.082448099536));
#40374=CARTESIAN_POINT('Ctrl Pts',(96.7482718489681,1.47341096653177,-8.16144793538358));
#40375=CARTESIAN_POINT('Ctrl Pts',(97.8517501055313,0.56403334452648,-8.24044777123112));
#40376=CARTESIAN_POINT('Ctrl Pts',(97.6930580606508,-0.857039755969165,
-8.31944760707869));
#40377=CARTESIAN_POINT('Ctrl Pts',(96.4161623833438,-1.50059966107122,-8.39844744292626));
#40378=CARTESIAN_POINT('Ctrl Pts',(95.179472857312,-0.782803772029945,-8.47744727877381));
#40379=CARTESIAN_POINT('Ctrl Pts',(95.1049239300038,0.645157844829405,-8.55644711462139));
#40380=CARTESIAN_POINT('Ctrl Pts',(96.2601469737666,1.48782719984968,-8.63544695046894));
#40381=CARTESIAN_POINT('Ctrl Pts',(97.5971145730019,0.980728037363569,-8.71444678631651));
#40382=CARTESIAN_POINT('Ctrl Pts',(97.9029192255884,-0.416095299490275,
-8.79344662216406));
#40383=CARTESIAN_POINT('Ctrl Pts',(96.9001325483008,-1.43543371584626,-8.87244645801162));
#40384=CARTESIAN_POINT('Ctrl Pts',(95.4984904907437,-1.15253539122406,-8.95144629385919));
#40385=CARTESIAN_POINT('Ctrl Pts',(94.9695737265171,0.175952081182726,-9.03044612970675));
#40386=CARTESIAN_POINT('Ctrl Pts',(95.7932197078309,1.34481445972806,-9.10944596555432));
#40387=CARTESIAN_POINT('Ctrl Pts',(97.2222103120731,1.29365057125066,-9.18844580140188));
#40388=CARTESIAN_POINT('Ctrl Pts',(97.9601540864565,0.0688767881518556,
-9.26744563724945));
#40389=CARTESIAN_POINT('Ctrl Pts',(97.3375825611522,-1.21838267655828,-9.34644547309699));
#40390=CARTESIAN_POINT('Ctrl Pts',(95.9192976768465,-1.40031557814065,-9.42544530894457));
#40391=CARTESIAN_POINT('Ctrl Pts',(94.9919782916159,-0.31187165126773,-9.50444514479212));
#40392=CARTESIAN_POINT('Ctrl Pts',(95.3968964695879,1.05950558679262,-9.58344498063969));
#40393=CARTESIAN_POINT('Ctrl Pts',(96.766706008181,1.4696892681371,-9.66244481648726));
#40394=CARTESIAN_POINT('Ctrl Pts',(97.8587074007407,0.546562785148768,-9.7414446523348));
#40395=CARTESIAN_POINT('Ctrl Pts',(97.68222357279,-0.872416584351429,-9.82044448818239));
#40396=CARTESIAN_POINT('Ctrl Pts',(96.3973715462248,-1.49991934260912,-9.89944432402992));
#40397=CARTESIAN_POINT('Ctrl Pts',(95.1697604815257,-0.766709904223744,
-9.97844415987751));
#40398=CARTESIAN_POINT('Ctrl Pts',(95.113125498743,0.662116678280016,-10.0574439957251));
#40399=CARTESIAN_POINT('Ctrl Pts',(96.2787741235636,1.49016381068195,-10.1364438315726));
#40400=CARTESIAN_POINT('Ctrl Pts',(97.6093626221807,0.966523110216778,-10.2154436674202));
#40401=CARTESIAN_POINT('Ctrl Pts',(97.8974918691158,-0.43434903833823,-10.2944435032678));
#40402=CARTESIAN_POINT('Ctrl Pts',(96.8823167554179,-1.44040079614298,-10.3734433391153));
#40403=CARTESIAN_POINT('Ctrl Pts',(95.4837341853858,-1.14124506615788,-10.4524431749629));
#40404=CARTESIAN_POINT('Ctrl Pts',(94.9726781721285,0.196400159027038,-10.5314430108104));
#40405=CARTESIAN_POINT('Ctrl Pts',(95.5299087207281,0.964251148760358,-10.5841095680422));
#40406=CARTESIAN_POINT('Ctrl Pts',(95.9093442884325,1.1466298417671,-10.610442846658));
#40407=CARTESIAN_POINT('Ctrl Pts',(95.7772565821794,-0.95676571636586,-0.00118268688497079));
#40408=CARTESIAN_POINT('Ctrl Pts',(95.4605674478988,-0.730627682766301,
-0.0275223413239983));
#40409=CARTESIAN_POINT('Ctrl Pts',(95.0747639166813,0.0568396289661587,
-0.0801952743788798));
#40410=CARTESIAN_POINT('Ctrl Pts',(95.7520483255391,1.19379006350773,-0.159201486049616));
#40411=CARTESIAN_POINT('Ctrl Pts',(97.0727632643449,1.24454744834932,-0.238201321897178));
#40412=CARTESIAN_POINT('Ctrl Pts',(97.8376034789184,0.167752758640745,-0.317201157744741));
#40413=CARTESIAN_POINT('Ctrl Pts',(97.3533151348387,-1.06199217367905,-0.396200993592303));
#40414=CARTESIAN_POINT('Ctrl Pts',(96.0589348237986,-1.32790139441603,-0.475200829439865));
#40415=CARTESIAN_POINT('Ctrl Pts',(95.1288941394749,-0.389325460524031,
-0.554200665287428));
#40416=CARTESIAN_POINT('Ctrl Pts',(95.4068520745854,0.902550032438413,-0.633200501134991));
#40417=CARTESIAN_POINT('Ctrl Pts',(96.6406843334901,1.37557394241651,-0.712200336982554));
#40418=CARTESIAN_POINT('Ctrl Pts',(97.7110275767741,0.600692376110241,-0.791200172830115));
#40419=CARTESIAN_POINT('Ctrl Pts',(97.6468687095074,-0.719155261321492,
-0.870200008677678));
#40420=CARTESIAN_POINT('Ctrl Pts',(96.5064077160413,-1.38657286711812,-0.949199844525241));
#40421=CARTESIAN_POINT('Ctrl Pts',(95.3242825335359,-0.796084107070757,
-1.0281996803728));
#40422=CARTESIAN_POINT('Ctrl Pts',(95.1729249993416,0.516620148098217,-1.10719951622037));
#40423=CARTESIAN_POINT('Ctrl Pts',(96.189648573922,1.36064166197053,-1.18619935206792));
#40424=CARTESIAN_POINT('Ctrl Pts',(97.4520732830183,0.970278828633655,-1.26519918791549));
#40425=CARTESIAN_POINT('Ctrl Pts',(97.8149177046067,-0.300328805516186,
-1.34419902376305));
#40426=CARTESIAN_POINT('Ctrl Pts',(96.9490064361857,-1.29847567252962,-1.42319885961061));
#40427=CARTESIAN_POINT('Ctrl Pts',(95.639901026997,-1.1186352742373,-1.50219869545818));
#40428=CARTESIAN_POINT('Ctrl Pts',(95.0752321578856,0.0760398577476157,
-1.58119853130574));
#40429=CARTESIAN_POINT('Ctrl Pts',(95.7672718726961,1.2017310183888,-1.6601983671533));
#40430=CARTESIAN_POINT('Ctrl Pts',(97.0881963024602,1.23720237191416,-1.73919820300086));
#40431=CARTESIAN_POINT('Ctrl Pts',(97.839652436839,0.150274016097634,-1.81819803884842));
#40432=CARTESIAN_POINT('Ctrl Pts',(97.3399133692319,-1.072984104931,-1.89719787469599));
#40433=CARTESIAN_POINT('Ctrl Pts',(96.0423463061713,-1.32282262275537,-1.97619771054355));
#40434=CARTESIAN_POINT('Ctrl Pts',(95.1241142743353,-0.372586070909921,
-2.05519754639111));
#40435=CARTESIAN_POINT('Ctrl Pts',(95.4182445824703,0.915663489455976,-2.13419738223868));
#40436=CARTESIAN_POINT('Ctrl Pts',(96.6578999056424,1.37321594324093,-2.21319721808624));
#40437=CARTESIAN_POINT('Ctrl Pts',(97.7184552019094,0.584976111817808,-2.2921970539338));
#40438=CARTESIAN_POINT('Ctrl Pts',(97.6377663798092,-0.733958640991776,
-2.37119688978136));
#40439=CARTESIAN_POINT('Ctrl Pts',(96.4890349722712,-1.38704035223526,-2.45019672562893));
#40440=CARTESIAN_POINT('Ctrl Pts',(95.3143991311586,-0.781788165952468,
-2.52919656147649));
#40441=CARTESIAN_POINT('Ctrl Pts',(95.1794977138653,0.532708382474514,-2.60819639732405));
#40442=CARTESIAN_POINT('Ctrl Pts',(96.2067143453001,1.36392770390827,-2.68719623317162));
#40443=CARTESIAN_POINT('Ctrl Pts',(97.4641500325143,0.957781103848562,-2.76619606901917));
#40444=CARTESIAN_POINT('Ctrl Pts',(97.8110492476535,-0.317272033379287,
-2.84519590486674));
#40445=CARTESIAN_POINT('Ctrl Pts',(96.9327022991588,-1.30449349095085,-2.9241957407143));
#40446=CARTESIAN_POINT('Ctrl Pts',(95.6259524348061,-1.10826821165649,-3.00319557656186));
#40447=CARTESIAN_POINT('Ctrl Pts',(95.0762933911271,0.0933866905184069,
-3.08219541240942));
#40448=CARTESIAN_POINT('Ctrl Pts',(95.7823801680448,1.21032045385489,-3.16119524825699));
#40449=CARTESIAN_POINT('Ctrl Pts',(97.1036452978925,1.22924199895298,-3.24019508410455));
#40450=CARTESIAN_POINT('Ctrl Pts',(97.8414266813184,0.132985551542359,-3.31919491995211));
#40451=CARTESIAN_POINT('Ctrl Pts',(97.3264032547896,-1.08391643232731,-3.39819475579968));
#40452=CARTESIAN_POINT('Ctrl Pts',(96.0258083144189,-1.31748091871516,-3.47719459164724));
#40453=CARTESIAN_POINT('Ctrl Pts',(95.1195518013773,-0.355816371802199,
-3.5561944274948));
#40454=CARTESIAN_POINT('Ctrl Pts',(95.4297967395223,0.928647581204988,-3.63519426334236));
#40455=CARTESIAN_POINT('Ctrl Pts',(96.675086485165,1.37063515751958,-3.71419409918992));
#40456=CARTESIAN_POINT('Ctrl Pts',(97.7256844040054,0.569171757763991,-3.79319393503749));
#40457=CARTESIAN_POINT('Ctrl Pts',(97.6284798155882,-0.748648729332052,
-3.87219377088505));
#40458=CARTESIAN_POINT('Ctrl Pts',(96.4716574857007,-1.38728921136657,-3.95119360673261));
#40459=CARTESIAN_POINT('Ctrl Pts',(95.3046957144924,-0.76737002892615,-4.03019344258017));
#40460=CARTESIAN_POINT('Ctrl Pts',(95.1862713828854,0.548713268552738,-4.10919327842774));
#40461=CARTESIAN_POINT('Ctrl Pts',(96.2238199742907,1.36699958072789,-4.1881931142753));
#40462=CARTESIAN_POINT('Ctrl Pts',(97.4760692605543,0.94513314064201,-4.26719295012286));
#40463=CARTESIAN_POINT('Ctrl Pts',(97.806968857485,-0.334165505089595,-4.34619278597042));
#40464=CARTESIAN_POINT('Ctrl Pts',(96.9163240527783,-1.31030658099452,-4.42519262181799));
#40465=CARTESIAN_POINT('Ctrl Pts',(95.6121348059199,-1.09772723910617,-4.50419245766555));
#40466=CARTESIAN_POINT('Ctrl Pts',(95.0775718411454,0.110718872605577,-4.58319229351311));
#40467=CARTESIAN_POINT('Ctrl Pts',(95.7975948770745,1.21871995381048,-4.66219212936068));
#40468=CARTESIAN_POINT('Ctrl Pts',(97.118993362447,1.22108872447091,-4.74119196520824));
#40469=CARTESIAN_POINT('Ctrl Pts',(97.8429842167332,0.115676217245968,-4.8201918010558));
#40470=CARTESIAN_POINT('Ctrl Pts',(97.3127572527077,-1.09467866246482,-4.89919163690336));
#40471=CARTESIAN_POINT('Ctrl Pts',(96.0093385350669,-1.31193246501631,-4.97819147275094));
#40472=CARTESIAN_POINT('Ctrl Pts',(95.1151997578914,-0.338990835024778,
-5.05719130859848));
#40473=CARTESIAN_POINT('Ctrl Pts',(95.4415106399219,0.941485941995406,-5.13619114444606));
#40474=CARTESIAN_POINT('Ctrl Pts',(96.6922393870391,1.36783928061704,-5.21519098029361));
#40475=CARTESIAN_POINT('Ctrl Pts',(97.7327150601027,0.553278084645531,-5.29419081614118));
#40476=CARTESIAN_POINT('Ctrl Pts',(97.6190099594978,-0.76322133362851,-5.37319065198874));
#40477=CARTESIAN_POINT('Ctrl Pts',(96.4542782452181,-1.38732036581045,-5.4521904878363));
#40478=CARTESIAN_POINT('Ctrl Pts',(95.2951736730316,-0.752831469961364,
-5.53119032368387));
#40479=CARTESIAN_POINT('Ctrl Pts',(95.1932450112196,0.564632046087808,-5.61019015953143));
#40480=CARTESIAN_POINT('Ctrl Pts',(96.2409627420432,1.36985693687148,-5.689189995379));
#40481=CARTESIAN_POINT('Ctrl Pts',(97.4878291142287,0.9323368594669,-5.76818983122655));
#40482=CARTESIAN_POINT('Ctrl Pts',(97.8026771654983,-0.351006536834826,
-5.84718966707411));
#40483=CARTESIAN_POINT('Ctrl Pts',(96.8998742717961,-1.31591404708784,-5.92618950292167));
#40484=CARTESIAN_POINT('Ctrl Pts',(95.5984503064001,-1.08701400228222,-6.00518933876924));
#40485=CARTESIAN_POINT('Ctrl Pts',(95.0790673084927,0.128033679788049,-6.0841891746168));
#40486=CARTESIAN_POINT('Ctrl Pts',(95.81291361157,1.22692820233305,-6.16318901046438));
#40487=CARTESIAN_POINT('Ctrl Pts',(97.1342380878854,1.21274382682907,-6.24218884631192));
#40488=CARTESIAN_POINT('Ctrl Pts',(97.8443247985074,0.0983487300980883,
-6.32118868215949));
#40489=CARTESIAN_POINT('Ctrl Pts',(97.2989775045063,-1.10526910673613,-6.40018851800705));
#40490=CARTESIAN_POINT('Ctrl Pts',(95.9929395526466,-1.30617813222014,-6.47918835385461));
#40491=CARTESIAN_POINT('Ctrl Pts',(95.1110588268558,-0.322112101052384,
-6.55818818970217));
#40492=CARTESIAN_POINT('Ctrl Pts',(95.4533844454178,0.954176557165478,-6.63718802554975));
#40493=CARTESIAN_POINT('Ctrl Pts',(96.7093559194969,1.3648287512656,-6.71618786139731));
#40494=CARTESIAN_POINT('Ctrl Pts',(97.7395460668907,0.537297586636558,-6.79518769724487));
#40495=CARTESIAN_POINT('Ctrl Pts',(97.6093582976261,-0.777674167034751,
-6.87418753309242));
#40496=CARTESIAN_POINT('Ctrl Pts',(96.4368999781142,-1.38713381067534,-6.95318736893999));
#40497=CARTESIAN_POINT('Ctrl Pts',(95.2858345010529,-0.738174770568153,
-7.03218720478755));
#40498=CARTESIAN_POINT('Ctrl Pts',(95.200417504509,0.580462216976517,-7.11118704063511));
#40499=CARTESIAN_POINT('Ctrl Pts',(96.2581399583757,1.37249932393917,-7.19018687648268));
#40500=CARTESIAN_POINT('Ctrl Pts',(97.4994277480854,0.919394268419785,-7.26918671233024));
#40501=CARTESIAN_POINT('Ctrl Pts',(97.7981748451804,-0.367792485783587,
-7.3481865481778));
#40502=CARTESIAN_POINT('Ctrl Pts',(96.8833555376452,-1.32131500926161,-7.42718638402537));
#40503=CARTESIAN_POINT('Ctrl Pts',(95.5849010837298,-1.07613018239279,-7.50618621987292));
#40504=CARTESIAN_POINT('Ctrl Pts',(95.0807795584877,0.145328394885655,-7.5851860557205));
#40505=CARTESIAN_POINT('Ctrl Pts',(95.8283339675914,1.23494391131751,-7.66418589156805));
#40506=CARTESIAN_POINT('Ctrl Pts',(97.1493770818821,1.2042086155766,-7.74318572741561));
#40507=CARTESIAN_POINT('Ctrl Pts',(97.8454482162656,0.0810058092686688,
-7.82218556326319));
#40508=CARTESIAN_POINT('Ctrl Pts',(97.2850661726159,-1.11568610320255,-7.90118539911075));
#40509=CARTESIAN_POINT('Ctrl Pts',(95.9766139406194,-1.30021882334358,-7.9801852349583));
#40510=CARTESIAN_POINT('Ctrl Pts',(95.1071296580992,-0.305182818632427,
-8.05918507080586));
#40511=CARTESIAN_POINT('Ctrl Pts',(95.4654162926759,0.966717435199593,-8.13818490665342));
#40512=CARTESIAN_POINT('Ctrl Pts',(96.7264333964741,1.36160404190438,-8.217184742501));
#40513=CARTESIAN_POINT('Ctrl Pts',(97.7461763523901,0.521232771521885,-8.29618457834855));
#40514=CARTESIAN_POINT('Ctrl Pts',(97.5995263445948,-0.792004961485537,
-8.37518441419613));
#40515=CARTESIAN_POINT('Ctrl Pts',(96.4195254115195,-1.38672957525517,-8.45418425004368));
#40516=CARTESIAN_POINT('Ctrl Pts',(95.2766796641515,-0.72340223075907,-8.53318408589125));
#40517=CARTESIAN_POINT('Ctrl Pts',(95.207787737155,0.596201296949623,-8.6121839217388));
#40518=CARTESIAN_POINT('Ctrl Pts',(96.2753489277647,1.37492632740421,-8.69118375758637));
#40519=CARTESIAN_POINT('Ctrl Pts',(97.5108633418452,0.906307398285803,-8.77018359343392));
#40520=CARTESIAN_POINT('Ctrl Pts',(97.7934626033228,-0.384520717215092,
-8.84918342928149));
#40521=CARTESIAN_POINT('Ctrl Pts',(96.866770442088,-1.32650862100118,-8.92818326512905));
#40522=CARTESIAN_POINT('Ctrl Pts',(95.5714892651293,-1.06507748535526,-9.00718310097661));
#40523=CARTESIAN_POINT('Ctrl Pts',(95.0827083205317,0.162600299822547,-9.0861829368242));
#40524=CARTESIAN_POINT('Ctrl Pts',(95.8438535289828,1.24276583083088,-9.16518277267173));
#40525=CARTESIAN_POINT('Ctrl Pts',(97.1644079613688,1.19548441448961,-9.24418260851932));
#40526=CARTESIAN_POINT('Ctrl Pts',(97.8463543081263,0.063650207084928,-9.32318244436686));
#40527=CARTESIAN_POINT('Ctrl Pts',(97.2710254117867,-1.12592807754988,-9.40218228021444));
#40528=CARTESIAN_POINT('Ctrl Pts',(95.9603643166085,-1.29405535485191,-9.48118211606198));
#40529=CARTESIAN_POINT('Ctrl Pts',(95.1034127587967,-0.288205877767486,
-9.56018195190957));
#40530=CARTESIAN_POINT('Ctrl Pts',(95.4776045086144,0.979107066640665,-9.63918178775711));
#40531=CARTESIAN_POINT('Ctrl Pts',(96.7434687153796,1.3581647573517,-9.71818162360469));
#40532=CARTESIAN_POINT('Ctrl Pts',(97.7526057067882,0.505087931553021,-9.79718145945224));
#40533=CARTESIAN_POINT('Ctrl Pts',(97.5895140107666,-0.806214949162121,
-9.8761812952998));
#40534=CARTESIAN_POINT('Ctrl Pts',(96.4021604805168,-1.38610088143599,-9.95518113114737));
#40535=CARTESIAN_POINT('Ctrl Pts',(95.2677042931061,-0.70852961480021,-10.0341809669949));
#40536=CARTESIAN_POINT('Ctrl Pts',(95.2153669458066,0.611873242317784,-10.1131808028425));
#40537=CARTESIAN_POINT('Ctrl Pts',(96.2925625925392,1.37708562906941,-10.1921806386901));
#40538=CARTESIAN_POINT('Ctrl Pts',(97.522181971641,0.893180384399409,-10.2711804745376));
#40539=CARTESIAN_POINT('Ctrl Pts',(97.788447091237,-0.401389306603797,-10.3501803103852));
#40540=CARTESIAN_POINT('Ctrl Pts',(96.8503065659866,-1.33109878407321,-10.4291801462327));
#40541=CARTESIAN_POINT('Ctrl Pts',(95.5578527132946,-1.05464390464104,-10.5081799820803));
#40542=CARTESIAN_POINT('Ctrl Pts',(95.0855771913276,0.181496715062028,-10.5871798179279));
#40543=CARTESIAN_POINT('Ctrl Pts',(95.6005233838565,0.891080826317942,-10.6398463751596));
#40544=CARTESIAN_POINT('Ctrl Pts',(95.9511662217095,1.05962006702942,-10.6661796537754));
#40545=CARTESIAN_POINT('',(95.7749081866277,-0.958725441828032,-10.5005139401467));
#40546=CARTESIAN_POINT('Ctrl Pts',(95.7743417034713,-0.959424604812491,
-10.5));
#40547=CARTESIAN_POINT('Ctrl Pts',(95.743761931704,-0.942816466443102,-10.5));
#40548=CARTESIAN_POINT('Ctrl Pts',(95.7140522834952,-0.924824833399416,
-10.5));
#40549=CARTESIAN_POINT('Ctrl Pts',(95.6853187497364,-0.905478391503427,
-10.5));
#40550=CARTESIAN_POINT('Ctrl Pts',(95.6455067847734,-0.878672782649827,
-10.5));
#40551=CARTESIAN_POINT('Ctrl Pts',(95.6075673391679,-0.849268629040611,
-10.5));
#40552=CARTESIAN_POINT('Ctrl Pts',(95.571561890951,-0.817569321508675,-10.5));
#40553=CARTESIAN_POINT('Ctrl Pts',(95.53699301791,-0.787134779187252,-10.5));
#40554=CARTESIAN_POINT('Ctrl Pts',(95.5042065672641,-0.754583714502893,
-10.5));
#40555=CARTESIAN_POINT('Ctrl Pts',(95.4732743966275,-0.720145741921755,
-10.5));
#40556=CARTESIAN_POINT('Ctrl Pts',(95.4565243447733,-0.701497266414933,
-10.5));
#40557=CARTESIAN_POINT('Ctrl Pts',(95.4403183608167,-0.682294881829244,
-10.5));
#40558=CARTESIAN_POINT('Ctrl Pts',(95.42467063047,-0.662571296003026,-10.5));
#40559=CARTESIAN_POINT('Ctrl Pts',(95.4184263768185,-0.654700565226925,
-10.5));
#40560=CARTESIAN_POINT('Ctrl Pts',(95.4122761815382,-0.646753210694079,
-10.5));
#40561=CARTESIAN_POINT('Ctrl Pts',(95.4062240468848,-0.638736400192628,
-10.5));
#40562=CARTESIAN_POINT('Ctrl Pts',(95.3752933609304,-0.597764831948361,
-10.5));
#40563=CARTESIAN_POINT('Ctrl Pts',(95.3468925649399,-0.554945957420721,
-10.5));
#40564=CARTESIAN_POINT('Ctrl Pts',(95.3210948996399,-0.51060962610373,-10.5));
#40565=CARTESIAN_POINT('Ctrl Pts',(95.2946242490595,-0.465116690186564,
-10.5));
#40566=CARTESIAN_POINT('Ctrl Pts',(95.2708935368424,-0.41802532548798,-10.5));
#40567=CARTESIAN_POINT('Ctrl Pts',(95.250013584509,-0.369646938464868,-10.5));
#40568=CARTESIAN_POINT('Ctrl Pts',(95.2305984415717,-0.324662482363928,
-10.5));
#40569=CARTESIAN_POINT('Ctrl Pts',(95.2136479739893,-0.27856414950988,-10.5));
#40570=CARTESIAN_POINT('Ctrl Pts',(95.1992838987357,-0.231578413904824,
-10.5));
#40571=CARTESIAN_POINT('Ctrl Pts',(95.1963990144411,-0.22214178757666,-10.5));
#40572=CARTESIAN_POINT('Ctrl Pts',(95.1936212162796,-0.212677871502264,
-10.5));
#40573=CARTESIAN_POINT('Ctrl Pts',(95.1909519508877,-0.203191933881503,
-10.5));
#40574=CARTESIAN_POINT('Ctrl Pts',(95.1762463098862,-0.150931565302911,
-10.5));
#40575=CARTESIAN_POINT('Ctrl Pts',(95.1648222691944,-0.0979747821329156,
-10.5));
#40576=CARTESIAN_POINT('Ctrl Pts',(95.1567822801157,-0.044653796014109,
-10.5));
#40577=CARTESIAN_POINT('Ctrl Pts',(95.1487886315547,0.0083598610667158,
-10.5));
#40578=CARTESIAN_POINT('Ctrl Pts',(95.1441395215139,0.0617346236555578,
-10.5));
#40579=CARTESIAN_POINT('Ctrl Pts',(95.1429788547342,0.115170238925761,-10.5));
#40580=CARTESIAN_POINT('Ctrl Pts',(95.1425638222925,0.134277802153374,-10.5));
#40581=CARTESIAN_POINT('Ctrl Pts',(95.1425952849307,0.153393312536775,-10.5));
#40582=CARTESIAN_POINT('Ctrl Pts',(95.1430814086749,0.172503453148985,-10.5));
#40583=CARTESIAN_POINT('Ctrl Pts',(95.1435523124352,0.191015276902803,-10.5));
#40584=CARTESIAN_POINT('Ctrl Pts',(95.1444498564248,0.209522067576187,-10.5));
#40585=CARTESIAN_POINT('Ctrl Pts',(95.145766583077,0.228014411035019,-10.5));
#40586=CARTESIAN_POINT('Ctrl Pts',(95.146666979761,0.240659742321974,-10.5));
#40587=CARTESIAN_POINT('Ctrl Pts',(95.1477634041437,0.253298319323364,-10.5));
#40588=CARTESIAN_POINT('Ctrl Pts',(95.1490536859085,0.265927131090289,-10.5));
#40589=CARTESIAN_POINT('Ctrl Pts',(95.1500570571513,0.275747766322456,-10.5));
#40590=CARTESIAN_POINT('Ctrl Pts',(95.1511771699739,0.285557082169919,-10.5));
#40591=CARTESIAN_POINT('Ctrl Pts',(95.1524115154242,0.295345846772921,-10.5));
#40592=CARTESIAN_POINT('Ctrl Pts',(95.1590576930707,0.348052217159999,-10.5));
#40593=CARTESIAN_POINT('Ctrl Pts',(95.1690182934861,0.400230513827266,-10.5));
#40594=CARTESIAN_POINT('Ctrl Pts',(95.1820544730012,0.451656851506956,-10.5));
#40595=CARTESIAN_POINT('Ctrl Pts',(95.1955365881926,0.504842357864085,-10.5));
#40596=CARTESIAN_POINT('Ctrl Pts',(95.2123083596628,0.557224436802563,-10.5));
#40597=CARTESIAN_POINT('Ctrl Pts',(95.2321614793495,0.608561995447114,-10.5));
#40598=CARTESIAN_POINT('Ctrl Pts',(95.2464121121572,0.645412259235966,-10.5));
#40599=CARTESIAN_POINT('Ctrl Pts',(95.2622515842379,0.681724527967293,-10.5));
#40600=CARTESIAN_POINT('Ctrl Pts',(95.2796192182905,0.717407656638586,-10.5));
#40601=CARTESIAN_POINT('Ctrl Pts',(95.2866053987556,0.731761297192127,-10.5));
#40602=CARTESIAN_POINT('Ctrl Pts',(95.2938389938601,0.746013100506293,-10.5));
#40603=CARTESIAN_POINT('Ctrl Pts',(95.3013166297465,0.760156939120319,-10.5));
#40604=CARTESIAN_POINT('Ctrl Pts',(95.3063377624319,0.7696543379561,-10.5));
#40605=CARTESIAN_POINT('Ctrl Pts',(95.3114688717837,0.779102706153686,-10.5));
#40606=CARTESIAN_POINT('Ctrl Pts',(95.3167019374426,0.788488138842627,-10.5));
#40607=CARTESIAN_POINT('Ctrl Pts',(95.3444794956177,0.838306814836282,-10.5));
#40608=CARTESIAN_POINT('Ctrl Pts',(95.3751713649573,0.886440870645454,-10.5));
#40609=CARTESIAN_POINT('Ctrl Pts',(95.4085627630981,0.932633649457067,-10.5));
#40610=CARTESIAN_POINT('Ctrl Pts',(95.4365439625058,0.971342102145167,-10.5));
#40611=CARTESIAN_POINT('Ctrl Pts',(95.4664218796374,1.00868767887304,-10.5));
#40612=CARTESIAN_POINT('Ctrl Pts',(95.4980964137371,1.0445113235797,-10.5));
#40613=CARTESIAN_POINT('Ctrl Pts',(95.5067327648042,1.05427896755563,-10.5));
#40614=CARTESIAN_POINT('Ctrl Pts',(95.5155028091272,1.06393340204177,-10.5));
#40615=CARTESIAN_POINT('Ctrl Pts',(95.5244047958277,1.07347123922404,-10.5));
#40616=CARTESIAN_POINT('Ctrl Pts',(95.5330197495047,1.0827015412082,-10.5));
#40617=CARTESIAN_POINT('Ctrl Pts',(95.5417528075879,1.09181672209954,-10.5));
#40618=CARTESIAN_POINT('Ctrl Pts',(95.5505984710309,1.10081064316732,-10.5));
#40619=CARTESIAN_POINT('Ctrl Pts',(95.5918901186315,1.14279435887975,-10.5));
#40620=CARTESIAN_POINT('Ctrl Pts',(95.6356542695399,1.18216184934901,-10.5));
#40621=CARTESIAN_POINT('Ctrl Pts',(95.6816922111834,1.2186319374679,-10.5));
#40622=CARTESIAN_POINT('Ctrl Pts',(95.7277301528269,1.25510202558684,-10.5));
#40623=CARTESIAN_POINT('Ctrl Pts',(95.7760424196809,1.28867583950039,-10.5));
#40624=CARTESIAN_POINT('Ctrl Pts',(95.8264738550018,1.31904027763685,-10.5));
#40625=CARTESIAN_POINT('Ctrl Pts',(95.7870390291235,-0.966214801312805,
-10.4999999999999));
#40626=CARTESIAN_POINT('Ctrl Pts',(95.7831492272154,-0.963503648819942,
-10.5001713133822));
#40627=CARTESIAN_POINT('Ctrl Pts',(95.7792757974046,-0.960769006609016,
-10.5003426267644));
#40628=CARTESIAN_POINT('Ctrl Pts',(95.7754190221833,-0.958011074119503,
-10.5005139401467));
#40629=CARTESIAN_POINT('Ctrl Pts',(95.8249089770643,1.32073714597366,1.47379938114645E-14));
#40630=CARTESIAN_POINT('Ctrl Pts',(95.7882096295246,1.29890519325284,2.47546172164436E-14));
#40631=CARTESIAN_POINT('Ctrl Pts',(95.7526292179146,1.27542989100163,4.25615003845605E-15));
#40632=CARTESIAN_POINT('Ctrl Pts',(95.7182919635207,1.25031227307591,9.89139326001975E-15));
#40633=CARTESIAN_POINT('Ctrl Pts',(95.6717202412518,1.21624517170915,1.73698872156513E-14));
#40634=CARTESIAN_POINT('Ctrl Pts',(95.6274334991323,1.17915789839703,9.97151118260645E-16));
#40635=CARTESIAN_POINT('Ctrl Pts',(95.585565943421,1.1393743846506,6.57807142090405E-15));
#40636=CARTESIAN_POINT('Ctrl Pts',(95.5491852857017,1.10480464749038,1.1427591481002E-14));
#40637=CARTESIAN_POINT('Ctrl Pts',(95.5146317052295,1.06819794712208,6.30435606573601E-15));
#40638=CARTESIAN_POINT('Ctrl Pts',(95.4820208735387,1.02975084482163,6.20337115009306E-15));
#40639=CARTESIAN_POINT('Ctrl Pts',(95.4671764842234,1.01224979609028,6.07670337588304E-15));
#40640=CARTESIAN_POINT('Ctrl Pts',(95.4527350160314,0.994367261227605,1.23663649028217E-14));
#40641=CARTESIAN_POINT('Ctrl Pts',(95.4387093357306,0.976121279115226,1.82250048386123E-14));
#40642=CARTESIAN_POINT('Ctrl Pts',(95.4322004051361,0.967653823087995,2.0923811005169E-14));
#40643=CARTESIAN_POINT('Ctrl Pts',(95.4257810378785,0.959108091365199,2.27073921460578E-14));
#40644=CARTESIAN_POINT('Ctrl Pts',(95.419452614983,0.950485878413156,8.29891710907305E-15));
#40645=CARTESIAN_POINT('Ctrl Pts',(95.4129727980227,0.941657397345356,-6.60253895520359E-15));
#40646=CARTESIAN_POINT('Ctrl Pts',(95.4065928858365,0.932754851908662,1.77479395350164E-16));
#40647=CARTESIAN_POINT('Ctrl Pts',(95.4003179024342,0.923786314242425,3.69843045078255E-15));
#40648=CARTESIAN_POINT('Ctrl Pts',(95.3677308770152,0.877211216563209,2.16423796791319E-14));
#40649=CARTESIAN_POINT('Ctrl Pts',(95.3379338541689,0.828809305904207,1.19539479630578E-14));
#40650=CARTESIAN_POINT('Ctrl Pts',(95.3110606737817,0.77888382467263,8.24340595784179E-15));
#40651=CARTESIAN_POINT('Ctrl Pts',(95.2843801273044,0.72931622220764,4.55946207774017E-15));
#40652=CARTESIAN_POINT('Ctrl Pts',(95.2605813437002,0.678245682189612,-5.6098006835629E-15));
#40653=CARTESIAN_POINT('Ctrl Pts',(95.2398443953752,0.625955786165572,-1.25247034965525E-14));
#40654=CARTESIAN_POINT('Ctrl Pts',(95.2218459942583,0.580571358898283,-1.84710252423929E-14));
#40655=CARTESIAN_POINT('Ctrl Pts',(95.2061547434338,0.534267750929017,7.33456568098874E-15));
#40656=CARTESIAN_POINT('Ctrl Pts',(95.1929214733713,0.487231932453229,-1.0692835505921E-14));
#40657=CARTESIAN_POINT('Ctrl Pts',(95.1889192493455,0.473006583624943,-1.60992812190512E-14));
#40658=CARTESIAN_POINT('Ctrl Pts',(95.1851406834792,0.458707962306186,1.6491895291636E-14));
#40659=CARTESIAN_POINT('Ctrl Pts',(95.1815985241459,0.444375806041165,1.71807013060743E-14));
#40660=CARTESIAN_POINT('Ctrl Pts',(95.168691449557,0.392151670274027,1.95643296332385E-14));
#40661=CARTESIAN_POINT('Ctrl Pts',(95.158897674096,0.339415368628355,-4.77953976795929E-15));
#40662=CARTESIAN_POINT('Ctrl Pts',(95.1523649309639,0.286422180494928,-6.99440505513849E-15));
#40663=CARTESIAN_POINT('Ctrl Pts',(95.1459203851088,0.234144442946058,-9.17936788277064E-15));
#40664=CARTESIAN_POINT('Ctrl Pts',(95.1426492616811,0.1816158105116,-1.2022342687055E-14));
#40665=CARTESIAN_POINT('Ctrl Pts',(95.1427428232365,0.129086762469465,9.96425164601078E-15));
#40666=CARTESIAN_POINT('Ctrl Pts',(95.1427865748878,0.10452290626488,2.02972138732121E-14));
#40667=CARTESIAN_POINT('Ctrl Pts',(95.1435668137101,0.0799591192207672,
8.29095392627298E-15));
#40668=CARTESIAN_POINT('Ctrl Pts',(95.1451070256586,0.0554222538728419,
1.63619118254132E-14));
#40669=CARTESIAN_POINT('Ctrl Pts',(95.1469030423967,0.0268102041407893,
2.57643491551798E-14));
#40670=CARTESIAN_POINT('Ctrl Pts',(95.1497324600441,-0.00176532152798841,
2.28418772120502E-14));
#40671=CARTESIAN_POINT('Ctrl Pts',(95.1535760456806,-0.0302592959787804,
2.42444953002519E-14));
#40672=CARTESIAN_POINT('Ctrl Pts',(95.1551319527013,-0.041793831458969,
2.50559662492533E-14));
#40673=CARTESIAN_POINT('Ctrl Pts',(95.1568545835752,-0.0533170828206849,
9.15937163043892E-15));
#40674=CARTESIAN_POINT('Ctrl Pts',(95.1587387377557,-0.064803940851461,
1.1671219546372E-14));
#40675=CARTESIAN_POINT('Ctrl Pts',(95.1672789468338,-0.116869833466758,
2.27889665739075E-14));
#40676=CARTESIAN_POINT('Ctrl Pts',(95.1791453848401,-0.168288980706651,
-1.08395901568713E-14));
#40677=CARTESIAN_POINT('Ctrl Pts',(95.194147378263,-0.218805534067158,-1.06858966120171E-15));
#40678=CARTESIAN_POINT('Ctrl Pts',(95.2092083821131,-0.269520794580306,
8.71771805315145E-15));
#40679=CARTESIAN_POINT('Ctrl Pts',(95.2274304072348,-0.319327333795833,
-1.20151378749622E-14));
#40680=CARTESIAN_POINT('Ctrl Pts',(95.2486662510227,-0.367940603828083,
-1.25316423904565E-14));
#40681=CARTESIAN_POINT('Ctrl Pts',(95.2620753394337,-0.398636800424634,
-1.2922186424885E-14));
#40682=CARTESIAN_POINT('Ctrl Pts',(95.2766869482097,-0.428856661622077,
2.14493485157268E-14));
#40683=CARTESIAN_POINT('Ctrl Pts',(95.2924713193047,-0.458520632581111,
2.45081732686003E-14));
#40684=CARTESIAN_POINT('Ctrl Pts',(95.3008107067378,-0.474193055963875,
2.60243438444447E-14));
#40685=CARTESIAN_POINT('Ctrl Pts',(95.3094775372499,-0.489710195447915,
2.29976605015753E-15));
#40686=CARTESIAN_POINT('Ctrl Pts',(95.3184679272418,-0.505059462317017,
1.29479760246909E-14));
#40687=CARTESIAN_POINT('Ctrl Pts',(95.3242758264827,-0.514975271918048,
1.99495353990142E-14));
#40688=CARTESIAN_POINT('Ctrl Pts',(95.3302143331834,-0.524813350049739,
1.92471923790151E-14));
#40689=CARTESIAN_POINT('Ctrl Pts',(95.3362788672618,-0.534565975662569,
1.7125190154843E-14));
#40690=CARTESIAN_POINT('Ctrl Pts',(95.3635106434983,-0.578358510253512,
8.19581166695719E-15));
#40691=CARTESIAN_POINT('Ctrl Pts',(95.3932993713737,-0.620462763195338,
1.21772296880902E-14));
#40692=CARTESIAN_POINT('Ctrl Pts',(95.4255117600527,-0.660602238459277,
1.63757896132211E-15));
#40693=CARTESIAN_POINT('Ctrl Pts',(95.4506195460652,-0.691888752651906,
-6.61641427583824E-15));
#40694=CARTESIAN_POINT('Ctrl Pts',(95.4772006416695,-0.721981045963318,
9.76424046132771E-15));
#40695=CARTESIAN_POINT('Ctrl Pts',(95.5052033941774,-0.750728856696811,
1.41830991395864E-14));
#40696=CARTESIAN_POINT('Ctrl Pts',(95.5160198476517,-0.761833099295801,
1.584519613144E-14));
#40697=CARTESIAN_POINT('Ctrl Pts',(95.5270521274395,-0.77273972936565,-1.46751849299723E-15));
#40698=CARTESIAN_POINT('Ctrl Pts',(95.5382756714544,-0.783419267701306,
1.94289029309402E-15));
#40699=CARTESIAN_POINT('Ctrl Pts',(95.5740535630002,-0.817463003247418,
1.30361735751359E-14));
#40700=CARTESIAN_POINT('Ctrl Pts',(95.6118085679276,-0.849241382244103,
-8.74677678469814E-15));
#40701=CARTESIAN_POINT('Ctrl Pts',(95.6514318537012,-0.878485337795217,
-1.27675647831893E-15));
#40702=CARTESIAN_POINT('Ctrl Pts',(95.6910551394747,-0.90772929334633,6.2769800476697E-15));
#40703=CARTESIAN_POINT('Ctrl Pts',(95.7325473555912,-0.934439521706132,
8.70022739947829E-15));
#40704=CARTESIAN_POINT('Ctrl Pts',(95.7758165250375,-0.958295198918397,
1.22124532708767E-14));
#40705=CARTESIAN_POINT('Origin',(96.460480949577,-2.11854640757359E-15,
-10.5));
#40706=CARTESIAN_POINT('Origin',(96.460480949577,-8.32667268468867E-16,
1.18130019239114E-14));
#40707=CARTESIAN_POINT('',(0.,0.,0.));
#40708=CARTESIAN_POINT('',(0.,0.,0.));
#40709=CARTESIAN_POINT('',(0.,0.,0.));
#40710=CARTESIAN_POINT('',(0.,0.,0.));
#40711=CARTESIAN_POINT('',(0.,0.,0.));
#40712=CARTESIAN_POINT('',(0.,0.,0.));
#40713=CARTESIAN_POINT('',(0.,0.,0.));
#40714=CARTESIAN_POINT('',(0.,0.,0.));
#40715=UNCERTAINTY_MEASURE_WITH_UNIT(LENGTH_MEASURE(0.01),#40735,
'DISTANCE_ACCURACY_VALUE',
'Maximum model space distance between geometric entities at asserted c
onnectivities');
#40716=UNCERTAINTY_MEASURE_WITH_UNIT(LENGTH_MEASURE(0.01),#40735,
'DISTANCE_ACCURACY_VALUE',
'Maximum model space distance between geometric entities at asserted c
onnectivities');
#40717=UNCERTAINTY_MEASURE_WITH_UNIT(LENGTH_MEASURE(0.01),#40735,
'DISTANCE_ACCURACY_VALUE',
'Maximum model space distance between geometric entities at asserted c
onnectivities');
#40718=UNCERTAINTY_MEASURE_WITH_UNIT(LENGTH_MEASURE(0.01),#40735,
'DISTANCE_ACCURACY_VALUE',
'Maximum model space distance between geometric entities at asserted c
onnectivities');
#40719=UNCERTAINTY_MEASURE_WITH_UNIT(LENGTH_MEASURE(0.01),#40735,
'DISTANCE_ACCURACY_VALUE',
'Maximum model space distance between geometric entities at asserted c
onnectivities');
#40720=UNCERTAINTY_MEASURE_WITH_UNIT(LENGTH_MEASURE(0.01),#40735,
'DISTANCE_ACCURACY_VALUE',
'Maximum model space distance between geometric entities at asserted c
onnectivities');
#40721=UNCERTAINTY_MEASURE_WITH_UNIT(LENGTH_MEASURE(0.01),#40735,
'DISTANCE_ACCURACY_VALUE',
'Maximum model space distance between geometric entities at asserted c
onnectivities');
#40722=UNCERTAINTY_MEASURE_WITH_UNIT(LENGTH_MEASURE(0.01),#40735,
'DISTANCE_ACCURACY_VALUE',
'Maximum model space distance between geometric entities at asserted c
onnectivities');
#40723=UNCERTAINTY_MEASURE_WITH_UNIT(LENGTH_MEASURE(0.01),#40735,
'DISTANCE_ACCURACY_VALUE',
'Maximum model space distance between geometric entities at asserted c
onnectivities');
#40724=UNCERTAINTY_MEASURE_WITH_UNIT(LENGTH_MEASURE(0.01),#40735,
'DISTANCE_ACCURACY_VALUE',
'Maximum model space distance between geometric entities at asserted c
onnectivities');
#40725=(
GEOMETRIC_REPRESENTATION_CONTEXT(3)
GLOBAL_UNCERTAINTY_ASSIGNED_CONTEXT((#40715))
GLOBAL_UNIT_ASSIGNED_CONTEXT((#40735,#40737,#40738))
REPRESENTATION_CONTEXT('','3D')
);
#40726=(
GEOMETRIC_REPRESENTATION_CONTEXT(3)
GLOBAL_UNCERTAINTY_ASSIGNED_CONTEXT((#40716))
GLOBAL_UNIT_ASSIGNED_CONTEXT((#40735,#40737,#40738))
REPRESENTATION_CONTEXT('','3D')
);
#40727=(
GEOMETRIC_REPRESENTATION_CONTEXT(3)
GLOBAL_UNCERTAINTY_ASSIGNED_CONTEXT((#40717))
GLOBAL_UNIT_ASSIGNED_CONTEXT((#40735,#40737,#40738))
REPRESENTATION_CONTEXT('','3D')
);
#40728=(
GEOMETRIC_REPRESENTATION_CONTEXT(3)
GLOBAL_UNCERTAINTY_ASSIGNED_CONTEXT((#40718))
GLOBAL_UNIT_ASSIGNED_CONTEXT((#40735,#40737,#40738))
REPRESENTATION_CONTEXT('','3D')
);
#40729=(
GEOMETRIC_REPRESENTATION_CONTEXT(3)
GLOBAL_UNCERTAINTY_ASSIGNED_CONTEXT((#40719))
GLOBAL_UNIT_ASSIGNED_CONTEXT((#40735,#40737,#40738))
REPRESENTATION_CONTEXT('','3D')
);
#40730=(
GEOMETRIC_REPRESENTATION_CONTEXT(3)
GLOBAL_UNCERTAINTY_ASSIGNED_CONTEXT((#40720))
GLOBAL_UNIT_ASSIGNED_CONTEXT((#40735,#40737,#40738))
REPRESENTATION_CONTEXT('','3D')
);
#40731=(
GEOMETRIC_REPRESENTATION_CONTEXT(3)
GLOBAL_UNCERTAINTY_ASSIGNED_CONTEXT((#40721))
GLOBAL_UNIT_ASSIGNED_CONTEXT((#40735,#40737,#40738))
REPRESENTATION_CONTEXT('','3D')
);
#40732=(
GEOMETRIC_REPRESENTATION_CONTEXT(3)
GLOBAL_UNCERTAINTY_ASSIGNED_CONTEXT((#40722))
GLOBAL_UNIT_ASSIGNED_CONTEXT((#40735,#40737,#40738))
REPRESENTATION_CONTEXT('','3D')
);
#40733=(
GEOMETRIC_REPRESENTATION_CONTEXT(3)
GLOBAL_UNCERTAINTY_ASSIGNED_CONTEXT((#40723))
GLOBAL_UNIT_ASSIGNED_CONTEXT((#40735,#40737,#40738))
REPRESENTATION_CONTEXT('','3D')
);
#40734=(
GEOMETRIC_REPRESENTATION_CONTEXT(3)
GLOBAL_UNCERTAINTY_ASSIGNED_CONTEXT((#40724))
GLOBAL_UNIT_ASSIGNED_CONTEXT((#40735,#40737,#40738))
REPRESENTATION_CONTEXT('','3D')
);
#40735=(
LENGTH_UNIT()
NAMED_UNIT(*)
SI_UNIT(.MILLI.,.METRE.)
);
#40736=(
LENGTH_UNIT()
NAMED_UNIT(*)
SI_UNIT($,.METRE.)
);
#40737=(
NAMED_UNIT(*)
PLANE_ANGLE_UNIT()
SI_UNIT($,.RADIAN.)
);
#40738=(
NAMED_UNIT(*)
SI_UNIT($,.STERADIAN.)
SOLID_ANGLE_UNIT()
);
#40739=SHAPE_DEFINITION_REPRESENTATION(#40748,#40765);
#40740=SHAPE_DEFINITION_REPRESENTATION(#40749,#40766);
#40741=SHAPE_DEFINITION_REPRESENTATION(#40750,#40767);
#40742=SHAPE_DEFINITION_REPRESENTATION(#40751,#40768);
#40743=SHAPE_DEFINITION_REPRESENTATION(#40752,#40769);
#40744=SHAPE_DEFINITION_REPRESENTATION(#40753,#40770);
#40745=SHAPE_DEFINITION_REPRESENTATION(#40754,#40771);
#40746=SHAPE_DEFINITION_REPRESENTATION(#40755,#40772);
#40747=SHAPE_DEFINITION_REPRESENTATION(#40756,#40773);
#40748=PRODUCT_DEFINITION_SHAPE('',$,#40775);
#40749=PRODUCT_DEFINITION_SHAPE('',$,#40776);
#40750=PRODUCT_DEFINITION_SHAPE('',$,#40777);
#40751=PRODUCT_DEFINITION_SHAPE('',$,#40778);
#40752=PRODUCT_DEFINITION_SHAPE('',$,#40779);
#40753=PRODUCT_DEFINITION_SHAPE('',$,#40780);
#40754=PRODUCT_DEFINITION_SHAPE('',$,#40781);
#40755=PRODUCT_DEFINITION_SHAPE('',$,#40782);
#40756=PRODUCT_DEFINITION_SHAPE('',$,#40783);
#40757=PRODUCT_DEFINITION_SHAPE($,$,#35);
#40758=PRODUCT_DEFINITION_SHAPE($,$,#36);
#40759=PRODUCT_DEFINITION_SHAPE($,$,#37);
#40760=PRODUCT_DEFINITION_SHAPE($,$,#38);
#40761=PRODUCT_DEFINITION_SHAPE($,$,#39);
#40762=PRODUCT_DEFINITION_SHAPE($,$,#40);
#40763=PRODUCT_DEFINITION_SHAPE($,$,#41);
#40764=PRODUCT_DEFINITION_SHAPE($,$,#42);
#40765=SHAPE_REPRESENTATION('',(#3264,#3474,#3475,#3476,#3477,#3478,#3479,
#3480,#3481),#40725);
#40766=SHAPE_REPRESENTATION('',(#3265),#40726);
#40767=SHAPE_REPRESENTATION('',(#3284),#40727);
#40768=SHAPE_REPRESENTATION('',(#3299),#40728);
#40769=SHAPE_REPRESENTATION('',(#3320),#40729);
#40770=SHAPE_REPRESENTATION('',(#3340),#40730);
#40771=SHAPE_REPRESENTATION('',(#3351),#40731);
#40772=SHAPE_REPRESENTATION('',(#3402),#40732);
#40773=SHAPE_REPRESENTATION('',(#3423),#40733);
#40774=PRODUCT_DEFINITION_CONTEXT('part definition',#40803,'design');
#40775=PRODUCT_DEFINITION('BR-109','BR-109',#40784,#40774);
#40776=PRODUCT_DEFINITION('Ball_Stud','Ball_Stud_left',#40785,#40774);
#40777=PRODUCT_DEFINITION('Body','Body',#40786,#40774);
#40778=PRODUCT_DEFINITION('Nut','Nut',#40787,#40774);
#40779=PRODUCT_DEFINITION('Ball_Stud (1)','Ball_Stud_right',#40788,#40774);
#40780=PRODUCT_DEFINITION('Rod','Rod',#40789,#40774);
#40781=PRODUCT_DEFINITION('Screw','Screw',#40790,#40774);
#40782=PRODUCT_DEFINITION('Nut (1)','Nut_right',#40791,#40774);
#40783=PRODUCT_DEFINITION('Screw (1)','Screw_right',#40792,#40774);
#40784=PRODUCT_DEFINITION_FORMATION('',$,#40805);
#40785=PRODUCT_DEFINITION_FORMATION('',$,#40806);
#40786=PRODUCT_DEFINITION_FORMATION('',$,#40807);
#40787=PRODUCT_DEFINITION_FORMATION('',$,#40808);
#40788=PRODUCT_DEFINITION_FORMATION('',$,#40809);
#40789=PRODUCT_DEFINITION_FORMATION('',$,#40810);
#40790=PRODUCT_DEFINITION_FORMATION('',$,#40811);
#40791=PRODUCT_DEFINITION_FORMATION('',$,#40812);
#40792=PRODUCT_DEFINITION_FORMATION('',$,#40813);
#40793=PRODUCT_RELATED_PRODUCT_CATEGORY('BR-109','BR-109',(#40805));
#40794=PRODUCT_RELATED_PRODUCT_CATEGORY('Ball_Stud_left',
'Ball_Stud_left',(#40806));
#40795=PRODUCT_RELATED_PRODUCT_CATEGORY('Body','Body',(#40807));
#40796=PRODUCT_RELATED_PRODUCT_CATEGORY('Nut','Nut',(#40808));
#40797=PRODUCT_RELATED_PRODUCT_CATEGORY('Ball_Stud_right',
'Ball_Stud_right',(#40809));
#40798=PRODUCT_RELATED_PRODUCT_CATEGORY('Rod','Rod',(#40810));
#40799=PRODUCT_RELATED_PRODUCT_CATEGORY('Screw','Screw',(#40811));
#40800=PRODUCT_RELATED_PRODUCT_CATEGORY('Nut_right','Nut_right',(#40812));
#40801=PRODUCT_RELATED_PRODUCT_CATEGORY('Screw_right','Screw_right',(#40813));
#40802=APPLICATION_PROTOCOL_DEFINITION('international standard',
'automotive_design',2009,#40803);
#40803=APPLICATION_CONTEXT(
'Core Data for Automotive Mechanical Design Process');
#40804=PRODUCT_CONTEXT('part definition',#40803,'mechanical');
#40805=PRODUCT('BR-109','BR-109',$,(#40804));
#40806=PRODUCT('Ball_Stud','Ball_Stud_left',$,(#40804));
#40807=PRODUCT('Body','Body',$,(#40804));
#40808=PRODUCT('Nut','Nut',$,(#40804));
#40809=PRODUCT('Ball_Stud (1)','Ball_Stud_right',$,(#40804));
#40810=PRODUCT('Rod','Rod',$,(#40804));
#40811=PRODUCT('Screw','Screw',$,(#40804));
#40812=PRODUCT('Nut (1)','Nut_right',$,(#40804));
#40813=PRODUCT('Screw (1)','Screw_right',$,(#40804));
#40814=PRESENTATION_STYLE_ASSIGNMENT((#40817));
#40815=PRESENTATION_STYLE_ASSIGNMENT((#40818));
#40816=PRESENTATION_STYLE_ASSIGNMENT((#40819));
#40817=SURFACE_STYLE_USAGE(.BOTH.,#40820);
#40818=SURFACE_STYLE_USAGE(.BOTH.,#40821);
#40819=SURFACE_STYLE_USAGE(.BOTH.,#40822);
#40820=SURFACE_SIDE_STYLE('',(#40823));
#40821=SURFACE_SIDE_STYLE('',(#40824));
#40822=SURFACE_SIDE_STYLE('',(#40825));
#40823=SURFACE_STYLE_FILL_AREA(#40826);
#40824=SURFACE_STYLE_FILL_AREA(#40827);
#40825=SURFACE_STYLE_FILL_AREA(#40828);
#40826=FILL_AREA_STYLE('Steel - Satin',(#40829));
#40827=FILL_AREA_STYLE('Opaque(203,203,203)',(#40830));
#40828=FILL_AREA_STYLE('Opaque(67,67,67)',(#40831));
#40829=FILL_AREA_STYLE_COLOUR('Steel - Satin',#40832);
#40830=FILL_AREA_STYLE_COLOUR('Opaque(203,203,203)',#40833);
#40831=FILL_AREA_STYLE_COLOUR('Opaque(67,67,67)',#40834);
#40832=COLOUR_RGB('Steel - Satin', 0.09019608, 0.27058824, 0.51372549);
#40833=COLOUR_RGB('Opaque(203,203,203)', 0.09019608, 0.27058824, 0.51372549);
#40834=COLOUR_RGB('Opaque(67,67,67)', 0.66274510, 0.83137255, 0.94901961);
ENDSEC;
END-ISO-10303-21;
